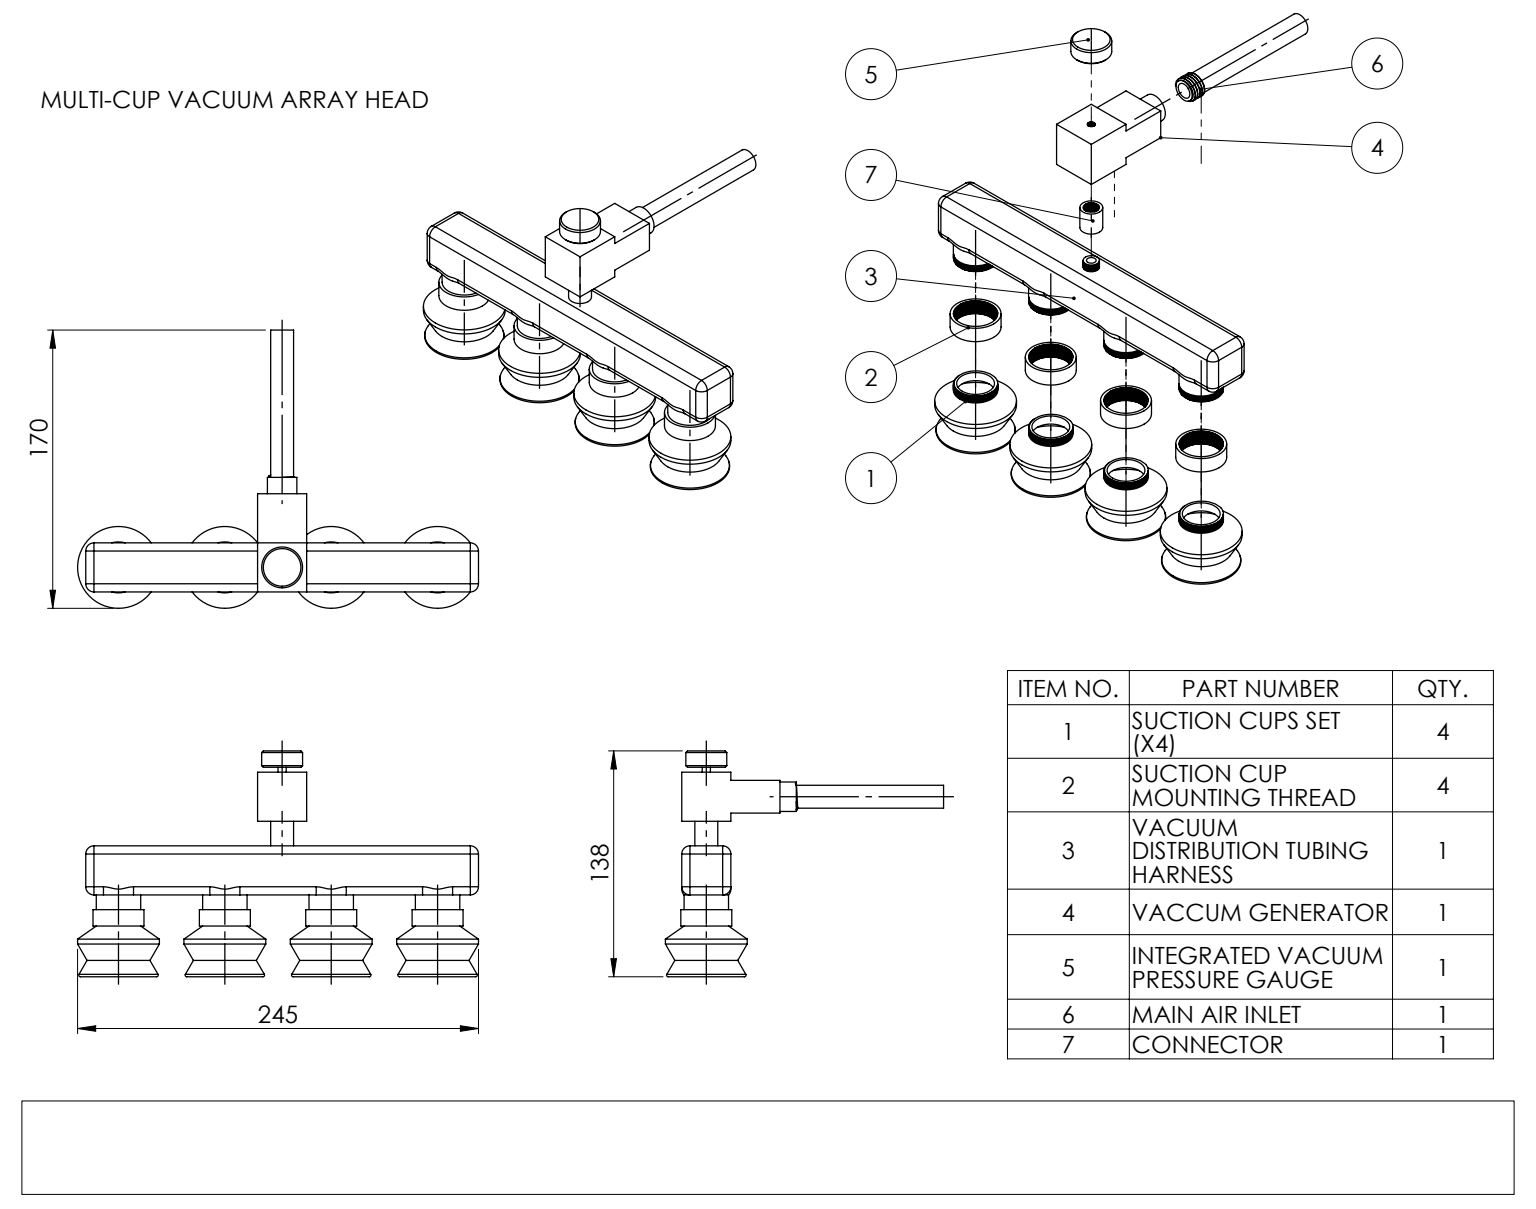
ISO-10303-21;
HEADER;
FILE_DESCRIPTION (('STEP AP214'),
    '1' );
FILE_NAME ('BR-008',
    '2026-10-01T14:18:43',
    ( '' ),
    ( '' ),
    'SwSTEP 2.0',
    'SolidWorks 2026',
    '' );
FILE_SCHEMA (( 'AUTOMOTIVE_DESIGN' ));
ENDSEC;

DATA;
#1 = ORIENTED_EDGE ( 'NONE', *, *, #27439, .T. ) ;
#2 = CARTESIAN_POINT ( 'NONE',  ( 94.99999999999995737, 83.93750000000001421, -2.071067811865491048 ) ) ;
#3 = CARTESIAN_POINT ( 'NONE',  ( 103.1528011352953484, 93.43749999863440792, -3.152801135295366208 ) ) ;
#4 = ORIENTED_EDGE ( 'NONE', *, *, #23222, .F. ) ;
#5 = CARTESIAN_POINT ( 'NONE',  ( 95.67376207875069838, 115.9545556584642867, -49.30000000000000426 ) ) ;
#6 = CARTESIAN_POINT ( 'NONE',  ( 59.55508561352770158, 34.55078125108393294, 13.14518615778179722 ) ) ;
#7 = ORIENTED_EDGE ( 'NONE', *, *, #7284, .F. ) ;
#8 = CARTESIAN_POINT ( 'NONE',  ( 13.57481594606304753, 32.71523437500000142, -5.622872871577873966 ) ) ;
#9 = CARTESIAN_POINT ( 'NONE',  ( 101.8468681455906903, 4.458734125000016313, 4.375000001365592084 ) ) ;
#10 = EDGE_CURVE ( 'NONE', #23304, #14872, #10315, .T. ) ;
#11 = VERTEX_POINT ( 'NONE', #12909 ) ;
#12 = CARTESIAN_POINT ( 'NONE',  ( 13.14518615778179544, 34.00507812608393721, -1.609821015232357215E-15 ) ) ;
#13 = CARTESIAN_POINT ( 'NONE',  ( -5.444914386472299306, 39.31328125108394289, 13.14518615778179722 ) ) ;
#14 = CARTESIAN_POINT ( 'NONE',  ( 185.4011555911795597, 37.22968750216787726, 9.598844408820459861 ) ) ;
#15 = CARTESIAN_POINT ( 'NONE',  ( 5.444914386472302859, 36.83281250108392868, 13.14518615778179189 ) ) ;
#16 = CARTESIAN_POINT ( 'NONE',  ( 94.99999999999995737, 1.387778780781445676E-14, 4.999999999999999112 ) ) ;
#17 = CARTESIAN_POINT ( 'NONE',  ( 198.0446094569239790, 53.89089363584123049, 14.99999999999994671 ) ) ;
#18 = CARTESIAN_POINT ( 'NONE',  ( 143.1451861577818363, 36.43593750108394147, -5.444914386472297529 ) ) ;
#19 = ORIENTED_EDGE ( 'NONE', *, *, #9159, .T. ) ;
#21 = VECTOR ( 'NONE', #21803, 1000.000000000000000 ) ;
#20 = CARTESIAN_POINT ( 'NONE',  ( 13.14518615778179544, 37.97382812608393721, -1.609821015232357215E-15 ) ) ;
#22 = CARTESIAN_POINT ( 'NONE',  ( 143.1451861577818079, 35.39414062608393152, -1.609821015232357215E-15 ) ) ;
#23 = CARTESIAN_POINT ( 'NONE',  ( 65.00000000000000000, 34.84843749999999574, 13.57481594606304576 ) ) ;
#24 = CARTESIAN_POINT ( 'NONE',  ( 130.0000000000000000, -7.395377635281828788, -1.503427012513233026E-14 ) ) ;
#25 = CARTESIAN_POINT ( 'NONE',  ( 95.54126587499996504, 1.387778780781445676E-14, 10.68750000136559208 ) ) ;
#26 = CARTESIAN_POINT ( 'NONE',  ( 99.99999999999998579, 130.0000000000000000, 0.5000000000000034417 ) ) ;
#27 = CARTESIAN_POINT ( 'NONE',  ( 99.99999999999995737, -4.458734124999988779, 1.687500001365591418 ) ) ;
#28 = CARTESIAN_POINT ( 'NONE',  ( 104.9952793366501851, 116.8754121666685393, -49.82500000273120122 ) ) ;
#29 = CARTESIAN_POINT ( 'NONE',  ( -8.312177448680279460E-16, 39.31328125216787583, -13.57481594606304576 ) ) ;
#30 = CARTESIAN_POINT ( 'NONE',  ( 99.99999999999995737, 80.00000000000000000, -1.387778780781445676E-14 ) ) ;
#31 = CARTESIAN_POINT ( 'NONE',  ( 93.46109445667489979, 105.2492070361643215, -47.42499999726882720 ) ) ;
#32 = CARTESIAN_POINT ( 'NONE',  ( -9.295050272127046043, 35.89023437608393152, -9.295050272127046043 ) ) ;
#33 = CARTESIAN_POINT ( 'NONE',  ( 95.00472066334982912, 103.1245878333314323, -47.57499999726882578 ) ) ;
#34 = VERTEX_POINT ( 'NONE', #6384 ) ;
#35 = CARTESIAN_POINT ( 'NONE',  ( 102.0669872999999797, 124.3500000010924822, -9.794112055954760458E-15 ) ) ;
#36 =( BOUNDED_CURVE ( )  B_SPLINE_CURVE ( 2, ( #22936, #3397, #12350, #21068, #12069, #998, #12204, #16222, #18653 ),
 .UNSPECIFIED., .F., .F. ) 
 B_SPLINE_CURVE_WITH_KNOTS ( ( 3, 2, 2, 2, 3 ),
 ( 0.5208333333333332593, 0.5312499999999997780, 0.5416666666666664076, 0.5520833333333330373, 0.5624999999999996669 ),
 .UNSPECIFIED. ) 
 CURVE ( )  GEOMETRIC_REPRESENTATION_ITEM ( )  RATIONAL_B_SPLINE_CURVE ( ( 1.000000000000000888, 0.9238795325112859613, 1.000000000000000000, 0.9238795325112867385, 1.000000000000000000, 0.9238795325112867385, 1.000000000000000000, 0.9238795325112891810, 0.9999999999999975575 ) ) 
 REPRESENTATION_ITEM ( '' )  );
#37 = CARTESIAN_POINT ( 'NONE',  ( 102.0669872999999797, 123.3500000010924680, -9.794112055954760458E-15 ) ) ;
#38 = LINE ( 'NONE', #22552, #12466 ) ;
#39 = CARTESIAN_POINT ( 'NONE',  ( 195.0000000000000000, 37.97382812608393721, -13.14518615778179544 ) ) ;
#40 = ORIENTED_EDGE ( 'NONE', *, *, #17022, .F. ) ;
#41 = CYLINDRICAL_SURFACE ( 'NONE', #26554, 13.57481594606304576 ) ;
#42 = CARTESIAN_POINT ( 'NONE',  ( -13.36000105192242060, 40.87597656304196647, 0.000000000000000000 ) ) ;
#43 = CARTESIAN_POINT ( 'NONE',  ( 104.4587341249999781, -1.846868145590721655, 14.12500000136559208 ) ) ;
#44 = EDGE_CURVE ( 'NONE', #13519, #7822, #26113, .T. ) ;
#45 = ORIENTED_EDGE ( 'NONE', *, *, #19075, .T. ) ;
#46 = CARTESIAN_POINT ( 'NONE',  ( 93.00000000000001421, 112.2744378736303332, -50.10000000000000142 ) ) ;
#47 = AXIS2_PLACEMENT_3D ( 'NONE', #20882, #18604, #27308 ) ;
#48 = CARTESIAN_POINT ( 'NONE',  ( -13.14518615778179900, 40.50390625108394005, -5.444914386472297529 ) ) ;
#49 = CARTESIAN_POINT ( 'NONE',  ( 97.93301269999999192, 123.9000000010924794, -0.8561741729129505041 ) ) ;
#50 = CARTESIAN_POINT ( 'NONE',  ( 143.1451861577818079, 39.31328125108392868, 5.444914386472293977 ) ) ;
#51 = CYLINDRICAL_SURFACE ( 'NONE', #259, 5.000000000000004441 ) ;
#52 = APPLICATION_CONTEXT ( 'automotive_design' ) ;
#53 = CARTESIAN_POINT ( 'NONE',  ( 103.5355339059327235, 93.74999999726881583, 3.535533905932724874 ) ) ;
#54 = CARTESIAN_POINT ( 'NONE',  ( 78.14518615778179367, 39.51171875108392584, 5.444914386472293977 ) ) ;
#55 = FACE_OUTER_BOUND ( 'NONE', #22673, .T. ) ;
#56 = CIRCLE ( 'NONE', #18273, 5.000000000000000000 ) ;
#57 = CARTESIAN_POINT ( 'NONE',  ( 181.8548138422181921, 33.65781250108393152, 5.444914386472304635 ) ) ;
#58 = VERTEX_POINT ( 'NONE', #14643 ) ;
#59 = ORIENTED_EDGE ( 'NONE', *, *, #2461, .T. ) ;
#60 = CARTESIAN_POINT ( 'NONE',  ( -13.14518615778179900, 39.11484375108394573, -5.444914386472297529 ) ) ;
#61 = CARTESIAN_POINT ( 'NONE',  ( 103.1528011352953342, -3.152801135295355106, 10.06250000136559386 ) ) ;
#62 = CARTESIAN_POINT ( 'NONE',  ( 51.85481384221820633, 38.96601562608393721, 0.000000000000000000 ) ) ;
#63 = CARTESIAN_POINT ( 'NONE',  ( 99.99999999999995737, 80.18750000136559208, -4.458734125000016313 ) ) ;
#64 = CARTESIAN_POINT ( 'NONE',  ( 189.5550856135277229, 39.61093750108393152, -13.14518615778179722 ) ) ;
#65 = CARTESIAN_POINT ( 'NONE',  ( -8.049105076161786076E-16, 38.96601562608393721, -13.14518615778179544 ) ) ;
#66 = CARTESIAN_POINT ( 'NONE',  ( 187.8845096081555823, 49.99999999945637796, 11.58166858714721492 ) ) ;
#67 =( BOUNDED_CURVE ( )  B_SPLINE_CURVE ( 2, ( #19739, #26449, #6767, #8908, #2228, #15452, #13444, #6906, #10892, #17316, #24023, #2505, #15595, #2083, #2648, #15160, #20032, #19600, #512, #9193, #17887, #26593, #10752, #19463, #28160, #8627, #4357, #13014, #83, #8766, #26155, #15308, #18836, #13875, #8143, #13592, #5879, #15877, #16700, #11735, #22314, #20460, #11453, #942, #10262, #12398, #21119, #26883, #22601, #3070, #26736, #2788, #23265, #20986, #13733, #1606, #24872, #14549, #18972, #27680, #27543, #16017, #5355, #24587, #4929, #7329, #18022, #20174, #9613, #9328, #8000, #3738, #7180, #1467, #25399, #5069, #16837, #655, #16165, #22457, #2923, #10123, #18316, #14410, #27025, #11593, #20313, #7470, #800, #9469, #23126, #18171, #3601, #24731, #5211, #12261, #10683, #8842, #23398, #23956, #8558 ),
 .UNSPECIFIED., .F., .F. ) 
 B_SPLINE_CURVE_WITH_KNOTS ( ( 3, 2, 2, 2, 2, 2, 2, 2, 2, 2, 2, 2, 2, 2, 2, 2, 2, 2, 2, 2, 2, 2, 2, 2, 2, 2, 2, 2, 2, 2, 2, 2, 2, 2, 2, 2, 2, 2, 2, 2, 2, 2, 2, 2, 2, 2, 2, 2, 2, 2, 3 ),
 ( 0.000000000000000000, 0.02000000000000000042, 0.04000000000000000083, 0.05999999999999999778, 0.08000000000000000167, 0.1000000000000000056, 0.1199999999999999956, 0.1400000000000000133, 0.1600000000000000033, 0.1799999999999999933, 0.2000000000000000111, 0.2200000000000000011, 0.2399999999999999911, 0.2600000000000000089, 0.2800000000000000266, 0.2999999999999999889, 0.3200000000000000067, 0.3400000000000000244, 0.3599999999999999867, 0.3800000000000000044, 0.4000000000000000222, 0.4199999999999999845, 0.4400000000000000022, 0.4600000000000000200, 0.4799999999999999822, 0.5000000000000000000, 0.5200000000000000178, 0.5400000000000000355, 0.5600000000000000533, 0.5799999999999999600, 0.5999999999999999778, 0.6199999999999999956, 0.6400000000000000133, 0.6600000000000000311, 0.6800000000000000488, 0.6999999999999999556, 0.7199999999999999734, 0.7399999999999999911, 0.7600000000000000089, 0.7800000000000000266, 0.8000000000000000444, 0.8199999999999999512, 0.8399999999999999689, 0.8599999999999999867, 0.8800000000000000044, 0.9000000000000000222, 0.9200000000000000400, 0.9399999999999999467, 0.9599999999999999645, 0.9799999999999999822, 1.000000000000000000 ),
 .UNSPECIFIED. ) 
 CURVE ( )  GEOMETRIC_REPRESENTATION_ITEM ( )  RATIONAL_B_SPLINE_CURVE ( ( 1.000000000000000000, 0.9510565162951535312, 1.000000000000000000, 0.9510565162951535312, 1.000000000000000000, 0.9510565162951535312, 1.000000000000000000, 0.9510565162951535312, 1.000000000000000000, 0.9510565162951535312, 1.000000000000000000, 0.9510565162951535312, 1.000000000000000000, 0.9510565162951535312, 1.000000000000000000, 0.9510565162951535312, 1.000000000000000000, 0.9510565162951535312, 1.000000000000000000, 0.9510565162951535312, 1.000000000000000000, 0.9510565162951535312, 1.000000000000000000, 0.9510565162951535312, 1.000000000000000000, 0.9510565162951535312, 1.000000000000000000, 0.9510565162951535312, 1.000000000000000000, 0.9510565162951535312, 1.000000000000000000, 0.9510565162951535312, 1.000000000000000000, 0.9510565162951535312, 1.000000000000000000, 0.9510565162951535312, 1.000000000000000000, 0.9510565162951535312, 1.000000000000000000, 0.9510565162951535312, 1.000000000000000000, 0.9510565162951535312, 1.000000000000000000, 0.9510565162951535312, 1.000000000000000000, 0.9510565162951535312, 1.000000000000000000, 0.9510565162951535312, 1.000000000000000000, 0.9510565162951535312, 1.000000000000000000, 0.9510565162951535312, 1.000000000000000000, 0.9510565162951535312, 1.000000000000000000, 0.9510565162951535312, 1.000000000000000000, 0.9510565162951535312, 1.000000000000000000, 0.9510565162951535312, 1.000000000000000000, 0.9510565162951535312, 1.000000000000000000, 0.9510565162951535312, 1.000000000000000000, 0.9510565162951535312, 1.000000000000000000, 0.9510565162951535312, 1.000000000000000000, 0.9510565162951535312, 1.000000000000000000, 0.9510565162951535312, 1.000000000000000000, 0.9510565162951535312, 1.000000000000000000, 0.9510565162951535312, 1.000000000000000000, 0.9510565162951535312, 1.000000000000000000, 0.9510565162951535312, 1.000000000000000000, 0.9510565162951535312, 1.000000000000000000, 0.9510565162951535312, 1.000000000000000000, 0.9510565162951535312, 1.000000000000000000, 0.9510565162951535312, 1.000000000000000000, 0.9510565162951535312, 1.000000000000000000, 0.9510565162951535312, 1.000000000000000000, 0.9510565162951535312, 1.000000000000000000, 0.9510565162951535312, 1.000000000000000000, 0.9510565162951535312, 1.000000000000000000, 0.9510565162951535312, 1.000000000000000000 ) ) 
 REPRESENTATION_ITEM ( '' )  );
#68 = CARTESIAN_POINT ( 'NONE',  ( 2.493653234604083739E-15, 38.02343749999999289, 13.57481594606304576 ) ) ;
#69 = CARTESIAN_POINT ( 'NONE',  ( 97.50236033167490746, 102.3130555110000159, -55.22499999726881725 ) ) ;
#70 = ORIENTED_EDGE ( 'NONE', *, *, #20702, .F. ) ;
#71 = EDGE_CURVE ( 'NONE', #7474, #9199, #1741, .T. ) ;
#72 = CARTESIAN_POINT ( 'NONE',  ( 13.57481594606304931, 38.17226562499999432, 5.622872871577869525 ) ) ;
#73 = CARTESIAN_POINT ( 'NONE',  ( 5.444914386472297529, 37.92421875108392726, -13.14518615778179900 ) ) ;
#74 = CARTESIAN_POINT ( 'NONE',  ( 99.99999999999995737, -4.999999999999990230, 1.375000002731184612 ) ) ;
#75 = CARTESIAN_POINT ( 'NONE',  ( 143.1451861577818079, 34.79882812608394005, -1.609821015232357215E-15 ) ) ;
#76 = CARTESIAN_POINT ( 'NONE',  ( 59.55508561352770158, 32.76484375108393010, 13.14518615778179722 ) ) ;
#77 = CARTESIAN_POINT ( 'NONE',  ( 208.1451861577817795, 38.71796875108393721, 5.444914386472293977 ) ) ;
#78 = CARTESIAN_POINT ( 'NONE',  ( 9.295050272127047819, 32.91367187608393152, 9.295050272127046043 ) ) ;
#79 = CARTESIAN_POINT ( 'NONE',  ( 134.5715916325255250, 51.44262710532316873, -14.99999999999934452 ) ) ;
#80 = EDGE_CURVE ( 'NONE', #16509, #7689, #8629, .T. ) ;
#81 = CARTESIAN_POINT ( 'NONE',  ( 99.99999999999998579, 110.0000000000000000, -145.0000000000000284 ) ) ;
#82 = CARTESIAN_POINT ( 'NONE',  ( -9.180175813647991845, 50.00000000000000000, 9.999999999999998224 ) ) ;
#83 = CARTESIAN_POINT ( 'NONE',  ( 93.46109445667491400, 114.7507929638356785, -51.32500000273120122 ) ) ;
#84 = EDGE_CURVE ( 'NONE', #861, #22018, #1572, .T. ) ;
#85 = CARTESIAN_POINT ( 'NONE',  ( 13.14518615778179544, 33.80664062608393294, -1.609821015232357215E-15 ) ) ;
#86 = CARTESIAN_POINT ( 'NONE',  ( 84.99999999999998579, 100.0000000000000000, -15.00000000000000533 ) ) ;
#87 = CARTESIAN_POINT ( 'NONE',  ( 101.7677669529663547, 123.8000000021849587, 1.767766952966350891 ) ) ;
#88 = EDGE_CURVE ( 'NONE', #26327, #25494, #13051, .T. ) ;
#89 = CARTESIAN_POINT ( 'NONE',  ( -5.622872871577804688, 36.48554687716787726, 13.57481594606311504 ) ) ;
#90 = SURFACE_STYLE_USAGE ( .BOTH. , #4222 ) ;
#91 = CARTESIAN_POINT ( 'NONE',  ( 98.15313185440925281, 4.458734125000016313, 7.250000001365591196 ) ) ;
#92 = ORIENTED_EDGE ( 'NONE', *, *, #1447, .F. ) ;
#93 = CARTESIAN_POINT ( 'NONE',  ( 102.0669872999999797, 122.5500000010924850, -9.794112055954760458E-15 ) ) ;
#94 = CARTESIAN_POINT ( 'NONE',  ( 101.8468681455906903, -4.458734124999987891, 10.75000000136559208 ) ) ;
#95 = LINE ( 'NONE', #11320, #20973 ) ;
#96 = ADVANCED_FACE ( 'NONE', ( #24479 ), #13627, .T. ) ;
#97 = CARTESIAN_POINT ( 'NONE',  ( 13.14518615778179544, 38.56914062608393579, -1.609821015232357215E-15 ) ) ;
#98 = CARTESIAN_POINT ( 'NONE',  ( 120.4011555911795455, 38.61875000216787157, -9.598844408820458085 ) ) ;
#99 = CARTESIAN_POINT ( 'NONE',  ( 103.1528011352953342, 80.06250000136559208, 3.152801135295355106 ) ) ;
#100 = CARTESIAN_POINT ( 'NONE',  ( 78.14518615778179367, 34.05468750108394005, -5.444914386472297529 ) ) ;
#101 = CARTESIAN_POINT ( 'NONE',  ( 108.0825317500000011, 112.6261737610028320, -50.02500000273118275 ) ) ;
#102 = CARTESIAN_POINT ( 'NONE',  ( 103.5355339059327093, 3.535533905932755072, 11.62500000000000000 ) ) ;
#103 = CARTESIAN_POINT ( 'NONE',  ( 214.9999999999999716, 80.00000000000000000, 9.999999999999946709 ) ) ;
#104 = CARTESIAN_POINT ( 'NONE',  ( 95.54126587499996504, 1.387778780781445676E-14, 0.6875000013655923059 ) ) ;
#105 = CARTESIAN_POINT ( 'NONE',  ( 143.5748159460630404, 39.06523437499998863, -5.622872871577873077 ) ) ;
#106 = ORIENTED_EDGE ( 'NONE', *, *, #13267, .T. ) ;
#107 = DIRECTION ( 'NONE',  ( -1.000000000000000000, 0.000000000000000000, 0.000000000000000000 ) ) ;
#108 = CARTESIAN_POINT ( 'NONE',  ( 9.295050272127046043, 38.07304687608393579, -9.295050272127046043 ) ) ;
#109 = CARTESIAN_POINT ( 'NONE',  ( -5.622872871577873077, 36.18789062716787441, -13.57481594606304753 ) ) ;
#110 = CARTESIAN_POINT ( 'NONE',  ( 143.1451861577818079, 37.82500000108392868, -5.444914386472297529 ) ) ;
#111 = CARTESIAN_POINT ( 'NONE',  ( 51.42518405393695957, 33.16171875216787868, 0.000000000000000000 ) ) ;
#112 = EDGE_CURVE ( 'NONE', #21487, #10978, #25380, .T. ) ;
#113 = DIRECTION ( 'NONE',  ( 0.000000000000000000, 0.000000000000000000, 1.000000000000000000 ) ) ;
#114 = CARTESIAN_POINT ( 'NONE',  ( 13.57481594606304931, 32.71523437716787441, 5.622872871577869525 ) ) ;
#115 = CARTESIAN_POINT ( 'NONE',  ( 102.0710678118654329, 5.000000000000018652, 4.687500000000000000 ) ) ;
#116 = EDGE_CURVE ( 'NONE', #24967, #25660, #21271, .T. ) ;
#117 = CARTESIAN_POINT ( 'NONE',  ( 185.7049497278729575, 34.10429687608393579, -9.295050272127046043 ) ) ;
#118 = EDGE_CURVE ( 'NONE', #27220, #19908, #1908, .T. ) ;
#119 = VECTOR ( 'NONE', #9370, 1000.000000000000000 ) ;
#120 = CARTESIAN_POINT ( 'NONE',  ( 104.9999999999999716, 92.93749999999998579, 2.071067811865467956 ) ) ;
#121 = CARTESIAN_POINT ( 'NONE',  ( 181.4251840539369596, 37.97382812716787726, 5.622872871577880183 ) ) ;
#122 = LINE ( 'NONE', #8807, #24532 ) ;
#123 = CARTESIAN_POINT ( 'NONE',  ( 92.99999999999998579, 110.0000000000000000, -48.49999999453763877 ) ) ;
#124 = CARTESIAN_POINT ( 'NONE',  ( 13.57481594606304576, 37.42812499999999432, -1.662435489736055892E-15 ) ) ;
#125 = CARTESIAN_POINT ( 'NONE',  ( 99.99999999999998579, 117.3602355696678643, -54.50000000000000000 ) ) ;
#126 = CARTESIAN_POINT ( 'NONE',  ( 5.444914386472297529, 36.53515625108393294, -13.14518615778179900 ) ) ;
#127 = CARTESIAN_POINT ( 'NONE',  ( 5.444914386472302859, 36.03906250108394005, 13.14518615778179189 ) ) ;
#128 = CARTESIAN_POINT ( 'NONE',  ( 195.0000000000000000, 35.24531249999999716, -13.57481594606304576 ) ) ;
#129 = CARTESIAN_POINT ( 'NONE',  ( 106.5389055433251002, 105.2492070361643215, -44.57500000273119412 ) ) ;
#130 = CARTESIAN_POINT ( 'NONE',  ( 104.3262379212492590, 115.9545556584642867, -45.20000000546237828 ) ) ;
#131 = CARTESIAN_POINT ( 'NONE',  ( 59.55508561352770158, 35.14609375108393152, 13.14518615778179722 ) ) ;
#132 = CARTESIAN_POINT ( 'NONE',  ( 104.4587341249999781, 1.846868145590750521, 4.000000001365592084 ) ) ;
#133 = CARTESIAN_POINT ( 'NONE',  ( 102.1631189606246295, 116.6573956140660897, -45.10000000546238397 ) ) ;
#134 = CARTESIAN_POINT ( 'NONE',  ( 98.15313185440925281, 94.99999999863439371, 4.458734124999979898 ) ) ;
#135 = CARTESIAN_POINT ( 'NONE',  ( 97.93294022916485631, 122.9999999999999858, -0.1348184704668160261 ) ) ;
#136 = CARTESIAN_POINT ( 'NONE',  ( 13.57481594606304753, 36.68398437499999432, -5.622872871577873077 ) ) ;
#137 = CARTESIAN_POINT ( 'NONE',  ( 130.0000000000000000, 36.58476562608393579, -13.14518615778179544 ) ) ;
#138 = VERTEX_POINT ( 'NONE', #3105 ) ;
#139 = ORIENTED_EDGE ( 'NONE', *, *, #6013, .F. ) ;
#140 = CARTESIAN_POINT ( 'NONE',  ( 99.99999999999995737, 84.75000000000000000, -5.000000000000018652 ) ) ;
#141 = CARTESIAN_POINT ( 'NONE',  ( 94.99999999999995737, 82.06250000273119838, -2.071067811865491048 ) ) ;
#142 = CARTESIAN_POINT ( 'NONE',  ( 96.84719886470463734, 92.93749999863440792, 3.152801135295351997 ) ) ;
#143 = CARTESIAN_POINT ( 'NONE',  ( 9.598844408820456309, 34.35234374999999574, -9.598844408820458085 ) ) ;
#144 = VERTEX_POINT ( 'NONE', #11771 ) ;
#145 = AXIS2_PLACEMENT_3D ( 'NONE', #183, #21567, #25834 ) ;
#146 = CARTESIAN_POINT ( 'NONE',  ( 99.99999999999997158, 102.6397644303321215, -52.50000000000000711 ) ) ;
#147 = CARTESIAN_POINT ( 'NONE',  ( 70.44491438647230552, 33.85625000108393579, 13.14518615778179189 ) ) ;
#148 = ORIENTED_EDGE ( 'NONE', *, *, #16828, .T. ) ;
#149 = CARTESIAN_POINT ( 'NONE',  ( -8.312177448680279460E-16, 32.96328125216787441, -13.57481594606304576 ) ) ;
#150 = CARTESIAN_POINT ( 'NONE',  ( 101.8468681455906903, -4.458734124999987891, 3.000000001365592528 ) ) ;
#151 = EDGE_CURVE ( 'NONE', #14316, #1074, #18349, .T. ) ;
#152 = VERTEX_POINT ( 'NONE', #22777 ) ;
#153 = CARTESIAN_POINT ( 'NONE',  ( 94.99999999999995737, 82.18750000273119838, 2.071067811865466624 ) ) ;
#154 = CARTESIAN_POINT ( 'NONE',  ( 13.14518615778179544, 38.76757812608393294, -1.609821015232357215E-15 ) ) ;
#155 = UNCERTAINTY_MEASURE_WITH_UNIT (LENGTH_MEASURE( 1.000000000000000082E-05 ), #20072, 'distance_accuracy_value', 'NONE');
#156 = CARTESIAN_POINT ( 'NONE',  ( 208.5748159460630120, 35.09648437716787583, 5.622872871577869525 ) ) ;
#157 =( BOUNDED_CURVE ( )  B_SPLINE_CURVE ( 2, ( #25854, #26427, #8886, #8604, #23721, #4618, #22006, #19716, #2060, #6886, #24002, #4059, #2483, #19859, #12721, #10593, #17292, #17435, #26134, #346, #10730, #19438, #6600, #9033, #21447, #25994, #1925, #6465, #15139, #2204, #10868, #19578, #62, #5047, #2628, #15857, #775, #22576, #24851, #11571, #920, #7307, #13712, #7161, #13851, #491, #24419, #5188, #9172, #22433, #27146, #631, #15994, #4908, #9447, #11713, #24566, #3045, #9307, #11289, #17864, #20289, #22720, #26569, #9590, #18004, #2902, #24709, #20438, #7598, #18294, #7021, #27000, #7447, #16143, #22292, #24280, #5330, #4761, #13994, #3187, #13569, #11857, #20579, #2768, #26861, #18147, #1062, #15716, #9732, #18437, #13421, #11432 ),
 .UNSPECIFIED., .F., .F. ) 
 B_SPLINE_CURVE_WITH_KNOTS ( ( 3, 2, 2, 2, 2, 2, 2, 2, 2, 2, 2, 2, 2, 2, 2, 2, 2, 2, 2, 2, 2, 2, 2, 2, 2, 2, 2, 2, 2, 2, 2, 2, 2, 2, 2, 2, 2, 2, 2, 2, 2, 2, 2, 2, 2, 2, 3 ),
 ( 0.000000000000000000, 0.01041666666666666609, 0.02083333333333333218, 0.03125000000000000000, 0.04166666666666666435, 0.05208333333333333565, 0.06250000000000000000, 0.07291666666666667129, 0.08333333333333332871, 0.09375000000000000000, 0.1041666666666666713, 0.1145833333333333287, 0.1250000000000000000, 0.1354166666666666574, 0.1458333333333333426, 0.1562500000000000278, 0.1666666666666666574, 0.1770833333333333426, 0.1875000000000000000, 0.1979166666666666574, 0.2083333333333333426, 0.2187499999999999722, 0.2291666666666666574, 0.2395833333333333426, 0.2500000000000000000, 0.2604166666666666852, 0.2708333333333333148, 0.2812500000000000000, 0.2916666666666666852, 0.3020833333333333148, 0.3125000000000000555, 0.3229166666666666852, 0.3333333333333333148, 0.3437500000000000000, 0.3541666666666666852, 0.3645833333333333148, 0.3750000000000000000, 0.3854166666666666852, 0.3958333333333333148, 0.4062500000000000000, 0.4166666666666666852, 0.4270833333333333148, 0.4374999999999999445, 0.4479166666666666852, 0.4583333333333333148, 0.4687500000000000000, 0.4779971559588573893 ),
 .UNSPECIFIED. ) 
 CURVE ( )  GEOMETRIC_REPRESENTATION_ITEM ( )  RATIONAL_B_SPLINE_CURVE ( ( 1.000000000000000000, 0.9238795325112867385, 1.000000000000000000, 0.9238795325112867385, 1.000000000000000000, 0.9238795325112867385, 1.000000000000000000, 0.9238795325112867385, 1.000000000000000000, 0.9238795325112867385, 1.000000000000000000, 0.9238795325112867385, 1.000000000000000000, 0.9238795325112867385, 1.000000000000000000, 0.9238795325112867385, 1.000000000000000000, 0.9238795325112867385, 1.000000000000000000, 0.9238795325112867385, 1.000000000000000000, 0.9238795325112867385, 1.000000000000000000, 0.9238795325112867385, 1.000000000000000000, 0.9238795325112867385, 1.000000000000000000, 0.9238795325112867385, 1.000000000000000000, 0.9238795325112867385, 1.000000000000000000, 0.9238795325112867385, 1.000000000000000000, 0.9238795325112867385, 1.000000000000000000, 0.9238795325112867385, 1.000000000000000000, 0.9238795325112867385, 1.000000000000000000, 0.9238795325112867385, 1.000000000000000000, 0.9238795325112867385, 1.000000000000000000, 0.9238795325112867385, 1.000000000000000000, 0.9238795325112867385, 1.000000000000000000, 0.9238795325112867385, 1.000000000000000000, 0.9238795325112867385, 1.000000000000000000, 0.9238795325112867385, 1.000000000000000000, 0.9238795325112867385, 1.000000000000000000, 0.9238795325112867385, 1.000000000000000000, 0.9238795325112867385, 1.000000000000000000, 0.9238795325112867385, 1.000000000000000000, 0.9238795325112867385, 1.000000000000000000, 0.9238795325112867385, 1.000000000000000000, 0.9238795325112867385, 1.000000000000000000, 0.9238795325112867385, 1.000000000000000000, 0.9238795325112867385, 1.000000000000000000, 0.9238795325112867385, 1.000000000000000000, 0.9238795325112867385, 1.000000000000000000, 0.9238795325112867385, 1.000000000000000000, 0.9238795325112867385, 1.000000000000000000, 0.9238795325112867385, 1.000000000000000000, 0.9238795325112867385, 1.000000000000000000, 0.9238795325112867385, 1.000000000000000000, 0.9238795325112867385, 1.000000000000000000, 0.9238795325112867385, 1.000000000000000000, 0.9238795325112867385, 1.000000000000000000, 0.9324258078851906939, 0.9848264816800322841 ) ) 
 REPRESENTATION_ITEM ( '' )  );
#158 = CARTESIAN_POINT ( 'NONE',  ( -9.295050272127046043, 36.48554687608393721, -9.295050272127046043 ) ) ;
#159 = CARTESIAN_POINT ( 'NONE',  ( 103.5355338419364699, 95.00000000000001421, -3.535533969929001596 ) ) ;
#160 = EDGE_CURVE ( 'NONE', #17655, #15436, #3245, .T. ) ;
#161 = CARTESIAN_POINT ( 'NONE',  ( 204.5988444088204687, 39.80937500216786873, 9.598844408820456309 ) ) ;
#162 = VERTEX_POINT ( 'NONE', #19320 ) ;
#163 = CARTESIAN_POINT ( 'NONE',  ( -13.14518615778179189, 36.83281250108393579, 5.444914386472304635 ) ) ;
#164 = CARTESIAN_POINT ( 'NONE',  ( 130.0000000000000000, 36.38632812608393152, -13.14518615778179544 ) ) ;
#165 = CARTESIAN_POINT ( 'NONE',  ( 65.00000000000000000, 35.64218749999999147, 13.57481594606304576 ) ) ;
#166 = CARTESIAN_POINT ( 'NONE',  ( 9.598844408820456309, 38.42031250216787441, -9.598844408820458085 ) ) ;
#167 = CARTESIAN_POINT ( 'NONE',  ( 96.84719886470459471, -3.152801135295355994, 12.81250000136559208 ) ) ;
#169 = CARTESIAN_POINT ( 'NONE',  ( 195.0000000000000000, 37.22968749999999716, 13.57481594606304576 ) ) ;
#168 = AXIS2_PLACEMENT_3D ( 'NONE', #6488, #12746, #4083 ) ;
#170 = CARTESIAN_POINT ( 'NONE',  ( 103.1528011352953342, -3.152801135295355106, 0.8125000013655924169 ) ) ;
#171 = CARTESIAN_POINT ( 'NONE',  ( 93.46109445667491400, 114.7507929638356785, -51.32500000273120122 ) ) ;
#172 = CARTESIAN_POINT ( 'NONE',  ( 103.1528011352953342, -3.152801135295355106, 1.062500001365592528 ) ) ;
#173 = DIRECTION ( 'NONE',  ( 1.000000000000000000, 0.000000000000000000, 0.000000000000000000 ) ) ;
#174 = CARTESIAN_POINT ( 'NONE',  ( 99.99999999999997158, 118.4984768113314146, -52.12499999726881583 ) ) ;
#175 = CARTESIAN_POINT ( 'NONE',  ( -13.14518615778179900, 36.73359375108393010, -5.444914386472297529 ) ) ;
#176 = CARTESIAN_POINT ( 'NONE',  ( 106.5389055433250860, 114.7507929638356785, -50.67499999726882010 ) ) ;
#177 = ORIENTED_EDGE ( 'NONE', *, *, #19574, .T. ) ;
#178 = CARTESIAN_POINT ( 'NONE',  ( 101.4615807364564546, 124.2500000010924737, 1.461580736456455476 ) ) ;
#179 = CARTESIAN_POINT ( 'NONE',  ( 84.99999999999998579, 120.0000000000000000, -45.00000000000000711 ) ) ;
#180 = LINE ( 'NONE', #8862, #20235 ) ;
#181 = CARTESIAN_POINT ( 'NONE',  ( 185.7049497278729575, 38.27148437608393294, 9.295050272127047819 ) ) ;
#182 = EDGE_LOOP ( 'NONE', ( #354, #23980, #3469, #3062 ) ) ;
#183 = CARTESIAN_POINT ( 'NONE',  ( 0.000000000000000000, -7.395377635281828788, 0.000000000000000000 ) ) ;
#184 = CARTESIAN_POINT ( 'NONE',  ( 189.6826484225240677, 54.47013368152370560, -15.00000000000000000 ) ) ;
#185 = CARTESIAN_POINT ( 'NONE',  ( 143.5748159460630688, 39.85898437499999858, -5.622872871577873966 ) ) ;
#186 = ORIENTED_EDGE ( 'NONE', *, *, #18586, .T. ) ;
#187 = CARTESIAN_POINT ( 'NONE',  ( 97.83688103937538472, 116.6573956140660897, -48.40000000000000568 ) ) ;
#188 = CARTESIAN_POINT ( 'NONE',  ( 130.0000000000000000, 37.62656249999999858, -13.57481594606304576 ) ) ;
#189 = FACE_OUTER_BOUND ( 'NONE', #22000, .T. ) ;
#190 = CARTESIAN_POINT ( 'NONE',  ( 130.0000000000000000, 31.37578125216787583, -13.57481594606304576 ) ) ;
#191 = CARTESIAN_POINT ( 'NONE',  ( 13.14518615778179722, 40.30546875108393579, 5.444914386472293977 ) ) ;
#192 = CARTESIAN_POINT ( 'NONE',  ( 95.00000000000000000, 93.31249999726880162, -2.071067811865479058 ) ) ;
#193 = CARTESIAN_POINT ( 'NONE',  ( 51.85481384221820633, 37.57695312608393579, 0.000000000000000000 ) ) ;
#194 = CARTESIAN_POINT ( 'NONE',  ( 92.99999999999998579, 110.0000000000000000, -145.0000000000000284 ) ) ;
#195 = CARTESIAN_POINT ( 'NONE',  ( 189.5550856135277229, 36.13828125108393863, 13.14518615778179722 ) ) ;
#196 = ORIENTED_EDGE ( 'NONE', *, *, #21889, .T. ) ;
#197 =( BOUNDED_CURVE ( )  B_SPLINE_CURVE ( 2, ( #21878, #15145, #8893, #6748, #2489, #2066, #15434, #19866, #10736 ),
 .UNSPECIFIED., .F., .F. ) 
 B_SPLINE_CURVE_WITH_KNOTS ( ( 3, 2, 2, 2, 3 ),
 ( 0.1041666666666664909, 0.1145833333333332732, 0.1250000000000000833, 0.1354166666666668517, 0.1458333333333336757 ),
 .UNSPECIFIED. ) 
 CURVE ( )  GEOMETRIC_REPRESENTATION_ITEM ( )  RATIONAL_B_SPLINE_CURVE ( ( 1.000000000000001332, 0.9238795325112854062, 1.000000000000000000, 0.9238795325112867385, 1.000000000000000000, 0.9238795325112867385, 1.000000000000000000, 0.9238795325112842960, 1.000000000000002442 ) ) 
 REPRESENTATION_ITEM ( '' )  );
#198 = ORIENTED_EDGE ( 'NONE', *, *, #2542, .F. ) ;
#199 = CARTESIAN_POINT ( 'NONE',  ( -13.14518615778179544, 37.57695312608393579, 0.000000000000000000 ) ) ;
#200 = PRODUCT_CONTEXT ( 'NONE', #23898, 'mechanical' ) ;
#201 = CARTESIAN_POINT ( 'NONE',  ( 104.4587341249999781, -1.846868145590721655, 11.12500000136559208 ) ) ;
#202 = CARTESIAN_POINT ( 'NONE',  ( 101.8468681455907046, 80.12500000136560629, -4.458734125000016313 ) ) ;
#203 = CARTESIAN_POINT ( 'NONE',  ( 208.1451861577818079, 38.61875000108392442, -5.444914386472297529 ) ) ;
#204 = CARTESIAN_POINT ( 'NONE',  ( -9.295050272127046043, 36.68398437608393436, -9.295050272127046043 ) ) ;
#205 = ADVANCED_FACE ( 'NONE', ( #10326 ), #4081, .F. ) ;
#206 = CARTESIAN_POINT ( 'NONE',  ( 186.5976842187810973, 54.99999999484811752, 14.99999999999995026 ) ) ;
#207 = CARTESIAN_POINT ( 'NONE',  ( 103.5355339059327093, -3.535533905932726206, 12.37499999999999822 ) ) ;
#208 = DIRECTION ( 'NONE',  ( 0.000000000000000000, 0.000000000000000000, 1.000000000000000000 ) ) ;
#209 = CARTESIAN_POINT ( 'NONE',  ( 99.99999999999997158, 118.4984768113314004, -52.12499999726880873 ) ) ;
#210 = VERTEX_POINT ( 'NONE', #12459 ) ;
#211 = CARTESIAN_POINT ( 'NONE',  ( -8.312177448680279460E-16, 36.83281249999999574, -13.57481594606304576 ) ) ;
#212 = CARTESIAN_POINT ( 'NONE',  ( -13.14518615778179900, 38.12265625108393152, -5.444914386472297529 ) ) ;
#213 = ORIENTED_EDGE ( 'NONE', *, *, #13961, .F. ) ;
#214 = CARTESIAN_POINT ( 'NONE',  ( 116.8548138422182063, 35.93984375108393436, -5.444914386472297529 ) ) ;
#215 = CARTESIAN_POINT ( 'NONE',  ( 78.14518615778179367, 33.75703125108393010, 5.444914386472293977 ) ) ;
#216 = CARTESIAN_POINT ( 'NONE',  ( 189.5550856135277229, 35.84062500108394289, -13.14518615778179900 ) ) ;
#217 = ORIENTED_EDGE ( 'NONE', *, *, #21157, .F. ) ;
#218 = CARTESIAN_POINT ( 'NONE',  ( 66.13716782454086740, 35.99999999999998579, 13.09590655363602707 ) ) ;
#219 = FILL_AREA_STYLE ('',( #13008 ) ) ;
#220 = FACE_OUTER_BOUND ( 'NONE', #12562, .T. ) ;
#221 = DIRECTION ( 'NONE',  ( 1.000000000000000000, 0.000000000000000000, 0.000000000000000000 ) ) ;
#222 = CARTESIAN_POINT ( 'NONE',  ( 65.00000000000000000, 40.40468749999999432, 13.57481594606304576 ) ) ;
#223 = CARTESIAN_POINT ( 'NONE',  ( 92.99999999999998579, 110.0000000000000000, -45.00000000000001421 ) ) ;
#224 = CYLINDRICAL_SURFACE ( 'NONE', #5646, 2.500000000000008882 ) ;
#225 = CARTESIAN_POINT ( 'NONE',  ( 97.50000000000000000, 124.3184775928351655, 0.3826834323650784575 ) ) ;
#226 = CARTESIAN_POINT ( 'NONE',  ( 61.88530225446237409, 53.90847045361019241, 14.99999999999997868 ) ) ;
#227 = VECTOR ( 'NONE', #13588, 1000.000000000000000 ) ;
#228 =( NAMED_UNIT ( * ) PLANE_ANGLE_UNIT ( ) SI_UNIT ( $, .RADIAN. ) );
#229 = CARTESIAN_POINT ( 'NONE',  ( 95.54126587499995082, 1.846868145590750077, 10.37500000136559208 ) ) ;
#230 = CARTESIAN_POINT ( 'NONE',  ( 101.0355339059327378, 122.4500000021849502, -2.499999999999997780 ) ) ;
#231 = CARTESIAN_POINT ( 'NONE',  ( 95.54126587499995082, -1.846868145590724986, 13.50000000136559208 ) ) ;
#232 = CARTESIAN_POINT ( 'NONE',  ( 131.8143553545780264, 51.46618445021973542, 14.99999999999996625 ) ) ;
#233 = CARTESIAN_POINT ( 'NONE',  ( 5.444914386472297529, 38.71796875108393721, -13.14518615778179900 ) ) ;
#234 = PLANE ( 'NONE',  #26801 ) ;
#235 = CARTESIAN_POINT ( 'NONE',  ( 95.54126587499995082, 80.62500000136559208, -1.846868145590750077 ) ) ;
#236 = CARTESIAN_POINT ( 'NONE',  ( 65.00000000000000000, 35.39414062608393863, 13.14518615778179544 ) ) ;
#237 = CARTESIAN_POINT ( 'NONE',  ( 91.91746824999998466, 107.3738262389971538, -51.02500000273119696 ) ) ;
#238 = CARTESIAN_POINT ( 'NONE',  ( -5.444914386472297529, 36.43593750108394147, -13.14518615778179722 ) ) ;
#239 = EDGE_CURVE ( 'NONE', #2183, #6189, #25460, .T. ) ;
#240 = FACE_OUTER_BOUND ( 'NONE', #19523, .T. ) ;
#241 = CARTESIAN_POINT ( 'NONE',  ( 116.4251840539369596, 40.65273437608393436, 0.000000000000000000 ) ) ;
#242 = CARTESIAN_POINT ( 'NONE',  ( 1.662435489736055892E-15, 40.99999999999999289, 13.57481594606304576 ) ) ;
#243 = CARTESIAN_POINT ( 'NONE',  ( 130.0000000000000000, 38.81718749999999574, 13.57481594606304576 ) ) ;
#244 = ORIENTED_EDGE ( 'NONE', *, *, #571, .T. ) ;
#245 = CARTESIAN_POINT ( 'NONE',  ( 112.9999999999999858, 120.0000000000000000, -43.00000000000000000 ) ) ;
#246 = EDGE_CURVE ( 'NONE', #18432, #1781, #20836, .T. ) ;
#247 = CARTESIAN_POINT ( 'NONE',  ( 9.295050272127046043, 35.69179687608394147, -9.295050272127046043 ) ) ;
#248 = CARTESIAN_POINT ( 'NONE',  ( 2.493653234604083739E-15, 37.32890625216786873, 13.57481594606304576 ) ) ;
#249 = CARTESIAN_POINT ( 'NONE',  ( 143.1451861577818079, 36.93203125108394147, 5.444914386472293977 ) ) ;
#250 = CARTESIAN_POINT ( 'NONE',  ( 74.59884440882045453, 34.45156250216787441, -9.598844408820458085 ) ) ;
#251 = ORIENTED_EDGE ( 'NONE', *, *, #21153, .F. ) ;
#252 = VECTOR ( 'NONE', #26544, 1000.000000000000114 ) ;
#253 = CARTESIAN_POINT ( 'NONE',  ( 6.106658654948486920, 35.99999999999996447, 11.74215035806527396 ) ) ;
#254 = CARTESIAN_POINT ( 'NONE',  ( 2.493653234604083739E-15, 32.56640625216787299, 13.57481594606304576 ) ) ;
#255 = LINE ( 'NONE', #20201, #25320 ) ;
#256 = ADVANCED_FACE ( 'NONE', ( #12743 ), #3942, .F. ) ;
#257 = CARTESIAN_POINT ( 'NONE',  ( 104.9952793366501567, 116.8754121666685393, -48.57499999726882578 ) ) ;
#258 = CARTESIAN_POINT ( 'NONE',  ( 189.5550856135277229, 35.14609375108393152, 13.14518615778179722 ) ) ;
#259 = AXIS2_PLACEMENT_3D ( 'NONE', #9021, #6875, #19848 ) ;
#260 = AXIS2_PLACEMENT_3D ( 'NONE', #16112, #26536, #3014 ) ;
#261 = CARTESIAN_POINT ( 'NONE',  ( 1.662435489736055892E-15, 40.99999999999999289, 13.57481594606304576 ) ) ;
#263 = ORIENTED_EDGE ( 'NONE', *, *, #18368, .T. ) ;
#262 = CARTESIAN_POINT ( 'NONE',  ( 99.99999999999995737, 81.25000000000000000, 4.999999999999990230 ) ) ;
#264 = DIRECTION ( 'NONE',  ( 0.000000000000000000, -1.000000000000000000, 0.000000000000000000 ) ) ;
#265 = CARTESIAN_POINT ( 'NONE',  ( 95.67376207875072680, 104.0454443415356991, -48.19999999453764161 ) ) ;
#266 = CARTESIAN_POINT ( 'NONE',  ( -13.57481594606304576, 38.61874999999999147, 0.000000000000000000 ) ) ;
#267 = CARTESIAN_POINT ( 'NONE',  ( 139.5988444088204403, 38.32109374999999574, -9.598844408820458085 ) ) ;
#268 = CARTESIAN_POINT ( 'NONE',  ( 13.14518615778179900, 38.02343750108395426, -5.444914386472297529 ) ) ;
#269 = CARTESIAN_POINT ( 'NONE',  ( -13.14518615778179189, 36.63437500108393152, 5.444914386472304635 ) ) ;
#270 = CARTESIAN_POINT ( 'NONE',  ( 208.5748159460630120, 35.09648437499998863, -5.622872871577873077 ) ) ;
#271 = CARTESIAN_POINT ( 'NONE',  ( 204.1801758136480203, 55.00000000000014211, 9.999999999999948486 ) ) ;
#272 = CARTESIAN_POINT ( 'NONE',  ( 139.5988444088204403, 36.73359374999999716, -9.598844408820458085 ) ) ;
#273 = CARTESIAN_POINT ( 'NONE',  ( 74.29505027212704249, 35.49335937608393010, -9.295050272127046043 ) ) ;
#274 = CARTESIAN_POINT ( 'NONE',  ( 99.99999999999995737, -4.458734124999988779, 1.687500001365591418 ) ) ;
#275 = CARTESIAN_POINT ( 'NONE',  ( 102.4999999999999858, 123.0000000000000000, -8.724596124144689908E-15 ) ) ;
#276 = ORIENTED_EDGE ( 'NONE', *, *, #2418, .F. ) ;
#277 = ADVANCED_FACE ( 'NONE', ( #16895 ), #6077, .T. ) ;
#278 = DIRECTION ( 'NONE',  ( 0.000000000000000000, -1.000000000000000000, 0.000000000000000000 ) ) ;
#279 = CARTESIAN_POINT ( 'NONE',  ( 2.493653234604083739E-15, 35.64218749999999147, 13.57481594606304576 ) ) ;
#280 = CARTESIAN_POINT ( 'NONE',  ( 139.2950502721270425, 37.27929687608394005, -9.295050272127046043 ) ) ;
#281 = ORIENTED_EDGE ( 'NONE', *, *, #3794, .F. ) ;
#282 = ORIENTED_EDGE ( 'NONE', *, *, #1152, .F. ) ;
#283 = CARTESIAN_POINT ( 'NONE',  ( 104.9999999999999574, 83.56250000000002842, -2.071067811865491937 ) ) ;
#284 = CARTESIAN_POINT ( 'NONE',  ( 96.46446609406721961, 80.25000000273119838, 3.535533905932727539 ) ) ;
#285 = TOROIDAL_SURFACE ( 'NONE', #12557, 23.26794919243112858, 1.000000000000000000 ) ;
#286 = CARTESIAN_POINT ( 'NONE',  ( 98.15313185440925281, 92.99999999863439371, 4.458734124999979898 ) ) ;
#287 = CARTESIAN_POINT ( 'NONE',  ( 51.85082601884828080, 35.99999999999999289, -1.058935892997133088 ) ) ;
#288 = EDGE_CURVE ( 'NONE', #11725, #11898, #16264, .T. ) ;
#289 = CARTESIAN_POINT ( 'NONE',  ( 92.99999999999998579, 110.0000000000000000, -53.00000000000001421 ) ) ;
#290 = CARTESIAN_POINT ( 'NONE',  ( 59.37712712842213136, 40.85117187499999147, -13.57481594606304753 ) ) ;
#291 = VERTEX_POINT ( 'NONE', #25731 ) ;
#292 = CARTESIAN_POINT ( 'NONE',  ( 139.5988444088204403, 39.21406250216787015, -9.598844408820458085 ) ) ;
#293 = CARTESIAN_POINT ( 'NONE',  ( 101.8468681455906903, 4.458734125000016313, 3.375000001365592972 ) ) ;
#294 = EDGE_CURVE ( 'NONE', #22062, #7806, #16625, .T. ) ;
#295 = EDGE_LOOP ( 'NONE', ( #18742, #1157, #17267, #23427 ) ) ;
#296 = CARTESIAN_POINT ( 'NONE',  ( 120.8198241863519939, 50.00000000000000000, -9.999999999999998224 ) ) ;
#297 = CARTESIAN_POINT ( 'NONE',  ( -9.295050272127046043, 39.06523437608392868, -9.295050272127046043 ) ) ;
#298 = CARTESIAN_POINT ( 'NONE',  ( 181.4251840539369596, 33.90585937716787868, -5.622872871577873077 ) ) ;
#299 = AXIS2_PLACEMENT_3D ( 'NONE', #13990, #23131, #5887 ) ;
#300 = CARTESIAN_POINT ( 'NONE',  ( 13.14518615778179544, 37.77539062608393294, -1.609821015232357215E-15 ) ) ;
#301 = CARTESIAN_POINT ( 'NONE',  ( 92.99999999999998579, 110.0000000000000000, -145.0000000000000284 ) ) ;
#302 = CARTESIAN_POINT ( 'NONE',  ( 143.1451861577818363, 37.13046875108393863, 5.444914386472293977 ) ) ;
#303 = ORIENTED_EDGE ( 'NONE', *, *, #24870, .F. ) ;
#304 = CARTESIAN_POINT ( 'NONE',  ( 9.295050272127046043, 34.89804687608393863, -9.295050272127046043 ) ) ;
#305 = CARTESIAN_POINT ( 'NONE',  ( 124.5550856135277087, 35.14609375108393152, 13.14518615778179722 ) ) ;
#306 = CARTESIAN_POINT ( 'NONE',  ( 59.37712712842213136, 35.29492187500000000, -13.57481594606304753 ) ) ;
#307 = AXIS2_PLACEMENT_3D ( 'NONE', #10055, #1393, #9916 ) ;
#308 = CARTESIAN_POINT ( 'NONE',  ( 97.93301270000000613, 124.7500000010924737, -9.540979117872439019E-15 ) ) ;
#309 = CARTESIAN_POINT ( 'NONE',  ( 101.8468681455906903, -4.458734124999987891, 13.00000000136559386 ) ) ;
#310 = DIRECTION ( 'NONE',  ( -0.000000000000000000, 1.000000000000000000, -0.000000000000000000 ) ) ;
#311 = CARTESIAN_POINT ( 'NONE',  ( 95.54126587499995082, -1.846868145590724986, 0.5000000013655920839 ) ) ;
#312 = CARTESIAN_POINT ( 'NONE',  ( 102.4976396683250925, 102.3130555110000159, -44.52500000273119696 ) ) ;
#313 = CARTESIAN_POINT ( 'NONE',  ( 104.9999999999999716, 1.449011120738813565E-14, 5.625000002731185056 ) ) ;
#314 = FACE_OUTER_BOUND ( 'NONE', #8408, .T. ) ;
#315 = CARTESIAN_POINT ( 'NONE',  ( 106.5389055433250860, 105.2492070361643215, -50.82499999726882578 ) ) ;
#316 = CARTESIAN_POINT ( 'NONE',  ( 5.444914386472302859, 37.82500000108392868, 13.14518615778179189 ) ) ;
#317 = CARTESIAN_POINT ( 'NONE',  ( 108.0825317499999869, 107.3738262389971538, -54.97499999726881015 ) ) ;
#318 = ORIENTED_EDGE ( 'NONE', *, *, #24476, .T. ) ;
#319 = CARTESIAN_POINT ( 'NONE',  ( 98.53841926354351699, 124.6500000010924651, -1.461580736456474794 ) ) ;
#320 =( BOUNDED_CURVE ( )  B_SPLINE_CURVE ( 2, ( #29, #14971, #10973, #15395, #28107, #8572, #17262, #24107, #13244 ),
 .UNSPECIFIED., .F., .T. ) 
 B_SPLINE_CURVE_WITH_KNOTS ( ( 3, 2, 2, 2, 3 ),
 ( 0.1041666666666664909, 0.1145833333333332732, 0.1250000000000000833, 0.1354166666666668517, 0.1458333333333336757 ),
 .UNSPECIFIED. ) 
 CURVE ( )  GEOMETRIC_REPRESENTATION_ITEM ( )  RATIONAL_B_SPLINE_CURVE ( ( 1.000000000000001332, 0.9238795325112854062, 1.000000000000000000, 0.9238795325112867385, 1.000000000000000000, 0.9238795325112867385, 1.000000000000000000, 0.9238795325112842960, 1.000000000000002442 ) ) 
 REPRESENTATION_ITEM ( '' )  );
#321 = AXIS2_PLACEMENT_3D ( 'NONE', #9134, #9413, #17827 ) ;
#322 = CARTESIAN_POINT ( 'NONE',  ( 102.0669872999999797, 122.5500000010924850, -9.794112055954760458E-15 ) ) ;
#323 = FACE_OUTER_BOUND ( 'NONE', #26669, .T. ) ;
#324 = EDGE_CURVE ( 'NONE', #25689, #13199, #21050, .T. ) ;
#325 = CARTESIAN_POINT ( 'NONE',  ( 181.8548138422181921, 39.01562500108393294, 5.444914386472304635 ) ) ;
#326 = ORIENTED_EDGE ( 'NONE', *, *, #10011, .F. ) ;
#327 = CARTESIAN_POINT ( 'NONE',  ( 135.6228728715780107, 36.08867187716787583, -13.57481594606290898 ) ) ;
#328 = CARTESIAN_POINT ( 'NONE',  ( 104.4587341249999781, -1.846868145590721655, 13.12500000136559208 ) ) ;
#329 = ORIENTED_EDGE ( 'NONE', *, *, #20493, .F. ) ;
#330 = CARTESIAN_POINT ( 'NONE',  ( 95.00472066334982912, 116.8754121666685393, -51.67500000273118133 ) ) ;
#331 = CARTESIAN_POINT ( 'NONE',  ( 13.14518615778179900, 38.51953125108393294, 5.444914386472293977 ) ) ;
#332 = CARTESIAN_POINT ( 'NONE',  ( 101.4615807364564546, 122.8500000010924680, -1.461580736456474794 ) ) ;
#333 = CARTESIAN_POINT ( 'NONE',  ( 143.5748159460630404, 31.92148437716787512, 5.622872871577869525 ) ) ;
#334 = DIRECTION ( 'NONE',  ( -0.000000000000000000, 1.000000000000000000, -0.000000000000000000 ) ) ;
#335 = CARTESIAN_POINT ( 'NONE',  ( 96.46446609406726225, 92.24999999726880162, -3.535533905932738197 ) ) ;
#336 = AXIS2_PLACEMENT_3D ( 'NONE', #4217, #10471, #27744 ) ;
#337 = CARTESIAN_POINT ( 'NONE',  ( 74.29505027212704249, 37.87460937608393863, 9.295050272127046043 ) ) ;
#338 = CARTESIAN_POINT ( 'NONE',  ( 64.55395874322236693, 49.99999999978093257, -13.57776691409252656 ) ) ;
#339 = CARTESIAN_POINT ( 'NONE',  ( 189.3771271284221314, 40.35507812499998437, 13.57481594606304753 ) ) ;
#340 = CARTESIAN_POINT ( 'NONE',  ( 77.25119088044421289, 35.99999999999997158, 5.405483146088426061 ) ) ;
#341 = ORIENTED_EDGE ( 'NONE', *, *, #1476, .T. ) ;
#342 = EDGE_LOOP ( 'NONE', ( #1311, #13880, #16852, #27004 ) ) ;
#343 = CARTESIAN_POINT ( 'NONE',  ( 2.414731522848535132E-15, 40.15664062608393436, 13.14518615778179544 ) ) ;
#344 = CARTESIAN_POINT ( 'NONE',  ( 195.0000000000000000, 0.000000000000000000, 0.000000000000000000 ) ) ;
#345 = CARTESIAN_POINT ( 'NONE',  ( 98.15313185440923860, -4.458734124999987891, 12.87500000136559208 ) ) ;
#346 = CARTESIAN_POINT ( 'NONE',  ( 59.55508561352770158, 39.61093750108393152, -13.14518615778179722 ) ) ;
#347 = CARTESIAN_POINT ( 'NONE',  ( 103.1528011352953342, 82.81250000136560629, 3.152801135295355106 ) ) ;
#348 = CARTESIAN_POINT ( 'NONE',  ( 189.5550856135277229, 38.32109375108394289, 13.14518615778179722 ) ) ;
#349 = CARTESIAN_POINT ( 'NONE',  ( 9.295050272127046043, 37.27929687608394005, -9.295050272127046043 ) ) ;
#350 = CARTESIAN_POINT ( 'NONE',  ( 186.7886859848165102, 50.68678854790359622, 14.99999999999995737 ) ) ;
#351 = DIRECTION ( 'NONE',  ( 0.000000000000000000, 0.000000000000000000, -1.000000000000000000 ) ) ;
#352 = CARTESIAN_POINT ( 'NONE',  ( 208.1451861577818079, 40.40468750108393436, -5.444914386472297529 ) ) ;
#353 = CARTESIAN_POINT ( 'NONE',  ( 93.46109445667489979, 105.2492070361643215, -55.42499999726882720 ) ) ;
#354 = ORIENTED_EDGE ( 'NONE', *, *, #7968, .T. ) ;
#355 = CARTESIAN_POINT ( 'NONE',  ( 5.622872871577878406, 37.27929687499999289, 13.57481594606304576 ) ) ;
#356 = CARTESIAN_POINT ( 'NONE',  ( -5.444914386472299306, 38.32109375108394289, 13.14518615778179722 ) ) ;
#357 = ORIENTED_EDGE ( 'NONE', *, *, #27287, .T. ) ;
#358 = CARTESIAN_POINT ( 'NONE',  ( 116.8548138422182063, 34.35234375108393579, -5.444914386472297529 ) ) ;
#359 = AXIS2_PLACEMENT_3D ( 'NONE', #24146, #26286, #22010 ) ;
#360 = CARTESIAN_POINT ( 'NONE',  ( 74.29505027212704249, 34.69960937608393436, -9.295050272127046043 ) ) ;
#361 = CARTESIAN_POINT ( 'NONE',  ( 181.8548138422182205, 38.37070312608393152, 0.000000000000000000 ) ) ;
#362 = ORIENTED_EDGE ( 'NONE', *, *, #430, .T. ) ;
#363 = CARTESIAN_POINT ( 'NONE',  ( 99.99999999999995737, 80.00000000000000000, -1.387778780781445676E-14 ) ) ;
#364 = CARTESIAN_POINT ( 'NONE',  ( 5.444914386472302859, 32.07031250108393294, 13.14518615778179189 ) ) ;
#365 = CARTESIAN_POINT ( 'NONE',  ( 2.493653234604083739E-15, 35.64218749999999147, 13.57481594606304576 ) ) ;
#366 = CARTESIAN_POINT ( 'NONE',  ( 78.57481594606305464, 40.65273437499999432, -5.622872871577873966 ) ) ;
#367 = PLANE ( 'NONE',  #22670 ) ;
#368 = EDGE_CURVE ( 'NONE', #4636, #22369, #10615, .T. ) ;
#369 =( BOUNDED_CURVE ( )  B_SPLINE_CURVE ( 2, ( #25306, #14184, #6305, #9907, #1384, #3231, #14981, #3653, #12315 ),
 .UNSPECIFIED., .F., .F. ) 
 B_SPLINE_CURVE_WITH_KNOTS ( ( 3, 2, 2, 2, 3 ),
 ( 0.05000000000000004441, 0.07500000000000006661, 0.1000000000000000888, 0.1250000000000001110, 0.1500000000000001332 ),
 .UNSPECIFIED. ) 
 CURVE ( )  GEOMETRIC_REPRESENTATION_ITEM ( )  RATIONAL_B_SPLINE_CURVE ( ( 0.9999999999999998890, 0.9238795325112868495, 1.000000000000000000, 0.9238795325112867385, 1.000000000000000000, 0.9238795325112867385, 1.000000000000000000, 0.9238795325112862944, 1.000000000000000444 ) ) 
 REPRESENTATION_ITEM ( '' )  );
#370 = VERTEX_POINT ( 'NONE', #20912 ) ;
#371 = CARTESIAN_POINT ( 'NONE',  ( 0.000000000000000000, 40.99999999999999289, 0.000000000000000000 ) ) ;
#372 = CARTESIAN_POINT ( 'NONE',  ( 102.4999999999999858, 122.2813376356282191, 0.3865102666887284544 ) ) ;
#373 = CARTESIAN_POINT ( 'NONE',  ( 57.88450960814756030, 49.99999999945625717, 11.58166858714126235 ) ) ;
#374 = ORIENTED_EDGE ( 'NONE', *, *, #22029, .T. ) ;
#375 = CARTESIAN_POINT ( 'NONE',  ( 95.54126587499996504, 1.387778780781445676E-14, 7.437500001365592084 ) ) ;
#376 = ORIENTED_EDGE ( 'NONE', *, *, #19099, .T. ) ;
#377 = CARTESIAN_POINT ( 'NONE',  ( 99.99999999999998579, 122.9000000021849530, 2.499999999999978684 ) ) ;
#378 = CARTESIAN_POINT ( 'NONE',  ( 95.54126587499995082, 1.846868145590750077, 7.375000001365592084 ) ) ;
#379 = AXIS2_PLACEMENT_3D ( 'NONE', #4372, #22042, #19613 ) ;
#380 = CARTESIAN_POINT ( 'NONE',  ( -9.295050272127046043, 40.45429687608393721, -9.295050272127046043 ) ) ;
#381 = CARTESIAN_POINT ( 'NONE',  ( 84.99999999999998579, 99.99999999999998579, -45.00000000000000711 ) ) ;
#382 = CARTESIAN_POINT ( 'NONE',  ( 95.54126587499995082, 82.75000000136560629, 1.846868145590724986 ) ) ;
#383 = CARTESIAN_POINT ( 'NONE',  ( 65.00000000000000000, 36.18789062608393436, 13.14518615778179544 ) ) ;
#384 = CARTESIAN_POINT ( 'NONE',  ( 99.99999999999998579, 118.4984768113314004, -53.62500000273119127 ) ) ;
#385 = CARTESIAN_POINT ( 'NONE',  ( -13.14518615778179544, 36.58476562608393579, 0.000000000000000000 ) ) ;
#386 = PRODUCT_DEFINITION_FORMATION_WITH_SPECIFIED_SOURCE ( 'ANY', '', #2399, .NOT_KNOWN. ) ;
#387 = DIRECTION ( 'NONE',  ( 0.000000000000000000, 0.000000000000000000, -1.000000000000000000 ) ) ;
#388 = LINE ( 'NONE', #2390, #9039 ) ;
#389 = CARTESIAN_POINT ( 'NONE',  ( 95.67376207875072680, 115.9545556584642867, -54.79999999453764303 ) ) ;
#390 = CARTESIAN_POINT ( 'NONE',  ( 116.4251840539369454, 37.77539062499999289, -5.622872871577873077 ) ) ;
#391 = ORIENTED_EDGE ( 'NONE', *, *, #1518, .F. ) ;
#392 = ORIENTED_EDGE ( 'NONE', *, *, #14583, .T. ) ;
#393 = CARTESIAN_POINT ( 'NONE',  ( 106.9999999999999858, 112.2744378736303474, -51.90000000000001279 ) ) ;
#394 = CARTESIAN_POINT ( 'NONE',  ( 5.444914386472297529, 38.12265625108393152, -13.14518615778179900 ) ) ;
#395 = CARTESIAN_POINT ( 'NONE',  ( -9.598844408820454532, 37.22968750216787726, 9.598844408820459861 ) ) ;
#396 = CARTESIAN_POINT ( 'NONE',  ( 99.99999999999995737, -4.999999999999990230, 10.37500000273118594 ) ) ;
#397 = CARTESIAN_POINT ( 'NONE',  ( 124.5550856135277087, 37.52734375108393294, 13.14518615778179722 ) ) ;
#398 = CARTESIAN_POINT ( 'NONE',  ( 51.42518405393695957, 33.11210937716786873, -5.622872871577873077 ) ) ;
#399 = ORIENTED_EDGE ( 'NONE', *, *, #6701, .T. ) ;
#400 = CARTESIAN_POINT ( 'NONE',  ( 3.304118597822780057, 36.00000000000001421, 12.77244747738236441 ) ) ;
#401 = CARTESIAN_POINT ( 'NONE',  ( -13.57481594606304576, 33.95546875216787441, 0.000000000000000000 ) ) ;
#402 = CIRCLE ( 'NONE', #16324, 11.57481594606304398 ) ;
#403 = CARTESIAN_POINT ( 'NONE',  ( 102.4976396683250783, 117.6869444889999841, -46.47499999726882436 ) ) ;
#404 = AXIS2_PLACEMENT_3D ( 'NONE', #9924, #14615, #3535 ) ;
#405 = CARTESIAN_POINT ( 'NONE',  ( 181.8548138422182205, 34.99726562608393721, 0.000000000000000000 ) ) ;
#406 = FACE_OUTER_BOUND ( 'NONE', #21933, .T. ) ;
#407 = CARTESIAN_POINT ( 'NONE',  ( -8.312177448680279460E-16, 34.55078125216787299, -13.57481594606304576 ) ) ;
#408 = CARTESIAN_POINT ( 'NONE',  ( 189.3771271284220745, 40.05742187499998863, -13.57481594606297293 ) ) ;
#409 = CARTESIAN_POINT ( 'NONE',  ( -5.622872871578057818, 35.59257812499998863, 13.57481594606286457 ) ) ;
#410 = CARTESIAN_POINT ( 'NONE',  ( 120.8198241863519939, 55.00000000000000000, 14.99999999999996803 ) ) ;
#411 = CARTESIAN_POINT ( 'NONE',  ( -5.622872871577873077, 37.97382812499999716, 13.57481594606304753 ) ) ;
#412 = CARTESIAN_POINT ( 'NONE',  ( 135.6228728715778118, 38.07304687499999574, 13.57481594606313813 ) ) ;
#413 = CARTESIAN_POINT ( 'NONE',  ( -8.049105076161786076E-16, 36.58476562608393579, -13.14518615778179544 ) ) ;
#414 = CARTESIAN_POINT ( 'NONE',  ( -13.14518615778179189, 35.84062500108394289, 5.444914386472304635 ) ) ;
#415 = CARTESIAN_POINT ( 'NONE',  ( 181.4251840539369596, 33.11210937499999574, 5.622872871577880183 ) ) ;
#416 = CARTESIAN_POINT ( 'NONE',  ( 9.598844408820456309, 39.11484374999999858, -9.598844408820458085 ) ) ;
#417 = CARTESIAN_POINT ( 'NONE',  ( 70.44491438647230552, 36.83281250108392868, 13.14518615778179189 ) ) ;
#418 = CARTESIAN_POINT ( 'NONE',  ( 101.8468681455907046, -4.458734124999987891, 3.750000001365591640 ) ) ;
#419 = CARTESIAN_POINT ( 'NONE',  ( 100.8031273896213378, 123.0000000000000000, 2.371931796629188405 ) ) ;
#420 = CARTESIAN_POINT ( 'NONE',  ( 99.99999999999998579, 92.12499999726880162, -4.999999999999997335 ) ) ;
#421 = CARTESIAN_POINT ( 'NONE',  ( -9.598844408820454532, 34.74921874999999716, 9.598844408820459861 ) ) ;
#422 = CARTESIAN_POINT ( 'NONE',  ( 143.1451861577818079, 38.76757812608393294, -1.609821015232357215E-15 ) ) ;
#423 = ORIENTED_EDGE ( 'NONE', *, *, #17964, .T. ) ;
#424 = CARTESIAN_POINT ( 'NONE',  ( 102.0710678118654329, 82.68750000000001421, -5.000000000000018652 ) ) ;
#425 = CARTESIAN_POINT ( 'NONE',  ( 219.9999999999999716, 50.00000000000000000, -10.00000000000000000 ) ) ;
#426 = CARTESIAN_POINT ( 'NONE',  ( 103.5355339059327093, 83.50000000273119838, 3.535533905932726206 ) ) ;
#427 = CARTESIAN_POINT ( 'NONE',  ( 96.84719886470463734, 94.68749999863440792, -3.152801135295366208 ) ) ;
#428 = PRESENTATION_LAYER_ASSIGNMENT (  '', '', ( #26847 ) ) ;
#429 = CARTESIAN_POINT ( 'NONE',  ( 95.54126587499999346, 94.99999999863439371, -1.846868145590737864 ) ) ;
#430 = EDGE_CURVE ( 'NONE', #1457, #22555, #4820, .T. ) ;
#431 = CARTESIAN_POINT ( 'NONE',  ( 95.67376207875069838, 115.9545556584642867, -47.30000000000000426 ) ) ;
#432 = CARTESIAN_POINT ( 'NONE',  ( 59.37712712842213136, 39.56132812499999574, 13.57481594606304753 ) ) ;
#433 = ORIENTED_EDGE ( 'NONE', *, *, #23597, .T. ) ;
#434 = DIRECTION ( 'NONE',  ( 0.000000000000000000, 1.000000000000000000, -1.156482317317871478E-16 ) ) ;
#435 = CARTESIAN_POINT ( 'NONE',  ( 96.46446609406721961, 3.535533905932755072, 11.87500000000000000 ) ) ;
#436 = EDGE_LOOP ( 'NONE', ( #17651, #5409, #22660, #15371, #2602 ) ) ;
#437 = CARTESIAN_POINT ( 'NONE',  ( 5.444914386472297529, 35.74140625108393721, -13.14518615778179900 ) ) ;
#438 = CARTESIAN_POINT ( 'NONE',  ( 189.3771271284221314, 33.31054687716787299, 13.57481594606304753 ) ) ;
#439 = VERTEX_POINT ( 'NONE', #6346 ) ;
#440 = EDGE_CURVE ( 'NONE', #5976, #21288, #23550, .T. ) ;
#441 = CARTESIAN_POINT ( 'NONE',  ( 13.14518615778179544, 33.01289062608393010, -1.609821015232357215E-15 ) ) ;
#442 = CARTESIAN_POINT ( 'NONE',  ( 99.99999999999995737, 1.387778780781445676E-14, 34.79898987322334136 ) ) ;
#443 = CARTESIAN_POINT ( 'NONE',  ( 124.5550856135277087, 36.93203125108394147, 13.14518615778179722 ) ) ;
#444 = VERTEX_POINT ( 'NONE', #16759 ) ;
#445 = CARTESIAN_POINT ( 'NONE',  ( 13.14518615778179900, 33.95546875108393436, 5.444914386472293977 ) ) ;
#446 = EDGE_CURVE ( 'NONE', #27429, #27080, #21214, .T. ) ;
#447 = CARTESIAN_POINT ( 'NONE',  ( 120.7049497278729575, 32.51679687608393721, -9.295050272127046043 ) ) ;
#448 = CARTESIAN_POINT ( 'NONE',  ( 78.57481594606304043, 34.30273437500000000, -5.622872871577873077 ) ) ;
#449 = CARTESIAN_POINT ( 'NONE',  ( 97.93301269999999192, 124.7000000010924623, -0.8561741729129505041 ) ) ;
#450 = AXIS2_PLACEMENT_3D ( 'NONE', #25758, #24046, #13329 ) ;
#451 = EDGE_CURVE ( 'NONE', #10079, #19989, #7039, .T. ) ;
#452 = CARTESIAN_POINT ( 'NONE',  ( 103.1528011352953342, 3.152801135295383084, 11.31250000136559386 ) ) ;
#453 = FACE_OUTER_BOUND ( 'NONE', #21146, .T. ) ;
#454 = CARTESIAN_POINT ( 'NONE',  ( 96.84719886470459471, -3.152801135295355994, 0.5625000013655921949 ) ) ;
#455 = CARTESIAN_POINT ( 'NONE',  ( 99.99999999999998579, 118.4984768113314004, -45.62500000273118417 ) ) ;
#456 = CARTESIAN_POINT ( 'NONE',  ( 101.8468681455907046, -4.458734124999987891, 1.000000001365592528 ) ) ;
#457 = CARTESIAN_POINT ( 'NONE',  ( 102.0710678118654187, 83.81250000273119838, -5.000000000000015987 ) ) ;
#458 = CARTESIAN_POINT ( 'NONE',  ( 97.50236033167490746, 117.6869444889999841, -50.02499999726882152 ) ) ;
#459 = CARTESIAN_POINT ( 'NONE',  ( -5.444914386472299306, 36.13828125108393863, 13.14518615778179722 ) ) ;
#460 = ADVANCED_FACE ( 'NONE', ( #11167, #24165 ), #367, .F. ) ;
#461 = CARTESIAN_POINT ( 'NONE',  ( 92.99999999999998579, 110.0000000000000000, -48.49999999453763877 ) ) ;
#462 = ORIENTED_EDGE ( 'NONE', *, *, #14982, .F. ) ;
#463 = CARTESIAN_POINT ( 'NONE',  ( 101.4615807364564546, 124.4500000010924765, -1.461580736456474794 ) ) ;
#464 = CARTESIAN_POINT ( 'NONE',  ( 102.0669873000000081, 123.3000000010924850, 0.8561741729129311862 ) ) ;
#465 = DIRECTION ( 'NONE',  ( 0.000000000000000000, 0.000000000000000000, 1.000000000000000000 ) ) ;
#466 = CARTESIAN_POINT ( 'NONE',  ( 189.5550856135277229, 37.22968750108393721, -13.14518615778179900 ) ) ;
#467 = VERTEX_POINT ( 'NONE', #26304 ) ;
#468 = CARTESIAN_POINT ( 'NONE',  ( 13.57481594606304753, 39.95820312716787726, -5.622872871577873966 ) ) ;
#469 = CARTESIAN_POINT ( 'NONE',  ( 104.4587341249999781, -1.846868145590721655, 12.12500000136559208 ) ) ;
#470 = EDGE_CURVE ( 'NONE', #4431, #13527, #13159, .T. ) ;
#471 = VECTOR ( 'NONE', #27075, 1000.000000000000000 ) ;
#472 = ORIENTED_EDGE ( 'NONE', *, *, #2653, .T. ) ;
#473 = CARTESIAN_POINT ( 'NONE',  ( 107.0000000000000142, 110.0000000000000000, -47.00000000000000711 ) ) ;
#474 = CARTESIAN_POINT ( 'NONE',  ( -13.14518615778179189, 39.01562500108393294, 5.444914386472304635 ) ) ;
#475 = CARTESIAN_POINT ( 'NONE',  ( 101.0355339059327378, 123.1499999999999915, -2.499999999999997780 ) ) ;
#476 = EDGE_CURVE ( 'NONE', #26599, #20388, #21898, .T. ) ;
#477 = CARTESIAN_POINT ( 'NONE',  ( 143.5748159460630688, 32.76484375216787015, -1.662435489736055892E-15 ) ) ;
#478 = CARTESIAN_POINT ( 'NONE',  ( 9.295050272127047819, 39.46210937608393721, 9.295050272127046043 ) ) ;
#479 = EDGE_CURVE ( 'NONE', #25975, #2330, #24301, .T. ) ;
#480 = CARTESIAN_POINT ( 'NONE',  ( 104.9999999999999716, 94.81249999726880162, 2.071067811865467956 ) ) ;
#481 = CARTESIAN_POINT ( 'NONE',  ( 55.70494972787295751, 38.27148437608393294, -9.295050272127046043 ) ) ;
#482 = CARTESIAN_POINT ( 'NONE',  ( 62.97537227446170505, 50.00000000051003468, -13.43320860980927201 ) ) ;
#483 = CARTESIAN_POINT ( 'NONE',  ( 108.0825317500000153, 110.0000000000000000, -52.37500000273119838 ) ) ;
#484 = EDGE_CURVE ( 'NONE', #26503, #20101, #13985, .T. ) ;
#485 = CARTESIAN_POINT ( 'NONE',  ( 189.5550856135277229, 31.87187500108393223, -13.14518615778179900 ) ) ;
#486 = CARTESIAN_POINT ( 'NONE',  ( 102.4999999999999858, 123.1000000021849416, -9.847140817659276890E-15 ) ) ;
#487 = VERTEX_POINT ( 'NONE', #17746 ) ;
#488 = CARTESIAN_POINT ( 'NONE',  ( -9.295050272127046043, 35.09648437608393579, -9.295050272127046043 ) ) ;
#489 = CARTESIAN_POINT ( 'NONE',  ( 98.15313185440923860, -4.458734124999987891, 11.87500000136559208 ) ) ;
#490 =( BOUNDED_CURVE ( )  B_SPLINE_CURVE ( 2, ( #3629, #3902, #12290, #3485, #23428, #25141, #19000, #10438, #9887 ),
 .UNSPECIFIED., .F., .F. ) 
 B_SPLINE_CURVE_WITH_KNOTS ( ( 3, 2, 2, 2, 3 ),
 ( 0.4500000000000003997, 0.4750000000000003664, 0.5000000000000004441, 0.5250000000000004663, 0.5500000000000004885 ),
 .UNSPECIFIED. ) 
 CURVE ( )  GEOMETRIC_REPRESENTATION_ITEM ( )  RATIONAL_B_SPLINE_CURVE ( ( 0.9999999999999987788, 0.9238795325112879597, 1.000000000000000000, 0.9238795325112867385, 1.000000000000000000, 0.9238795325112867385, 1.000000000000000000, 0.9238795325112854062, 1.000000000000001332 ) ) 
 REPRESENTATION_ITEM ( '' )  );
#491 = CARTESIAN_POINT ( 'NONE',  ( 59.55508561352770158, 38.32109375108394289, 13.14518615778179722 ) ) ;
#492 = DIRECTION ( 'NONE',  ( -0.000000000000000000, 1.000000000000000000, -0.000000000000000000 ) ) ;
#493 = EDGE_LOOP ( 'NONE', ( #21611, #13258, #8930, #18827, #22732, #24894, #25682, #24306 ) ) ;
#494 = AXIS2_PLACEMENT_3D ( 'NONE', #24, #21266, #25957 ) ;
#495 = CARTESIAN_POINT ( 'NONE',  ( 13.14518615778179544, 36.38632812608393863, -1.609821015232357215E-15 ) ) ;
#496 = CARTESIAN_POINT ( 'NONE',  ( 97.50000000000000000, 124.9500000000000028, -1.035533905932742416 ) ) ;
#497 = CARTESIAN_POINT ( 'NONE',  ( 200.4449143864723055, 36.53515625108394715, -13.14518615778179722 ) ) ;
#498 = CARTESIAN_POINT ( 'NONE',  ( 91.91746824999998466, 110.0000000000000000, -53.62499999726882294 ) ) ;
#499 = VERTEX_POINT ( 'NONE', #223 ) ;
#500 = CARTESIAN_POINT ( 'NONE',  ( 2.493653234604083739E-15, 33.26093749999999716, 13.57481594606304576 ) ) ;
#501 = CARTESIAN_POINT ( 'NONE',  ( -8.049105076161786076E-16, 33.21132812608393436, -13.14518615778179544 ) ) ;
#502 = ORIENTED_EDGE ( 'NONE', *, *, #15207, .F. ) ;
#503 = CARTESIAN_POINT ( 'NONE',  ( 116.8548138422182063, 32.07031250108393294, 5.444914386472304635 ) ) ;
#504 = CARTESIAN_POINT ( 'NONE',  ( 51.85481384221820633, 35.04687500108393294, 5.444914386472304635 ) ) ;
#505 = CARTESIAN_POINT ( 'NONE',  ( 208.1451861577818079, 36.38632812608393863, -1.609821015232357215E-15 ) ) ;
#506 = VERTEX_POINT ( 'NONE', #11310 ) ;
#507 = CARTESIAN_POINT ( 'NONE',  ( 94.99999999999995737, 1.387778780781445676E-14, 34.79898987322334136 ) ) ;
#508 = CARTESIAN_POINT ( 'NONE',  ( -9.295050272127044266, 33.50898437608393010, 9.295050272127047819 ) ) ;
#509 = CARTESIAN_POINT ( 'NONE',  ( 99.99999999999995737, -4.999999999999990230, 1.375000002731184612 ) ) ;
#510 = AXIS2_PLACEMENT_3D ( 'NONE', #5908, #18592, #16158 ) ;
#511 = CARTESIAN_POINT ( 'NONE',  ( 124.3771271284221314, 39.36289062716787157, -13.57481594606304753 ) ) ;
#512 = CARTESIAN_POINT ( 'NONE',  ( 106.5389055433251002, 105.2492070361643215, -52.32500000273119412 ) ) ;
#513 = PLANE ( 'NONE',  #11990 ) ;
#514 = DIRECTION ( 'NONE',  ( -1.000000000000000000, 0.000000000000000000, 0.000000000000000000 ) ) ;
#515 = CARTESIAN_POINT ( 'NONE',  ( 208.1451861577817795, 39.61093750108393863, -5.444914386472297529 ) ) ;
#516 = VECTOR ( 'NONE', #15597, 1000.000000000000000 ) ;
#517 = CARTESIAN_POINT ( 'NONE',  ( 95.54126587499995082, -1.846868145590724986, 3.500000001365591196 ) ) ;
#518 = ORIENTED_EDGE ( 'NONE', *, *, #16489, .T. ) ;
#519 = CARTESIAN_POINT ( 'NONE',  ( 102.0669872999999797, 123.3500000010924680, -9.794112055954760458E-15 ) ) ;
#520 = CARTESIAN_POINT ( 'NONE',  ( 95.54126587499995082, 1.846868145590750077, 9.375000001365592084 ) ) ;
#521 = CARTESIAN_POINT ( 'NONE',  ( 139.1801758136480203, 50.00000000000000000, 9.999999999999953815 ) ) ;
#522 = CARTESIAN_POINT ( 'NONE',  ( 13.14518615778179544, 35.39414062608393152, -1.609821015232357215E-15 ) ) ;
#523 = CARTESIAN_POINT ( 'NONE',  ( 74.59884440882045453, 39.01562500216787299, 9.598844408820456309 ) ) ;
#524 = CARTESIAN_POINT ( 'NONE',  ( 93.00000000000000000, 110.0000000000000000, -52.50000000546237544 ) ) ;
#525 = CARTESIAN_POINT ( 'NONE',  ( 59.55508561352770158, 35.34453125108393579, 13.14518615778179722 ) ) ;
#526 = CARTESIAN_POINT ( 'NONE',  ( 108.0825317500000153, 110.0000000000000000, -46.12500000273119838 ) ) ;
#527 = CARTESIAN_POINT ( 'NONE',  ( 5.444914386472297529, 38.71796875108393721, -13.14518615778179722 ) ) ;
#528 = CARTESIAN_POINT ( 'NONE',  ( 104.9999999999999716, 1.449011120738813565E-14, 34.79898987322334136 ) ) ;
#529 = CARTESIAN_POINT ( 'NONE',  ( 6.085944215996224038, 54.65299103241510892, 14.99999999999999289 ) ) ;
#530 = CARTESIAN_POINT ( 'NONE',  ( 107.0000000000000000, 110.0000000000000000, -55.49999999453763877 ) ) ;
#531 = CARTESIAN_POINT ( 'NONE',  ( 139.5988444088204403, 37.52734375000000000, -9.598844408820458085 ) ) ;
#532 = ORIENTED_EDGE ( 'NONE', *, *, #5026, .F. ) ;
#533 = EDGE_LOOP ( 'NONE', ( #3888, #18754, #1481 ) ) ;
#534 = DIRECTION ( 'NONE',  ( 0.000000000000000000, -1.000000000000000000, 0.000000000000000000 ) ) ;
#535 = CARTESIAN_POINT ( 'NONE',  ( -5.444914386472297529, 35.84062500108394289, -13.14518615778179900 ) ) ;
#536 = CARTESIAN_POINT ( 'NONE',  ( -13.57481594606304576, 37.92421875216787441, 0.000000000000000000 ) ) ;
#537 = CARTESIAN_POINT ( 'NONE',  ( 97.92893218813451028, -4.999999999999989342, 8.312500002731185944 ) ) ;
#538 = CARTESIAN_POINT ( 'NONE',  ( 124.5550856135277087, 33.55859375108393294, 13.14518615778179722 ) ) ;
#539 = CARTESIAN_POINT ( 'NONE',  ( 51.42518405393695957, 34.69960937716787441, -5.622872871577873077 ) ) ;
#540 = VERTEX_POINT ( 'NONE', #15739 ) ;
#541 =( BOUNDED_CURVE ( )  B_SPLINE_CURVE ( 2, ( #6091, #14214, #10070, #8082, #18782 ),
 .UNSPECIFIED., .F., .F. ) 
 B_SPLINE_CURVE_WITH_KNOTS ( ( 3, 2, 3 ),
 ( 0.9500000000000009548, 0.9750000000000005329, 1.000000000000000000 ),
 .UNSPECIFIED. ) 
 CURVE ( )  GEOMETRIC_REPRESENTATION_ITEM ( )  RATIONAL_B_SPLINE_CURVE ( ( 0.9999999999999970024, 0.9238795325112897361, 1.000000000000000000, 0.9238795325112867385, 1.000000000000000000 ) ) 
 REPRESENTATION_ITEM ( '' )  );
#542 = CARTESIAN_POINT ( 'NONE',  ( 219.9999999999999716, 55.00000000000000000, 14.99999999999994316 ) ) ;
#543 = CARTESIAN_POINT ( 'NONE',  ( 13.57481594606304576, 32.76484375216787015, -1.662435489736055892E-15 ) ) ;
#544 = CARTESIAN_POINT ( 'NONE',  ( 102.4999999999999858, 123.9000000021849530, -9.847140817659276890E-15 ) ) ;
#545 = DIRECTION ( 'NONE',  ( 0.000000000000000000, 0.000000000000000000, 1.000000000000000000 ) ) ;
#546 = DIRECTION ( 'NONE',  ( 1.000000000000000000, 0.000000000000000000, -5.782411586589357392E-17 ) ) ;
#547 = CARTESIAN_POINT ( 'NONE',  ( 181.8548138422182205, 33.40976562608393863, 0.000000000000000000 ) ) ;
#548 = CARTESIAN_POINT ( 'NONE',  ( -9.598844408820454532, 31.67343750216787512, 9.598844408820459861 ) ) ;
#549 = CARTESIAN_POINT ( 'NONE',  ( 102.4999999999999716, 124.5569999999781601, 1.035533905932722876 ) ) ;
#550 = CARTESIAN_POINT ( 'NONE',  ( 97.93301270000000613, 124.5500000010924850, -9.540979117872439019E-15 ) ) ;
#551 = CARTESIAN_POINT ( 'NONE',  ( 95.00000000000000000, 94.43749999726878741, 2.071067811865463959 ) ) ;
#552 = CARTESIAN_POINT ( 'NONE',  ( 116.4251840539369596, 36.33671875216787583, 0.000000000000000000 ) ) ;
#553 = FACE_OUTER_BOUND ( 'NONE', #16139, .T. ) ;
#554 = CARTESIAN_POINT ( 'NONE',  ( 5.622872871577878406, 37.27929687499999289, 13.57481594606304576 ) ) ;
#555 = CARTESIAN_POINT ( 'NONE',  ( -2.086998648631069653, 36.00000000000000000, -13.31420566034952202 ) ) ;
#556 = CARTESIAN_POINT ( 'NONE',  ( -8.049105076161786076E-16, 33.40976562608393863, -13.14518615778179544 ) ) ;
#557 = CARTESIAN_POINT ( 'NONE',  ( -13.14518615778179900, 37.32890625108393579, -5.444914386472297529 ) ) ;
#558 = CARTESIAN_POINT ( 'NONE',  ( 181.4251840539369596, 33.90585937500000568, 5.622872871577880183 ) ) ;
#559 = CARTESIAN_POINT ( 'NONE',  ( 9.598844408820459861, 35.04687500216787299, 9.598844408820456309 ) ) ;
#560 = DIRECTION ( 'NONE',  ( 5.782411586589357392E-17, -0.000000000000000000, 1.000000000000000000 ) ) ;
#561 = CARTESIAN_POINT ( 'NONE',  ( 84.99999999999998579, 102.0000000000000000, -43.00000000000000000 ) ) ;
#562 = CARTESIAN_POINT ( 'NONE',  ( 55.70494972787295751, 35.89023437608393152, 9.295050272127047819 ) ) ;
#563 = CARTESIAN_POINT ( 'NONE',  ( 99.99999999999995737, 85.00000000000000000, -1.387778780781445676E-14 ) ) ;
#564 = DIRECTION ( 'NONE',  ( -0.000000000000000000, 1.000000000000000000, -0.000000000000000000 ) ) ;
#565 = ORIENTED_EDGE ( 'NONE', *, *, #12281, .F. ) ;
#566 = CARTESIAN_POINT ( 'NONE',  ( 98.35496906260777905, 122.9999999999999858, -1.258827244710729154 ) ) ;
#567 = CARTESIAN_POINT ( 'NONE',  ( -9.598844408820458085, 35.34453124999998863, -9.598844408820458085 ) ) ;
#568 = CARTESIAN_POINT ( 'NONE',  ( 143.1451861577818079, 38.81718750108393579, -5.444914386472297529 ) ) ;
#569 = ORIENTED_EDGE ( 'NONE', *, *, #14895, .T. ) ;
#570 = CARTESIAN_POINT ( 'NONE',  ( 102.0710678118654329, 81.68750000000000000, -5.000000000000018652 ) ) ;
#571 = EDGE_CURVE ( 'NONE', #4666, #18529, #26293, .T. ) ;
#572 = CARTESIAN_POINT ( 'NONE',  ( 101.4674565229751693, 123.0000000000000568, 1.992898914349557682 ) ) ;
#573 = CARTESIAN_POINT ( 'NONE',  ( 103.5355339059327093, 83.75000000273119838, -3.535533905932755072 ) ) ;
#574 = CARTESIAN_POINT ( 'NONE',  ( 99.99999999999998579, 93.25000000000000000, -4.999999999999997335 ) ) ;
#575 = CARTESIAN_POINT ( 'NONE',  ( 104.4587341249999923, 94.62499999863439371, -1.846868145590737198 ) ) ;
#576 = CARTESIAN_POINT ( 'NONE',  ( 95.67376207875069838, 104.0454443415356991, -50.70000000000000284 ) ) ;
#577 = CARTESIAN_POINT ( 'NONE',  ( 70.62287287157786864, 40.75195312500000711, -13.57481594606304753 ) ) ;
#578 = ORIENTED_EDGE ( 'NONE', *, *, #27721, .F. ) ;
#579 =( BOUNDED_SURFACE ( )  B_SPLINE_SURFACE ( 1, 2, ( 
 ( #14484, #7804, #25599, #1404, #3808, #3950, #3385, #8074, #3536, #18775, #16634, #25327, #10196, #25188, #14203, #7938, #27346, #18906, #19188, #18641, #12055, #16494, #27890, #10335, #5676, #23201, #25740, #23333, #27482, #12610, #10063, #23472, #8351, #5813, #14341, #23058, #6085, #12468, #12192, #16770, #12339, #3676, #20921, #27617, #1678, #5949, #25470, #21193, #14616, #9926, #19044, #20781, #1263, #27752, #8213, #16902, #1815, #10480, #17037, #6772, #21759, #11035, #19745, #26021, #26310, #229, #15029, #4507, #1950, #6629, #17754, #23747, #15458, #10757, #24172, #4649, #10620, #17327, #9059, #6223, #10898, #23610, #8915, #14890, #19469, #28029, #17604, #28168, #6492, #21903, #12882, #4087, #8636, #19325, #13164, #21612, #2377, #2088, #12751, #15168, #23887, #4365, #13308, #22035, #2511, #11172, #19606, #19891, #13022, #21474, #8495, #2236, #375, #17180, #4223, #91, #8772, #17461, #26163, #25886, #6355, #15314, #24029, #22176, #948, #26888, #2927, #15602, #3078, #6911, #2792, #20038, #11743, #11459, #18028, #13882, #4935, #24305, #20178, #11316, #24736, #13598, #5217, #22321, #1092, #662, #9335, #26742, #18324, #5359, #24880, #14025, #11597, #9619, #7184, #4791, #9759, #13738, #27031, #22750, #7046, #24598, #15882, #20319, #15744, #26457, #13449, #9475, #7477, #2655, #16172, #7334, #3216, #5077, #18177, #517, #9198, #17892, #11882, #22608, #22462, #20607, #807, #26600, #16023, #24449, #20469, #4163, #12025, #7904, #5778, #15100, #14967, #9896, #23686, #20749, #12688, #12958, #18607, #27442, #2165, #27965, #23026, #17258, #14305, #28103, #4300, #10031, #1233, #27312, #10692, #17111, #7769, #21413, #16599, #18743, #16456, #4022, #6290, #10556, #25151, #8421, #5641, #14170, #12160 ),
 ( #25815, #19398, #14447, #12823, #21549, #25291, #8567, #2023, #3496, #25958, #22888, #19266, #18469, #20886, #6431, #1370, #23822, #21692, #3353, #23545, #27176, #7628, #1892, #16320, #25021, #5502, #9133, #309, #2449, #6702, #167, #15823, #2593, #13095, #24529, #17969, #26243, #13385, #20116, #9273, #8849, #13240, #23964, #11397, #21836, #22257, #17687, #6845, #4872, #11254, #2732, #19973, #2312, #10969, #452, #21972, #4725, #26678, #11110, #4443, #594, #15390, #17826, #7126, #25, #22113, #17539, #24102, #19824, #8994, #26392, #19681, #10828, #4580, #15535, #24243, #5014, #15243, #19544, #26531, #6987, #15682, #24383, #13536, #13679, #22396, #8707, #17399, #26098, #6563, #14386, #7704, #12098, #5720, #9412, #16107, #16253, #7559, #18683, #20402, #5582, #25096, #7413, #22685, #2865, #1030, #24952, #15961, #3431, #20689, #18111, #1172, #24676, #887, #26825, #14247, #9701, #27386, #7271, #5438, #16398, #14106, #20548, #22969, #22829, #3296, #20825, #11966, #5154, #18402, #11535, #13959, #20251, #1302, #9971, #18544, #3155, #9837, #24811, #5295, #9558, #27248, #7845, #16540, #27108, #11825, #738, #25230, #13816, #22539, #3007, #11679, #18260, #26968, #27796, #7977, #23653, #12655, #10103, #21380, #16676, #12378, #18815, #6259, #21237, #10659, #1445, #8253, #27931, #6124, #12508, #14932, #14790, #23513, #4128, #3992, #27522, #1719, #25926, #5990, #3577, #8390, #1992, #10523, #23375, #1859, #8119, #27657, #1585, #19230, #16940, #17076, #10381, #25510, #23103, #25781, #19088, #12794, #25375, #21512, #25641, #5855, #19366, #28069, #14655, #18948, #21097, #8535, #17221, #14525, #6400, #12234, #10239, #20962, #23240, #3717, #16813, #3848, #16312, #15650, #26063, #26498, #21942, #11078, #9101 ) ),
 .UNSPECIFIED., .F., .F., .F. ) 
 B_SPLINE_SURFACE_WITH_KNOTS ( ( 2, 2 ),
 ( 3, 2, 2, 2, 2, 2, 2, 2, 2, 2, 2, 2, 2, 2, 2, 2, 2, 2, 2, 2, 2, 2, 2, 2, 2, 2, 2, 2, 2, 2, 2, 2, 2, 2, 2, 2, 2, 2, 2, 2, 2, 2, 2, 2, 2, 2, 2, 2, 2, 2, 2, 2, 2, 2, 2, 2, 2, 2, 2, 2, 2, 2, 2, 2, 2, 2, 2, 2, 2, 2, 2, 2, 2, 2, 2, 2, 2, 2, 2, 2, 2, 2, 2, 2, 2, 2, 2, 2, 2, 2, 2, 2, 2, 2, 2, 2, 2, 2, 2, 2, 2, 2, 2, 2, 2, 2, 2, 2, 2, 2, 2, 2, 3 ),
 ( 0.000000000000000000, 1.000000000000000000 ),
 ( 0.000000000000000000, 0.008928571428571428076, 0.01785714285714285615, 0.02678571428571428423, 0.03571428571428571230, 0.04464285714285714385, 0.05357142857142856845, 0.06250000000000000000, 0.07142857142857142461, 0.08035714285714286309, 0.08928571428571428770, 0.09821428571428571230, 0.1071428571428571369, 0.1160714285714285754, 0.1250000000000000000, 0.1339285714285714246, 0.1428571428571428492, 0.1517857142857142738, 0.1607142857142857262, 0.1696428571428571508, 0.1785714285714285754, 0.1875000000000000000, 0.1964285714285714246, 0.2053571428571428492, 0.2142857142857142738, 0.2232142857142857262, 0.2321428571428571508, 0.2410714285714285754, 0.2500000000000000000, 0.2589285714285714524, 0.2678571428571428492, 0.2767857142857143016, 0.2857142857142856984, 0.2946428571428571508, 0.3035714285714285476, 0.3125000000000000000, 0.3214285714285714524, 0.3303571428571428492, 0.3392857142857143016, 0.3482142857142856984, 0.3571428571428571508, 0.3660714285714285476, 0.3750000000000000000, 0.3839285714285714524, 0.3928571428571428492, 0.4017857142857143016, 0.4107142857142856984, 0.4196428571428571508, 0.4285714285714285476, 0.4375000000000000000, 0.4464285714285714524, 0.4553571428571428492, 0.4642857142857143016, 0.4732142857142856984, 0.4821428571428571508, 0.4910714285714285476, 0.5000000000000000000, 0.5089285714285713969, 0.5178571428571429047, 0.5267857142857143016, 0.5357142857142856984, 0.5446428571428570953, 0.5535714285714286031, 0.5625000000000000000, 0.5714285714285713969, 0.5803571428571429047, 0.5892857142857143016, 0.5982142857142856984, 0.6071428571428570953, 0.6160714285714286031, 0.6250000000000000000, 0.6339285714285713969, 0.6428571428571429047, 0.6517857142857143016, 0.6607142857142856984, 0.6696428571428570953, 0.6785714285714286031, 0.6875000000000000000, 0.6964285714285713969, 0.7053571428571429047, 0.7142857142857143016, 0.7232142857142856984, 0.7321428571428570953, 0.7410714285714286031, 0.7500000000000000000, 0.7589285714285713969, 0.7678571428571429047, 0.7767857142857143016, 0.7857142857142856984, 0.7946428571428570953, 0.8035714285714286031, 0.8125000000000000000, 0.8214285714285713969, 0.8303571428571429047, 0.8392857142857143016, 0.8482142857142856984, 0.8571428571428570953, 0.8660714285714286031, 0.8750000000000000000, 0.8839285714285713969, 0.8928571428571429047, 0.9017857142857143016, 0.9107142857142856984, 0.9196428571428570953, 0.9285714285714286031, 0.9375000000000000000, 0.9464285714285713969, 0.9553571428571429047, 0.9642857142857143016, 0.9732142857142856984, 0.9821428571428570953, 0.9910714285714286031, 1.000000000000000000 ),
 .UNSPECIFIED. ) 
 GEOMETRIC_REPRESENTATION_ITEM ( )  RATIONAL_B_SPLINE_SURFACE ( (
 ( 1.000000000000000000, 0.9238795325112867385, 1.000000000000000000, 0.9238795325112867385, 1.000000000000000000, 0.9238795325112867385, 1.000000000000000000, 0.9238795325112867385, 1.000000000000000000, 0.9238795325112867385, 1.000000000000000000, 0.9238795325112867385, 1.000000000000000000, 0.9238795325112867385, 1.000000000000000000, 0.9238795325112867385, 1.000000000000000000, 0.9238795325112867385, 1.000000000000000000, 0.9238795325112867385, 1.000000000000000000, 0.9238795325112867385, 1.000000000000000000, 0.9238795325112867385, 1.000000000000000000, 0.9238795325112867385, 1.000000000000000000, 0.9238795325112867385, 1.000000000000000000, 0.9238795325112867385, 1.000000000000000000, 0.9238795325112867385, 1.000000000000000000, 0.9238795325112867385, 1.000000000000000000, 0.9238795325112867385, 1.000000000000000000, 0.9238795325112867385, 1.000000000000000000, 0.9238795325112867385, 1.000000000000000000, 0.9238795325112867385, 1.000000000000000000, 0.9238795325112867385, 1.000000000000000000, 0.9238795325112867385, 1.000000000000000000, 0.9238795325112867385, 1.000000000000000000, 0.9238795325112867385, 1.000000000000000000, 0.9238795325112867385, 1.000000000000000000, 0.9238795325112867385, 1.000000000000000000, 0.9238795325112867385, 1.000000000000000000, 0.9238795325112867385, 1.000000000000000000, 0.9238795325112867385, 1.000000000000000000, 0.9238795325112867385, 1.000000000000000000, 0.9238795325112867385, 1.000000000000000000, 0.9238795325112867385, 1.000000000000000000, 0.9238795325112867385, 1.000000000000000000, 0.9238795325112867385, 1.000000000000000000, 0.9238795325112867385, 1.000000000000000000, 0.9238795325112867385, 1.000000000000000000, 0.9238795325112867385, 1.000000000000000000, 0.9238795325112867385, 1.000000000000000000, 0.9238795325112867385, 1.000000000000000000, 0.9238795325112867385, 1.000000000000000000, 0.9238795325112867385, 1.000000000000000000, 0.9238795325112867385, 1.000000000000000000, 0.9238795325112867385, 1.000000000000000000, 0.9238795325112867385, 1.000000000000000000, 0.9238795325112867385, 1.000000000000000000, 0.9238795325112867385, 1.000000000000000000, 0.9238795325112867385, 1.000000000000000000, 0.9238795325112867385, 1.000000000000000000, 0.9238795325112867385, 1.000000000000000000, 0.9238795325112867385, 1.000000000000000000, 0.9238795325112867385, 1.000000000000000000, 0.9238795325112867385, 1.000000000000000000, 0.9238795325112867385, 1.000000000000000000, 0.9238795325112867385, 1.000000000000000000, 0.9238795325112867385, 1.000000000000000000, 0.9238795325112867385, 1.000000000000000000, 0.9238795325112867385, 1.000000000000000000, 0.9238795325112867385, 1.000000000000000000, 0.9238795325112867385, 1.000000000000000000, 0.9238795325112867385, 1.000000000000000000, 0.9238795325112867385, 1.000000000000000000, 0.9238795325112867385, 1.000000000000000000, 0.9238795325112867385, 1.000000000000000000, 0.9238795325112867385, 1.000000000000000000, 0.9238795325112867385, 1.000000000000000000, 0.9238795325112867385, 1.000000000000000000, 0.9238795325112867385, 1.000000000000000000, 0.9238795325112867385, 1.000000000000000000, 0.9238795325112867385, 1.000000000000000000, 0.9238795325112867385, 1.000000000000000000, 0.9238795325112867385, 1.000000000000000000, 0.9238795325112867385, 1.000000000000000000, 0.9238795325112867385, 1.000000000000000000, 0.9238795325112867385, 1.000000000000000000, 0.9238795325112867385, 1.000000000000000000, 0.9238795325112867385, 1.000000000000000000, 0.9238795325112867385, 1.000000000000000000, 0.9238795325112867385, 1.000000000000000000, 0.9238795325112867385, 1.000000000000000000, 0.9238795325112867385, 1.000000000000000000, 0.9238795325112867385, 1.000000000000000000, 0.9238795325112867385, 1.000000000000000000, 0.9238795325112867385, 1.000000000000000000, 0.9238795325112867385, 1.000000000000000000, 0.9238795325112867385, 1.000000000000000000, 0.9238795325112867385, 1.000000000000000000, 0.9238795325112867385, 1.000000000000000000, 0.9238795325112867385, 1.000000000000000000, 0.9238795325112867385, 1.000000000000000000, 0.9238795325112867385, 1.000000000000000000, 0.9238795325112867385, 1.000000000000000000, 0.9238795325112867385, 1.000000000000000000, 0.9238795325112867385, 1.000000000000000000, 0.9238795325112867385, 1.000000000000000000, 0.9238795325112867385, 1.000000000000000000, 0.9238795325112867385, 1.000000000000000000, 0.9238795325112867385, 1.000000000000000000, 0.9238795325112867385, 1.000000000000000000, 0.9238795325112867385, 1.000000000000000000, 0.9238795325112867385, 1.000000000000000000, 0.9238795325112867385, 1.000000000000000000, 0.9238795325112867385, 1.000000000000000000, 0.9238795325112867385, 1.000000000000000000, 0.9238795325112867385, 1.000000000000000000, 0.9238795325112867385, 1.000000000000000000, 0.9238795325112867385, 1.000000000000000000, 0.9238795325112867385, 1.000000000000000000, 0.9238795325112867385, 1.000000000000000000, 0.9238795325112867385, 1.000000000000000000, 0.9238795325112867385, 1.000000000000000000, 0.9238795325112867385, 1.000000000000000000),
 ( 1.000000000000000000, 0.9238795325112867385, 1.000000000000000000, 0.9238795325112867385, 1.000000000000000000, 0.9238795325112867385, 1.000000000000000000, 0.9238795325112867385, 1.000000000000000000, 0.9238795325112867385, 1.000000000000000000, 0.9238795325112867385, 1.000000000000000000, 0.9238795325112867385, 1.000000000000000000, 0.9238795325112867385, 1.000000000000000000, 0.9238795325112867385, 1.000000000000000000, 0.9238795325112867385, 1.000000000000000000, 0.9238795325112867385, 1.000000000000000000, 0.9238795325112867385, 1.000000000000000000, 0.9238795325112867385, 1.000000000000000000, 0.9238795325112867385, 1.000000000000000000, 0.9238795325112867385, 1.000000000000000000, 0.9238795325112867385, 1.000000000000000000, 0.9238795325112867385, 1.000000000000000000, 0.9238795325112867385, 1.000000000000000000, 0.9238795325112867385, 1.000000000000000000, 0.9238795325112867385, 1.000000000000000000, 0.9238795325112867385, 1.000000000000000000, 0.9238795325112867385, 1.000000000000000000, 0.9238795325112867385, 1.000000000000000000, 0.9238795325112867385, 1.000000000000000000, 0.9238795325112867385, 1.000000000000000000, 0.9238795325112867385, 1.000000000000000000, 0.9238795325112867385, 1.000000000000000000, 0.9238795325112867385, 1.000000000000000000, 0.9238795325112867385, 1.000000000000000000, 0.9238795325112867385, 1.000000000000000000, 0.9238795325112867385, 1.000000000000000000, 0.9238795325112867385, 1.000000000000000000, 0.9238795325112867385, 1.000000000000000000, 0.9238795325112867385, 1.000000000000000000, 0.9238795325112867385, 1.000000000000000000, 0.9238795325112867385, 1.000000000000000000, 0.9238795325112867385, 1.000000000000000000, 0.9238795325112867385, 1.000000000000000000, 0.9238795325112867385, 1.000000000000000000, 0.9238795325112867385, 1.000000000000000000, 0.9238795325112867385, 1.000000000000000000, 0.9238795325112867385, 1.000000000000000000, 0.9238795325112867385, 1.000000000000000000, 0.9238795325112867385, 1.000000000000000000, 0.9238795325112867385, 1.000000000000000000, 0.9238795325112867385, 1.000000000000000000, 0.9238795325112867385, 1.000000000000000000, 0.9238795325112867385, 1.000000000000000000, 0.9238795325112867385, 1.000000000000000000, 0.9238795325112867385, 1.000000000000000000, 0.9238795325112867385, 1.000000000000000000, 0.9238795325112867385, 1.000000000000000000, 0.9238795325112867385, 1.000000000000000000, 0.9238795325112867385, 1.000000000000000000, 0.9238795325112867385, 1.000000000000000000, 0.9238795325112867385, 1.000000000000000000, 0.9238795325112867385, 1.000000000000000000, 0.9238795325112867385, 1.000000000000000000, 0.9238795325112867385, 1.000000000000000000, 0.9238795325112867385, 1.000000000000000000, 0.9238795325112867385, 1.000000000000000000, 0.9238795325112867385, 1.000000000000000000, 0.9238795325112867385, 1.000000000000000000, 0.9238795325112867385, 1.000000000000000000, 0.9238795325112867385, 1.000000000000000000, 0.9238795325112867385, 1.000000000000000000, 0.9238795325112867385, 1.000000000000000000, 0.9238795325112867385, 1.000000000000000000, 0.9238795325112867385, 1.000000000000000000, 0.9238795325112867385, 1.000000000000000000, 0.9238795325112867385, 1.000000000000000000, 0.9238795325112867385, 1.000000000000000000, 0.9238795325112867385, 1.000000000000000000, 0.9238795325112867385, 1.000000000000000000, 0.9238795325112867385, 1.000000000000000000, 0.9238795325112867385, 1.000000000000000000, 0.9238795325112867385, 1.000000000000000000, 0.9238795325112867385, 1.000000000000000000, 0.9238795325112867385, 1.000000000000000000, 0.9238795325112867385, 1.000000000000000000, 0.9238795325112867385, 1.000000000000000000, 0.9238795325112867385, 1.000000000000000000, 0.9238795325112867385, 1.000000000000000000, 0.9238795325112867385, 1.000000000000000000, 0.9238795325112867385, 1.000000000000000000, 0.9238795325112867385, 1.000000000000000000, 0.9238795325112867385, 1.000000000000000000, 0.9238795325112867385, 1.000000000000000000, 0.9238795325112867385, 1.000000000000000000, 0.9238795325112867385, 1.000000000000000000, 0.9238795325112867385, 1.000000000000000000, 0.9238795325112867385, 1.000000000000000000, 0.9238795325112867385, 1.000000000000000000, 0.9238795325112867385, 1.000000000000000000, 0.9238795325112867385, 1.000000000000000000, 0.9238795325112867385, 1.000000000000000000, 0.9238795325112867385, 1.000000000000000000, 0.9238795325112867385, 1.000000000000000000, 0.9238795325112867385, 1.000000000000000000, 0.9238795325112867385, 1.000000000000000000, 0.9238795325112867385, 1.000000000000000000, 0.9238795325112867385, 1.000000000000000000, 0.9238795325112867385, 1.000000000000000000, 0.9238795325112867385, 1.000000000000000000, 0.9238795325112867385, 1.000000000000000000, 0.9238795325112867385, 1.000000000000000000, 0.9238795325112867385, 1.000000000000000000, 0.9238795325112867385, 1.000000000000000000, 0.9238795325112867385, 1.000000000000000000, 0.9238795325112867385, 1.000000000000000000, 0.9238795325112867385, 1.000000000000000000, 0.9238795325112867385, 1.000000000000000000) ) ) 
 REPRESENTATION_ITEM ( '' )  SURFACE ( )  );
#580 = DIRECTION ( 'NONE',  ( 0.000000000000000000, 0.000000000000000000, -1.000000000000000000 ) ) ;
#581 = AXIS2_PLACEMENT_3D ( 'NONE', #23300, #18317, #25016 ) ;
#582 = CARTESIAN_POINT ( 'NONE',  ( 102.0710678118654329, -4.999999999999989342, 12.31249999999999822 ) ) ;
#583 = ORIENTED_EDGE ( 'NONE', *, *, #5538, .F. ) ;
#584 = CARTESIAN_POINT ( 'NONE',  ( -5.444914386472299306, 35.34453125108393579, 13.14518615778179722 ) ) ;
#585 = CARTESIAN_POINT ( 'NONE',  ( 185.4011555911795313, 33.06250000216787299, -9.598844408820458085 ) ) ;
#586 = CARTESIAN_POINT ( 'NONE',  ( -5.444914386472299306, 31.97109375108393792, 13.14518615778179722 ) ) ;
#587 = CARTESIAN_POINT ( 'NONE',  ( 200.6228728715780107, 36.08867187716787583, -13.57481594606290898 ) ) ;
#588 = LINE ( 'NONE', #8843, #28012 ) ;
#589 = CARTESIAN_POINT ( 'NONE',  ( 13.14518615778179900, 35.64218750108393152, -5.444914386472297529 ) ) ;
#590 = CARTESIAN_POINT ( 'NONE',  ( 116.8548138422182205, 31.82226562608393650, 0.000000000000000000 ) ) ;
#591 = CARTESIAN_POINT ( 'NONE',  ( 65.00000000000000000, 33.26093749999999716, 13.57481594606304576 ) ) ;
#592 = DIRECTION ( 'NONE',  ( -5.782411586589357392E-17, 0.000000000000000000, -1.000000000000000000 ) ) ;
#593 = CARTESIAN_POINT ( 'NONE',  ( 122.9316343120017194, 36.00000000000003553, 11.09140360074130705 ) ) ;
#594 = CARTESIAN_POINT ( 'NONE',  ( 99.99999999999995737, -4.458734124999988779, 10.93750000136559208 ) ) ;
#595 = CARTESIAN_POINT ( 'NONE',  ( 207.0772764098356049, 36.00000000000000000, -6.197985357349214297 ) ) ;
#596 = CARTESIAN_POINT ( 'NONE',  ( 98.15313185440923860, 4.458734125000016313, 14.25000000136559208 ) ) ;
#597 = CARTESIAN_POINT ( 'NONE',  ( 91.91746824999998466, 107.3738262389971538, -45.02500000273118985 ) ) ;
#598 = CARTESIAN_POINT ( 'NONE',  ( 98.15313185440925281, 91.24999999863439371, 4.458734124999979898 ) ) ;
#599 = FACE_OUTER_BOUND ( 'NONE', #17431, .T. ) ;
#600 = CARTESIAN_POINT ( 'NONE',  ( 95.00472066334981491, 103.1245878333314465, -51.32499999726881157 ) ) ;
#601 = CARTESIAN_POINT ( 'NONE',  ( 5.444914386472297529, 37.32890625108393579, -13.14518615778179900 ) ) ;
#602 = VECTOR ( 'NONE', #8159, 1000.000000000000000 ) ;
#603 = ORIENTED_EDGE ( 'NONE', *, *, #9339, .T. ) ;
#604 = CYLINDRICAL_SURFACE ( 'NONE', #14088, 10.50000000000001599 ) ;
#606 = EDGE_CURVE ( 'NONE', #15224, #13309, #67, .T. ) ;
#605 = CARTESIAN_POINT ( 'NONE',  ( 104.4587341249999781, 90.56249999863440792, -6.938893903907228378E-15 ) ) ;
#607 = CARTESIAN_POINT ( 'NONE',  ( 99.99999999999998579, 123.7000000021849502, 2.499999999999978684 ) ) ;
#608 = EDGE_CURVE ( 'NONE', #15564, #13869, #4643, .T. ) ;
#609 = CARTESIAN_POINT ( 'NONE',  ( 208.1451861577818079, 35.39414062608393152, -1.609821015232357215E-15 ) ) ;
#610 = ORIENTED_EDGE ( 'NONE', *, *, #1683, .F. ) ;
#611 = CARTESIAN_POINT ( 'NONE',  ( 203.4023157812191300, 54.99999999485618929, -14.99999999999999645 ) ) ;
#612 = CARTESIAN_POINT ( 'NONE',  ( 101.8468681455906903, -4.458734124999987891, 9.000000001365593860 ) ) ;
#613 = VERTEX_POINT ( 'NONE', #17102 ) ;
#614 = CARTESIAN_POINT ( 'NONE',  ( 102.1631189606246295, 116.6573956140660897, -46.60000000000000142 ) ) ;
#615 = CARTESIAN_POINT ( 'NONE',  ( 13.14518615778179900, 36.23750000108393010, -5.444914386472297529 ) ) ;
#616 = CARTESIAN_POINT ( 'NONE',  ( 98.23223304703363112, 124.1000000000000085, -1.767766952966370209 ) ) ;
#617 = AXIS2_PLACEMENT_3D ( 'NONE', #8449, #19290, #20876 ) ;
#618 = EDGE_CURVE ( 'NONE', #28009, #5791, #13088, .T. ) ;
#619 = CARTESIAN_POINT ( 'NONE',  ( 120.7049497278729575, 38.86679687608393863, -9.295050272127046043 ) ) ;
#620 = LINE ( 'NONE', #26269, #12057 ) ;
#621 = CARTESIAN_POINT ( 'NONE',  ( 5.444914386472297529, 35.54296875108393294, -13.14518615778179900 ) ) ;
#622 =( BOUNDED_CURVE ( )  B_SPLINE_CURVE ( 2, ( #23987, #4050, #21858, #21436, #25840, #8308, #4465, #8730, #16998 ),
 .UNSPECIFIED., .F., .T. ) 
 B_SPLINE_CURVE_WITH_KNOTS ( ( 3, 2, 2, 2, 3 ),
 ( 0.3500000000000003109, 0.3750000000000003331, 0.4000000000000003553, 0.4250000000000003775, 0.4500000000000003997 ),
 .UNSPECIFIED. ) 
 CURVE ( )  GEOMETRIC_REPRESENTATION_ITEM ( )  RATIONAL_B_SPLINE_CURVE ( ( 0.9999999999999990008, 0.9238795325112877377, 1.000000000000000000, 0.9238795325112867385, 1.000000000000000000, 0.9238795325112867385, 1.000000000000000000, 0.9238795325112855172, 1.000000000000001110 ) ) 
 REPRESENTATION_ITEM ( '' )  );
#623 = CARTESIAN_POINT ( 'NONE',  ( 97.92893218813452449, 95.56249999726883004, 4.999999999999983125 ) ) ;
#624 = CARTESIAN_POINT ( 'NONE',  ( 78.14518615778179367, 38.02343750108395426, -5.444914386472297529 ) ) ;
#625 = CARTESIAN_POINT ( 'NONE',  ( 55.81982418635199394, 49.99999999999999289, -14.99999999999999822 ) ) ;
#626 = CARTESIAN_POINT ( 'NONE',  ( 104.9952793366501709, 103.1245878333314465, -50.67500000273119554 ) ) ;
#627 = CARTESIAN_POINT ( 'NONE',  ( 181.8548138422182205, 32.81445312608393294, 0.000000000000000000 ) ) ;
#628 = DIRECTION ( 'NONE',  ( 0.000000000000000000, -1.000000000000000000, 0.000000000000000000 ) ) ;
#629 = CARTESIAN_POINT ( 'NONE',  ( 13.14518615778179900, 36.33671875108394289, 5.444914386472293977 ) ) ;
#630 = CARTESIAN_POINT ( 'NONE',  ( 99.99999999999995737, -4.458734124999988779, 7.937500001365592084 ) ) ;
#631 = CARTESIAN_POINT ( 'NONE',  ( 59.55508561352770158, 38.02343750108394005, -13.14518615778179722 ) ) ;
#632 = ADVANCED_FACE ( 'NONE', ( #6014 ), #27956, .F. ) ;
#633 = CARTESIAN_POINT ( 'NONE',  ( 65.00000000000000000, 38.81718749999999574, 13.57481594606304576 ) ) ;
#634 = CARTESIAN_POINT ( 'NONE',  ( 208.1451861577818079, 36.18789062608393436, -1.609821015232357215E-15 ) ) ;
#635 = EDGE_LOOP ( 'NONE', ( #198, #4757, #6902, #2298 ) ) ;
#636 = CARTESIAN_POINT ( 'NONE',  ( -13.14518615778179189, 39.21406250108392300, 5.444914386472304635 ) ) ;
#637 = VERTEX_POINT ( 'NONE', #2015 ) ;
#638 = CARTESIAN_POINT ( 'NONE',  ( 99.99999999999998579, 91.31249999863440792, 4.458734124999981674 ) ) ;
#639 = CARTESIAN_POINT ( 'NONE',  ( 181.8548138422182205, 38.32109375108394289, -5.444914386472297529 ) ) ;
#640 = CARTESIAN_POINT ( 'NONE',  ( 102.4976396683250783, 117.6869444889999841, -50.47499999726882436 ) ) ;
#641 = ORIENTED_EDGE ( 'NONE', *, *, #1027, .F. ) ;
#642 = VECTOR ( 'NONE', #23365, 1000.000000000000000 ) ;
#643 = CARTESIAN_POINT ( 'NONE',  ( 5.622872871577878406, 33.31054687499999289, 13.57481594606304576 ) ) ;
#644 = CARTESIAN_POINT ( 'NONE',  ( 5.444914386472297529, 33.16171875108393152, -13.14518615778179900 ) ) ;
#645 = ORIENTED_EDGE ( 'NONE', *, *, #3764, .T. ) ;
#646 = CARTESIAN_POINT ( 'NONE',  ( 130.0000000000000000, 33.80664062608393294, 13.14518615778179544 ) ) ;
#647 = CARTESIAN_POINT ( 'NONE',  ( 70.44491438647230552, 32.07031250108393294, 13.14518615778179189 ) ) ;
#648 = EDGE_CURVE ( 'NONE', #24292, #15569, #2303, .T. ) ;
#649 = CARTESIAN_POINT ( 'NONE',  ( 195.0000000000000000, 33.80664062608393294, 13.14518615778179544 ) ) ;
#650 = ORIENTED_EDGE ( 'NONE', *, *, #4627, .F. ) ;
#651 = CARTESIAN_POINT ( 'NONE',  ( 96.46446609406721961, 3.535533905932755072, 11.00000000273118594 ) ) ;
#652 = CARTESIAN_POINT ( 'NONE',  ( -0.3969994146497772824, 51.45716825712459297, -15.00000000000033573 ) ) ;
#653 = CARTESIAN_POINT ( 'NONE',  ( 99.99999999999995737, -4.999999999999990230, 5.375000002731185056 ) ) ;
#654 = CARTESIAN_POINT ( 'NONE',  ( 65.00000000000000000, 36.00000000000000000, -7.517135062566165128E-15 ) ) ;
#655 = CARTESIAN_POINT ( 'NONE',  ( 104.9952793366501709, 103.1245878333314465, -46.42500000273119554 ) ) ;
#656 =( BOUNDED_CURVE ( )  B_SPLINE_CURVE ( 2, ( #15903, #27198, #9360, #11907, #14190, #4961, #20631, #9782, #7650 ),
 .UNSPECIFIED., .F., .T. ) 
 B_SPLINE_CURVE_WITH_KNOTS ( ( 3, 2, 2, 2, 3 ),
 ( 0.2708333333333330928, 0.2812499999999998890, 0.2916666666666666852, 0.3020833333333334259, 0.3125000000000002220 ),
 .UNSPECIFIED. ) 
 CURVE ( )  GEOMETRIC_REPRESENTATION_ITEM ( )  RATIONAL_B_SPLINE_CURVE ( ( 1.000000000000001554, 0.9238795325112850731, 1.000000000000000000, 0.9238795325112867385, 1.000000000000000000, 0.9238795325112867385, 1.000000000000000000, 0.9238795325112850731, 1.000000000000001554 ) ) 
 REPRESENTATION_ITEM ( '' )  );
#657 = FACE_OUTER_BOUND ( 'NONE', #19869, .T. ) ;
#658 = CARTESIAN_POINT ( 'NONE',  ( -9.598844408820454532, 34.05468750216788010, 9.598844408820459861 ) ) ;
#659 = CARTESIAN_POINT ( 'NONE',  ( 208.1451861577818079, 40.35507812608393863, -1.609821015232357215E-15 ) ) ;
#660 = ORIENTED_EDGE ( 'NONE', *, *, #2653, .F. ) ;
#661 =( NAMED_UNIT ( * ) SI_UNIT ( $, .STERADIAN. ) SOLID_ANGLE_UNIT ( ) );
#662 = CARTESIAN_POINT ( 'NONE',  ( 95.54126587499995082, 1.846868145590750077, 5.375000001365592972 ) ) ;
#663 = EDGE_LOOP ( 'NONE', ( #12558, #2041, #9546, #25011 ) ) ;
#664 = CARTESIAN_POINT ( 'NONE',  ( -5.622872871577920151, 35.39414062716787868, -13.57481594606300135 ) ) ;
#665 = CARTESIAN_POINT ( 'NONE',  ( 95.54126587499995082, 1.846868145590750077, 6.375000001365592084 ) ) ;
#666 = CARTESIAN_POINT ( 'NONE',  ( 138.3959387413077593, 54.99999999495823744, 14.99999999999996092 ) ) ;
#667 = CARTESIAN_POINT ( 'NONE',  ( -5.444914386472297529, 37.22968750108393721, -13.14518615778179900 ) ) ;
#668 = CYLINDRICAL_SURFACE ( 'NONE', #16059, 5.000000000000004441 ) ;
#669 = CARTESIAN_POINT ( 'NONE',  ( 78.14518615778179367, 33.21132812608393436, -1.609821015232357215E-15 ) ) ;
#670 = CARTESIAN_POINT ( 'NONE',  ( 96.84719886470463734, 92.68749999863440792, -3.152801135295366208 ) ) ;
#671 = CARTESIAN_POINT ( 'NONE',  ( 108.0825317500000153, 110.0000000000000000, -48.12500000273119838 ) ) ;
#672 = CARTESIAN_POINT ( 'NONE',  ( -8.049105076161786076E-16, 37.97382812608393721, -13.14518615778179544 ) ) ;
#673 = CIRCLE ( 'NONE', #4302, 5.000000000000000888 ) ;
#674 = CARTESIAN_POINT ( 'NONE',  ( 97.83688103937535629, 116.6573956140660897, -52.89999999453764445 ) ) ;
#675 = CARTESIAN_POINT ( 'NONE',  ( -3.863925265120440322, 54.10645156200380512, 14.99999999999999645 ) ) ;
#676 = CARTESIAN_POINT ( 'NONE',  ( 135.6228728715778971, 40.45429687500001137, 13.57481594606306174 ) ) ;
#677 = CARTESIAN_POINT ( 'NONE',  ( 143.5748159460630688, 37.42812499999999432, -1.662435489736055892E-15 ) ) ;
#678 = ORIENTED_EDGE ( 'NONE', *, *, #24104, .F. ) ;
#679 = CARTESIAN_POINT ( 'NONE',  ( 104.3262379212492448, 115.9545556584642867, -51.70000000000001705 ) ) ;
#680 = CARTESIAN_POINT ( 'NONE',  ( 13.14518615778179900, 33.95546875108393436, 5.444914386472293977 ) ) ;
#681 = CARTESIAN_POINT ( 'NONE',  ( -13.57481594606304576, 33.95546875216787441, 0.000000000000000000 ) ) ;
#682 = CARTESIAN_POINT ( 'NONE',  ( 104.9999999999999716, 1.449011120738813565E-14, 9.625000002731184168 ) ) ;
#683 = CARTESIAN_POINT ( 'NONE',  ( 116.8548138422182063, 31.87187500108393223, 5.444914386472304635 ) ) ;
#684 = CARTESIAN_POINT ( 'NONE',  ( 59.55508561352770158, 38.81718750108393579, -13.14518615778179900 ) ) ;
#685 = CYLINDRICAL_SURFACE ( 'NONE', #17971, 7.000000000000006217 ) ;
#686 = CARTESIAN_POINT ( 'NONE',  ( -9.598844408820458085, 32.26875000216787726, -9.598844408820458085 ) ) ;
#687 = CARTESIAN_POINT ( 'NONE',  ( 99.99999999999995737, 5.000000000000018652, 2.749999999999999112 ) ) ;
#688 = CARTESIAN_POINT ( 'NONE',  ( 99.99999999999997158, 101.5015231886685712, -53.37499999726883004 ) ) ;
#689 = AXIS2_PLACEMENT_3D ( 'NONE', #15191, #26185, #8519 ) ;
#690 = CARTESIAN_POINT ( 'NONE',  ( -8.312177448680279460E-16, 37.72578125216787726, -13.57481594606304576 ) ) ;
#691 = CARTESIAN_POINT ( 'NONE',  ( 195.0000000000000000, 35.19570312608392726, 13.14518615778179544 ) ) ;
#692 = DIRECTION ( 'NONE',  ( 0.000000000000000000, -1.000000000000000000, 0.000000000000000000 ) ) ;
#693 = CARTESIAN_POINT ( 'NONE',  ( 98.96446609406727646, 124.3569999999781430, 2.499999999999977796 ) ) ;
#694 = CARTESIAN_POINT ( 'NONE',  ( 99.99999999999998579, 123.9500000010924765, 2.066987299999980099 ) ) ;
#695 = CARTESIAN_POINT ( 'NONE',  ( 0.000000000000000000, 40.99999999999999289, -13.57481594606304576 ) ) ;
#696 = CARTESIAN_POINT ( 'NONE',  ( -9.598844408820458085, 35.34453124999998863, -9.598844408820458085 ) ) ;
#697 = DIRECTION ( 'NONE',  ( 0.000000000000000000, 0.000000000000000000, -1.000000000000000000 ) ) ;
#698 = CARTESIAN_POINT ( 'NONE',  ( 5.622872871577878406, 34.10429687499999574, 13.57481594606304576 ) ) ;
#699 = CARTESIAN_POINT ( 'NONE',  ( 94.33688103937534208, 114.1144967660473242, -45.20000000000000995 ) ) ;
#700 = CARTESIAN_POINT ( 'NONE',  ( -13.14518615778179900, 33.55859375108393294, -5.444914386472297529 ) ) ;
#701 = CARTESIAN_POINT ( 'NONE',  ( 13.14518615778179900, 34.65000000108393152, -5.444914386472297529 ) ) ;
#702 = CARTESIAN_POINT ( 'NONE',  ( -9.295050272127044266, 35.09648437608392868, 9.295050272127047819 ) ) ;
#703 = CARTESIAN_POINT ( 'NONE',  ( -5.622872871577873077, 34.89804687716787868, 13.57481594606304753 ) ) ;
#704 = DIRECTION ( 'NONE',  ( 0.000000000000000000, 0.000000000000000000, 1.000000000000000000 ) ) ;
#705 = CARTESIAN_POINT ( 'NONE',  ( 70.44491438647230552, 32.86406250108392868, 13.14518615778179189 ) ) ;
#706 = CARTESIAN_POINT ( 'NONE',  ( 106.5389055433251002, 105.2492070361643215, -52.57500000273119412 ) ) ;
#707 = CARTESIAN_POINT ( 'NONE',  ( 99.99999999999998579, 123.7000000021849502, 2.499999999999978684 ) ) ;
#708 = CARTESIAN_POINT ( 'NONE',  ( 195.0000000000000000, 36.93203125216787441, -13.57481594606304576 ) ) ;
#709 = CARTESIAN_POINT ( 'NONE',  ( 13.57481594606304753, 32.71523437500000142, -5.622872871577873077 ) ) ;
#710 = CARTESIAN_POINT ( 'NONE',  ( 116.8548138422182063, 36.73359375108393010, -5.444914386472297529 ) ) ;
#711 = ORIENTED_EDGE ( 'NONE', *, *, #4617, .T. ) ;
#712 = CARTESIAN_POINT ( 'NONE',  ( 97.92893218813451028, 80.18750000000000000, 4.999999999999989342 ) ) ;
#713 = CIRCLE ( 'NONE', #17080, 5.000000000000004441 ) ;
#714 = CARTESIAN_POINT ( 'NONE',  ( 97.83688103937535629, 116.6573956140660897, -47.40000000000001279 ) ) ;
#715 = CARTESIAN_POINT ( 'NONE',  ( 104.4587341249999781, 84.00000000136560629, -1.846868145590750299 ) ) ;
#716 = CARTESIAN_POINT ( 'NONE',  ( 96.46446609406726225, 91.62500000000000000, 3.535533905932723986 ) ) ;
#717 = CARTESIAN_POINT ( 'NONE',  ( -8.312177448680279460E-16, 34.45156249999999432, -13.57481594606304576 ) ) ;
#718 = CARTESIAN_POINT ( 'NONE',  ( 91.91746824999997045, 112.6261737610028320, -45.72499999726882436 ) ) ;
#719 = CARTESIAN_POINT ( 'NONE',  ( 55.70494972787295751, 32.11992187608393579, 9.295050272127047819 ) ) ;
#720 = AXIS2_PLACEMENT_3D ( 'NONE', #7150, #15417, #19999 ) ;
#721 = VECTOR ( 'NONE', #26504, 1000.000000000000000 ) ;
#722 = ORIENTED_EDGE ( 'NONE', *, *, #13713, .T. ) ;
#723 = CARTESIAN_POINT ( 'NONE',  ( 96.46446609406726225, 95.24999999726881583, -3.535533905932738197 ) ) ;
#724 = B_SPLINE_CURVE_WITH_KNOTS ( 'NONE', 3,
 ( #27392, #24818, #7851, #20969 ),
 .UNSPECIFIED., .F., .F.,
 ( 4, 4 ),
 ( 0.000000000000000000, 1.000000000000000000 ),
 .UNSPECIFIED. ) ;
#725 = CARTESIAN_POINT ( 'NONE',  ( 104.9999999999999716, 1.449011120738813565E-14, 11.50000000000000000 ) ) ;
#726 = EDGE_LOOP ( 'NONE', ( #26515, #6676, #7045, #6065, #18961, #16121, #12170, #2779, #21665, #14808, #18012, #26164 ) ) ;
#727 = CARTESIAN_POINT ( 'NONE',  ( 13.14518615778179900, 36.43593750108392726, -5.444914386472297529 ) ) ;
#728 = CARTESIAN_POINT ( 'NONE',  ( 189.3771271284221314, 35.69179687716786731, 13.57481594606304753 ) ) ;
#729 = CARTESIAN_POINT ( 'NONE',  ( -5.444914386472297529, 32.46718750108393436, -13.14518615778179722 ) ) ;
#730 = LINE ( 'NONE', #20110, #16690 ) ;
#731 = CARTESIAN_POINT ( 'NONE',  ( 116.8548138422182205, 40.55351562608393579, 0.000000000000000000 ) ) ;
#732 = CARTESIAN_POINT ( 'NONE',  ( 5.444914386472297529, 36.53515625108393294, -13.14518615778179900 ) ) ;
#733 = EDGE_CURVE ( 'NONE', #12114, #10399, #2983, .T. ) ;
#734 = CARTESIAN_POINT ( 'NONE',  ( 107.0000000000000142, 110.0000000000000000, -49.50000000546238255 ) ) ;
#735 = CARTESIAN_POINT ( 'NONE',  ( 101.8468681455907330, 91.49999999863440792, -4.458734124999994997 ) ) ;
#736 = DIRECTION ( 'NONE',  ( 0.000000000000000000, 0.000000000000000000, 1.000000000000000000 ) ) ;
#737 = CARTESIAN_POINT ( 'NONE',  ( 117.6241215996508060, 35.99999999999999289, 4.513979326318619201 ) ) ;
#738 = CARTESIAN_POINT ( 'NONE',  ( 96.84719886470459471, 3.152801135295383084, 5.562500001365592972 ) ) ;
#739 = CARTESIAN_POINT ( 'NONE',  ( 208.0198548647683197, 36.00000000000000711, 3.369129432478914055 ) ) ;
#740 = CARTESIAN_POINT ( 'NONE',  ( 96.84719886470459471, 3.152801135295383084, 11.31250000136559208 ) ) ;
#741 = CARTESIAN_POINT ( 'NONE',  ( 93.00000000000000000, 110.0000000000000000, -52.50000000546237544 ) ) ;
#742 = CARTESIAN_POINT ( 'NONE',  ( 0.000000000000000000, 50.00000000000000000, 0.000000000000000000 ) ) ;
#743 = AXIS2_PLACEMENT_3D ( 'NONE', #5650, #23447, #6063 ) ;
#744 = DIRECTION ( 'NONE',  ( -5.782411586589357392E-17, -0.000000000000000000, -1.000000000000000000 ) ) ;
#745 = CYLINDRICAL_SURFACE ( 'NONE', #13433, 11.57481594606304398 ) ;
#746 = CARTESIAN_POINT ( 'NONE',  ( -9.295050272127044266, 34.50117187608393721, 9.295050272127047819 ) ) ;
#747 = VERTEX_POINT ( 'NONE', #25950 ) ;
#748 = PRESENTATION_STYLE_ASSIGNMENT (( #20411 ) ) ;
#749 =( BOUNDED_CURVE ( )  B_SPLINE_CURVE ( 2, ( #24281, #4762, #20290, #13422, #20439 ),
 .UNSPECIFIED., .F., .F. ) 
 B_SPLINE_CURVE_WITH_KNOTS ( ( 3, 2, 3 ),
 ( 0.000000000000000000, 0.02500000000000002220, 0.05000000000000004441 ),
 .UNSPECIFIED. ) 
 CURVE ( )  GEOMETRIC_REPRESENTATION_ITEM ( )  RATIONAL_B_SPLINE_CURVE ( ( 1.000000000000000000, 0.9238795325112867385, 1.000000000000000000, 0.9238795325112866275, 1.000000000000000222 ) ) 
 REPRESENTATION_ITEM ( '' )  );
#750 = DIRECTION ( 'NONE',  ( -1.000000000000000000, 0.000000000000000000, 0.000000000000000000 ) ) ;
#751 = CARTESIAN_POINT ( 'NONE',  ( 97.50000000000000000, 123.4500000021849502, -1.035533905932742416 ) ) ;
#752 = CARTESIAN_POINT ( 'NONE',  ( 208.1451861577817795, 35.34453125108392868, 5.444914386472293977 ) ) ;
#753 = ORIENTED_EDGE ( 'NONE', *, *, #18439, .F. ) ;
#754 = CARTESIAN_POINT ( 'NONE',  ( 193.4989808756949685, 53.60014735326986113, -15.00000000000000000 ) ) ;
#755 = CARTESIAN_POINT ( 'NONE',  ( 101.8468681455906903, -4.458734124999987891, 10.00000000136559386 ) ) ;
#756 = VERTEX_POINT ( 'NONE', #28095 ) ;
#757 = CARTESIAN_POINT ( 'NONE',  ( 93.46109445667491400, 105.2492070361643215, -51.17500000273119554 ) ) ;
#758 = CARTESIAN_POINT ( 'NONE',  ( -13.14518615778179189, 35.04687500108393294, 5.444914386472304635 ) ) ;
#759 = AXIS2_PLACEMENT_3D ( 'NONE', #7749, #5760, #14289 ) ;
#760 = CARTESIAN_POINT ( 'NONE',  ( 101.0355339059327378, 123.6500000000000199, 2.499999999999977796 ) ) ;
#761 = CARTESIAN_POINT ( 'NONE',  ( 99.99999999999998579, 94.75000000000000000, 4.999999999999984013 ) ) ;
#762 = CARTESIAN_POINT ( 'NONE',  ( 120.7049497278729575, 37.27929687608393294, -9.295050272127046043 ) ) ;
#763 = CARTESIAN_POINT ( 'NONE',  ( -5.444914386472299306, 37.72578125108394431, 13.14518615778179722 ) ) ;
#764 = CARTESIAN_POINT ( 'NONE',  ( -9.295050272127044266, 34.30273437608393294, 9.295050272127047819 ) ) ;
#765 = CARTESIAN_POINT ( 'NONE',  ( 95.54126587499999346, 93.99999999863439371, -1.846868145590737864 ) ) ;
#766 = CARTESIAN_POINT ( 'NONE',  ( 57.37803646580599093, 54.91641323977226818, -14.99999999999999822 ) ) ;
#767 = CARTESIAN_POINT ( 'NONE',  ( 91.91746824999998466, 112.6261737610028320, -53.47500000273119980 ) ) ;
#768 = CARTESIAN_POINT ( 'NONE',  ( 208.5748159460630120, 39.85898437499999858, -5.622872871577873077 ) ) ;
#769 = EDGE_CURVE ( 'NONE', #10253, #21981, #23538, .T. ) ;
#770 = CARTESIAN_POINT ( 'NONE',  ( 69.85997726958113674, 35.99999999999999289, 12.29462155906316134 ) ) ;
#771 = ORIENTED_EDGE ( 'NONE', *, *, #15560, .F. ) ;
#772 = CARTESIAN_POINT ( 'NONE',  ( -5.444914386472297529, 36.63437500108393152, -13.14518615778179900 ) ) ;
#773 = CARTESIAN_POINT ( 'NONE',  ( 101.8468681455907046, 4.458734125000016313, 6.375000001365592084 ) ) ;
#774 = AXIS2_PLACEMENT_3D ( 'NONE', #17038, #5950, #27753 ) ;
#775 = CARTESIAN_POINT ( 'NONE',  ( 65.00000000000000000, 38.76757812608393294, -13.14518615778179544 ) ) ;
#776 = CARTESIAN_POINT ( 'NONE',  ( 99.99999999999998579, 124.7999999999999972, -2.499999999999997780 ) ) ;
#777 = CARTESIAN_POINT ( 'NONE',  ( 94.99999999999994316, -2.071067811865454633, 14.06249999999999645 ) ) ;
#778 = VERTEX_POINT ( 'NONE', #4290 ) ;
#779 = CARTESIAN_POINT ( 'NONE',  ( -8.049105076161786076E-16, 34.99726562608393721, -13.14518615778179544 ) ) ;
#780 = EDGE_LOOP ( 'NONE', ( #22014, #25520, #18027, #26838 ) ) ;
#781 = AXIS2_PLACEMENT_3D ( 'NONE', #19737, #5175, #18568 ) ;
#782 = CARTESIAN_POINT ( 'NONE',  ( 100.8561741729129295, 123.2000000010924765, 2.066987299999979211 ) ) ;
#783 = CARTESIAN_POINT ( 'NONE',  ( 95.54126587500000767, 92.06249999863440792, -7.484931351350258973E-15 ) ) ;
#784 = CARTESIAN_POINT ( 'NONE',  ( 204.2950502721270425, 37.08085937608393579, 9.295050272127046043 ) ) ;
#785 = CARTESIAN_POINT ( 'NONE',  ( 97.50236033167490746, 102.3130555110000159, -51.47499999726882436 ) ) ;
#786 = EDGE_LOOP ( 'NONE', ( #13335, #26038, #5279, #4137, #3777, #6140, #22751, #12521, #6165, #4758, #19712, #15028, #12709, #11189, #23225, #569, #24661 ) ) ;
#787 = CARTESIAN_POINT ( 'NONE',  ( -8.312177448680279460E-16, 32.86406249999999574, -13.57481594606304576 ) ) ;
#788 = CARTESIAN_POINT ( 'NONE',  ( 9.295050272127047819, 35.29492187608393294, 9.295050272127046043 ) ) ;
#789 = VERTEX_POINT ( 'NONE', #17249 ) ;
#790 = CARTESIAN_POINT ( 'NONE',  ( 135.4449143864723055, 32.26875000108393721, 13.14518615778179189 ) ) ;
#791 = CARTESIAN_POINT ( 'NONE',  ( 55.70494972787295751, 40.65273437608393436, -9.295050272127046043 ) ) ;
#792 = CARTESIAN_POINT ( 'NONE',  ( 189.5550856135277229, 34.25312500108393010, -13.14518615778179900 ) ) ;
#793 = ADVANCED_FACE ( 'NONE', ( #6282, #1743 ), #6424, .F. ) ;
#794 =( BOUNDED_CURVE ( )  B_SPLINE_CURVE ( 2, ( #5981, #8244, #25772, #1851, #19221, #27923, #21502, #17214, #25918 ),
 .UNSPECIFIED., .F., .T. ) 
 B_SPLINE_CURVE_WITH_KNOTS ( ( 3, 2, 2, 2, 3 ),
 ( 0.5249747582430949189, 0.5312500000000001110, 0.5416666666666668517, 0.5520833333333337034, 0.5625000000000004441 ),
 .UNSPECIFIED. ) 
 CURVE ( )  GEOMETRIC_REPRESENTATION_ITEM ( )  RATIONAL_B_SPLINE_CURVE ( ( 0.9635368518655842429, 0.9541432637305302666, 1.000000000000000000, 0.9238795325112867385, 1.000000000000000000, 0.9238795325112867385, 1.000000000000000000, 0.9238795325112835188, 1.000000000000003331 ) ) 
 REPRESENTATION_ITEM ( '' )  );
#795 = ORIENTED_EDGE ( 'NONE', *, *, #15778, .F. ) ;
#796 = CARTESIAN_POINT ( 'NONE',  ( 99.99999999999998579, 91.62499999726880162, 4.999999999999984013 ) ) ;
#797 = CARTESIAN_POINT ( 'NONE',  ( 7.171391216998964424, 31.99955315621561525, -11.52591757658528948 ) ) ;
#798 = AXIS2_PLACEMENT_3D ( 'NONE', #21029, #12723, #5784 ) ;
#799 = CARTESIAN_POINT ( 'NONE',  ( 143.5748159460630404, 39.06523437716786873, 5.622872871577869525 ) ) ;
#800 = CARTESIAN_POINT ( 'NONE',  ( 93.46109445667491400, 114.7507929638356785, -45.32500000273119412 ) ) ;
#801 = CARTESIAN_POINT ( 'NONE',  ( -18.00000000000000711, 80.00000000000000000, -12.99999999999999645 ) ) ;
#802 = EDGE_CURVE ( 'NONE', #24847, #3863, #10819, .T. ) ;
#803 = FACE_OUTER_BOUND ( 'NONE', #4700, .T. ) ;
#804 = FACE_OUTER_BOUND ( 'NONE', #18856, .T. ) ;
#805 = ORIENTED_EDGE ( 'NONE', *, *, #10321, .T. ) ;
#806 = SURFACE_STYLE_USAGE ( .BOTH. , #11458 ) ;
#807 = CARTESIAN_POINT ( 'NONE',  ( 103.1528011352953342, 3.152801135295383084, 3.062500001365592528 ) ) ;
#808 = EDGE_LOOP ( 'NONE', ( #10115, #14859, #2478, #8132 ) ) ;
#809 = CARTESIAN_POINT ( 'NONE',  ( -13.15267690958718205, 36.00000000000000711, 0.5874252385153145850 ) ) ;
#810 = CARTESIAN_POINT ( 'NONE',  ( 104.4587341249999781, 1.846868145590750299, 10.00000000136559208 ) ) ;
#811 = CARTESIAN_POINT ( 'NONE',  ( 138.2014461876379983, 50.69246985422729779, 14.99999999999717382 ) ) ;
#812 = ADVANCED_FACE ( 'NONE', ( #14959 ), #15093, .T. ) ;
#813 = CARTESIAN_POINT ( 'NONE',  ( 2.414731522848535132E-15, 35.98945312608393010, 13.14518615778179544 ) ) ;
#814 = CARTESIAN_POINT ( 'NONE',  ( 185.4011555911795313, 40.20625000216787726, -9.598844408820458085 ) ) ;
#815 = CARTESIAN_POINT ( 'NONE',  ( 70.44491438647230552, 32.56640625108394005, -13.14518615778179900 ) ) ;
#816 = CARTESIAN_POINT ( 'NONE',  ( 99.99999999999998579, 118.4984768113314004, -47.62500000273119127 ) ) ;
#817 = CARTESIAN_POINT ( 'NONE',  ( -5.622872871577947684, 39.36289062716787157, -13.57481594606297293 ) ) ;
#818 = AXIS2_PLACEMENT_3D ( 'NONE', #8800, #11063, #545 ) ;
#819 = CARTESIAN_POINT ( 'NONE',  ( 55.81982418635200816, 50.00000000000000000, -10.00000000000000000 ) ) ;
#820 = CARTESIAN_POINT ( 'NONE',  ( -4.925026783666235808, 49.99999999893053371, 12.67776588291678408 ) ) ;
#821 = CARTESIAN_POINT ( 'NONE',  ( 102.0710678118654613, 91.06249999726880162, -4.999999999999997335 ) ) ;
#822 = CARTESIAN_POINT ( 'NONE',  ( 143.5748159460630688, 35.84062499999999574, -1.662435489736055892E-15 ) ) ;
#823 = ORIENTED_EDGE ( 'NONE', *, *, #16054, .F. ) ;
#824 = ADVANCED_FACE ( 'NONE', ( #21683 ), #14677, .F. ) ;
#825 = ORIENTED_EDGE ( 'NONE', *, *, #22272, .F. ) ;
#826 = DIRECTION ( 'NONE',  ( -1.156482317317871478E-16, 0.000000000000000000, -1.000000000000000000 ) ) ;
#827 = CARTESIAN_POINT ( 'NONE',  ( -5.444914386472297529, 32.66562500108393863, -13.14518615778179900 ) ) ;
#828 = CARTESIAN_POINT ( 'NONE',  ( 13.57481594606304753, 35.19570312716788152, -5.622872871577873077 ) ) ;
#829 = CARTESIAN_POINT ( 'NONE',  ( 97.92893218813451028, -4.999999999999989342, 9.312500002731184168 ) ) ;
#830 = CARTESIAN_POINT ( 'NONE',  ( 116.8548138422182063, 34.25312500108393010, 5.444914386472304635 ) ) ;
#831 = PRODUCT_DEFINITION_SHAPE ( 'NONE', 'NONE',  #10642 ) ;
#832 = CARTESIAN_POINT ( 'NONE',  ( 78.14518615778179367, 38.56914062608393579, -1.609821015232357215E-15 ) ) ;
#833 = CARTESIAN_POINT ( 'NONE',  ( 2.414731522848535132E-15, 39.16445312608392726, 13.14518615778179544 ) ) ;
#834 = CARTESIAN_POINT ( 'NONE',  ( -14.99999999999999822, 55.00000000000000000, 15.00000000000000000 ) ) ;
#835 = CARTESIAN_POINT ( 'NONE',  ( 102.0710678118654329, 5.000000000000018652, 1.687499999999999778 ) ) ;
#836 = CARTESIAN_POINT ( 'NONE',  ( 108.0825317499999869, 107.3738262389971680, -54.97499999726881015 ) ) ;
#837 = CARTESIAN_POINT ( 'NONE',  ( -13.57481594606304576, 38.76757812716787299, 5.622872871577880183 ) ) ;
#838 = CARTESIAN_POINT ( 'NONE',  ( 0.000000000000000000, 36.00000000000000000, 0.000000000000000000 ) ) ;
#839 = DIRECTION ( 'NONE',  ( -0.000000000000000000, -1.000000000000000000, -0.000000000000000000 ) ) ;
#840 = CARTESIAN_POINT ( 'NONE',  ( 99.99999999999997158, 102.6397644303321215, -52.50000000000000711 ) ) ;
#841 = CARTESIAN_POINT ( 'NONE',  ( 98.53841926354351699, 123.6500000010924794, -1.461580736456474794 ) ) ;
#842 = CARTESIAN_POINT ( 'NONE',  ( 122.6059679576636796, 35.99999999999999289, -11.20317769887070547 ) ) ;
#843 = DIRECTION ( 'NONE',  ( 0.000000000000000000, 0.000000000000000000, 1.000000000000000000 ) ) ;
#844 = CARTESIAN_POINT ( 'NONE',  ( 94.99999999999995737, 1.387778780781445676E-14, 34.79898987322334136 ) ) ;
#845 = CARTESIAN_POINT ( 'NONE',  ( -9.598844408820458085, 33.75703124999999005, -9.598844408820458085 ) ) ;
#846 = CARTESIAN_POINT ( 'NONE',  ( -5.622872871577828668, 33.21132812499999432, 13.57481594606309194 ) ) ;
#847 = CARTESIAN_POINT ( 'NONE',  ( 2.414731522848535132E-15, 35.39414062608393863, 13.14518615778179544 ) ) ;
#848 = CARTESIAN_POINT ( 'NONE',  ( 13.14518615778179544, 32.21914062608393436, -1.609821015232357215E-15 ) ) ;
#849 = CARTESIAN_POINT ( 'NONE',  ( -13.14518615778179189, 34.25312500108393721, 5.444914386472304635 ) ) ;
#850 = EDGE_CURVE ( 'NONE', #21579, #8168, #25534, .T. ) ;
#851 = CARTESIAN_POINT ( 'NONE',  ( 13.57481594606304576, 35.14609375216787157, -1.662435489736055892E-15 ) ) ;
#852 = CARTESIAN_POINT ( 'NONE',  ( -8.312177448680279460E-16, 37.72578125216787726, -13.57481594606304576 ) ) ;
#853 = CARTESIAN_POINT ( 'NONE',  ( 96.84719886470459471, 83.56250000136560629, 3.152801135295355994 ) ) ;
#854 = CARTESIAN_POINT ( 'NONE',  ( 74.29505027212704249, 33.11210937608393579, -9.295050272127046043 ) ) ;
#855 = DIRECTION ( 'NONE',  ( 1.000000000000000000, 0.000000000000000000, -5.782411586589357392E-17 ) ) ;
#856 = CARTESIAN_POINT ( 'NONE',  ( 102.1049798866730214, 123.0000000000000284, -1.357224074530030800 ) ) ;
#857 = EDGE_LOOP ( 'NONE', ( #26118, #7258, #9956, #20270 ) ) ;
#858 = CARTESIAN_POINT ( 'NONE',  ( 102.0669872999999797, 124.1500000010924794, -9.794112055954760458E-15 ) ) ;
#859 = CARTESIAN_POINT ( 'NONE',  ( -8.312177448680279460E-16, 38.51953125216787299, -13.57481594606304576 ) ) ;
#860 = CARTESIAN_POINT ( 'NONE',  ( 143.1451861577818079, 35.59257812608393579, -1.609821015232357215E-15 ) ) ;
#861 = VERTEX_POINT ( 'NONE', #19534 ) ;
#862 = DIRECTION ( 'NONE',  ( -0.000000000000000000, -1.000000000000000000, -0.000000000000000000 ) ) ;
#863 = CARTESIAN_POINT ( 'NONE',  ( 92.99999999999998579, 110.0000000000000000, -54.49999999453763877 ) ) ;
#864 = CARTESIAN_POINT ( 'NONE',  ( 99.99999999999995737, 82.68750000136560629, 4.458734124999988779 ) ) ;
#865 = CARTESIAN_POINT ( 'NONE',  ( 99.99999999999998579, 92.75000000000000000, 4.999999999999984013 ) ) ;
#866 = CARTESIAN_POINT ( 'NONE',  ( 70.62287287157788285, 38.96601562716787015, 13.57481594606304576 ) ) ;
#867 = VECTOR ( 'NONE', #8438, 1000.000000000000000 ) ;
#868 = CARTESIAN_POINT ( 'NONE',  ( 97.50236033167490746, 117.6869444889999841, -50.02499999726882152 ) ) ;
#869 = CARTESIAN_POINT ( 'NONE',  ( 65.00000000000000000, 33.01289062608393721, 13.14518615778179544 ) ) ;
#870 = AXIS2_PLACEMENT_3D ( 'NONE', #1170, #3005, #6740 ) ;
#871 = CARTESIAN_POINT ( 'NONE',  ( -13.57481594606304576, 37.97382812716787726, 5.622872871577880183 ) ) ;
#872 = ORIENTED_EDGE ( 'NONE', *, *, #6518, .F. ) ;
#873 = CARTESIAN_POINT ( 'NONE',  ( 192.9130013513680808, 36.00000000000000711, -13.31420566034936392 ) ) ;
#874 = CARTESIAN_POINT ( 'NONE',  ( 103.5355339059327093, -3.535533905932726206, 13.37500000000000000 ) ) ;
#875 = EDGE_LOOP ( 'NONE', ( #22304, #6186, #9476, #20532 ) ) ;
#876 = CARTESIAN_POINT ( 'NONE',  ( -5.444914386472299306, 36.93203125108394147, 13.14518615778179722 ) ) ;
#877 = CARTESIAN_POINT ( 'NONE',  ( 200.6228728715778686, 32.11992187716787583, -13.57481594606304753 ) ) ;
#878 = CARTESIAN_POINT ( 'NONE',  ( -5.444914386472297529, 33.26093750108393721, -13.14518615778179722 ) ) ;
#879 = DIRECTION ( 'NONE',  ( 0.000000000000000000, 0.000000000000000000, 1.000000000000000000 ) ) ;
#880 = CARTESIAN_POINT ( 'NONE',  ( 135.4449143864723339, 40.30546875108393579, -13.14518615778179722 ) ) ;
#881 = CARTESIAN_POINT ( 'NONE',  ( 13.14518615778179544, 35.59257812608393579, -1.609821015232357215E-15 ) ) ;
#882 = CARTESIAN_POINT ( 'NONE',  ( 93.00000000000000000, 110.0000000000000000, -50.50000000546237544 ) ) ;
#883 = CARTESIAN_POINT ( 'NONE',  ( 51.42518405393695957, 32.31835937499999289, 5.622872871577880183 ) ) ;
#884 = DIRECTION ( 'NONE',  ( 0.000000000000000000, 1.000000000000000000, 0.000000000000000000 ) ) ;
#885 = CARTESIAN_POINT ( 'NONE',  ( 65.00000000000000000, 0.000000000000000000, 0.000000000000000000 ) ) ;
#886 = CARTESIAN_POINT ( 'NONE',  ( 99.99999999999998579, 124.3999999999999915, 2.499999999999978684 ) ) ;
#887 = CARTESIAN_POINT ( 'NONE',  ( 95.54126587499995082, 1.846868145590750077, 7.625000001365592084 ) ) ;
#888 = CARTESIAN_POINT ( 'NONE',  ( 0.000000000000000000, 52.00000000000000711, 11.57481594606304398 ) ) ;
#889 = CARTESIAN_POINT ( 'NONE',  ( 99.99999999999995737, 4.458734125000016313, 9.187500001365592084 ) ) ;
#890 = CARTESIAN_POINT ( 'NONE',  ( 104.9952793366501851, 116.8754121666685393, -45.82500000273119412 ) ) ;
#891 = VECTOR ( 'NONE', #4255, 1000.000000000000000 ) ;
#892 = CARTESIAN_POINT ( 'NONE',  ( 104.4587341249999923, 91.49999999863440792, 1.846868145590726318 ) ) ;
#893 = FACE_OUTER_BOUND ( 'NONE', #12108, .T. ) ;
#894 = DIRECTION ( 'NONE',  ( 0.000000000000000000, 1.000000000000000000, 0.000000000000000000 ) ) ;
#895 = CARTESIAN_POINT ( 'NONE',  ( 13.14518615778179900, 33.95546875108393436, 5.444914386472293977 ) ) ;
#896 = VERTEX_POINT ( 'NONE', #16 ) ;
#897 = CARTESIAN_POINT ( 'NONE',  ( 102.3917468249999700, 122.9375000002731184, -9.833883627233146598E-15 ) ) ;
#898 = FACE_OUTER_BOUND ( 'NONE', #11315, .T. ) ;
#899 = EDGE_CURVE ( 'NONE', #6096, #2435, #10963, .T. ) ;
#900 = CARTESIAN_POINT ( 'NONE',  ( 185.7049497278729575, 35.89023437608393152, 9.295050272127047819 ) ) ;
#901 = ORIENTED_EDGE ( 'NONE', *, *, #24657, .T. ) ;
#902 = CARTESIAN_POINT ( 'NONE',  ( 195.8389268692911571, 53.50081894914646341, -15.00000000000000000 ) ) ;
#903 = CARTESIAN_POINT ( 'NONE',  ( 99.99999999999995737, -4.458734124999988779, 8.937500001365592084 ) ) ;
#904 = ORIENTED_EDGE ( 'NONE', *, *, #5003, .F. ) ;
#905 = CARTESIAN_POINT ( 'NONE',  ( 106.5389055433251002, 114.7507929638356785, -52.17500000273119554 ) ) ;
#906 = CARTESIAN_POINT ( 'NONE',  ( 5.444914386472297529, 35.54296875108393294, -13.14518615778179900 ) ) ;
#907 = DIRECTION ( 'NONE',  ( 0.000000000000000000, 0.000000000000000000, 1.000000000000000000 ) ) ;
#908 = CARTESIAN_POINT ( 'NONE',  ( 0.000000000000000000, 11.00000000000000355, 0.000000000000000000 ) ) ;
#909 = CIRCLE ( 'NONE', #6776, 11.57481594606304576 ) ;
#910 = CARTESIAN_POINT ( 'NONE',  ( 120.7049497278729575, 38.07304687608393579, -9.295050272127046043 ) ) ;
#911 = CARTESIAN_POINT ( 'NONE',  ( -13.14518615778179189, 38.42031250108393436, 5.444914386472304635 ) ) ;
#912 = CARTESIAN_POINT ( 'NONE',  ( 13.14518615778179544, 34.60039062608392868, -1.609821015232357215E-15 ) ) ;
#913 = CARTESIAN_POINT ( 'NONE',  ( 104.4587341249999781, 92.56249999863440792, -6.938893903907228378E-15 ) ) ;
#914 = CARTESIAN_POINT ( 'NONE',  ( 73.77260924613699444, 50.37415326813934513, -15.00000000000000000 ) ) ;
#915 = CARTESIAN_POINT ( 'NONE',  ( 108.0825317500000011, 107.3738262389971680, -48.47500000273118559 ) ) ;
#916 = CARTESIAN_POINT ( 'NONE',  ( 130.0000000000000000, -7.395377635281828788, -13.57481594606305997 ) ) ;
#917 = CARTESIAN_POINT ( 'NONE',  ( -8.049105076161786076E-16, 37.37851562608393863, -13.14518615778179544 ) ) ;
#918 = CARTESIAN_POINT ( 'NONE',  ( 98.15313185440923860, 4.458734125000016313, 6.500000001365592084 ) ) ;
#919 =( BOUNDED_CURVE ( )  B_SPLINE_CURVE ( 2, ( #11916, #9919, #25049, #22918, #18636, #14478, #15162, #6218, #16897 ),
 .UNSPECIFIED., .F., .F. ) 
 B_SPLINE_CURVE_WITH_KNOTS ( ( 3, 2, 2, 2, 3 ),
 ( 0.2499999999999998335, 0.2916666666666665741, 0.3333333333333332593, 0.3750000000000000000, 0.4166666666666667407 ),
 .UNSPECIFIED. ) 
 CURVE ( )  GEOMETRIC_REPRESENTATION_ITEM ( )  RATIONAL_B_SPLINE_CURVE ( ( 1.000000000000000222, 0.9238795325112864054, 1.000000000000000000, 0.9238795325112867385, 1.000000000000000000, 0.9238795325112867385, 1.000000000000000000, 0.9238795325112866275, 1.000000000000000000 ) ) 
 REPRESENTATION_ITEM ( '' )  );
#920 = CARTESIAN_POINT ( 'NONE',  ( 78.14518615778179367, 38.56914062608393579, -1.609821015232357215E-15 ) ) ;
#921 = CARTESIAN_POINT ( 'NONE',  ( 59.37712712842228058, 36.18789062716787441, -13.57481594606318254 ) ) ;
#922 = LINE ( 'NONE', #9735, #12130 ) ;
#923 = VERTEX_POINT ( 'NONE', #159 ) ;
#924 = CARTESIAN_POINT ( 'NONE',  ( -8.049105076161786076E-16, 33.40976562608393863, -13.14518615778179544 ) ) ;
#925 = CARTESIAN_POINT ( 'NONE',  ( 100.8561741729129153, 122.7000000010924623, -2.066987299999999195 ) ) ;
#926 = DIRECTION ( 'NONE',  ( 0.000000000000000000, -1.000000000000000000, 0.000000000000000000 ) ) ;
#927 = CARTESIAN_POINT ( 'NONE',  ( 195.0000000000000000, 39.36289062608393152, 13.14518615778179544 ) ) ;
#928 = CARTESIAN_POINT ( 'NONE',  ( 93.46109445667489979, 114.7507929638356785, -48.07499999726882578 ) ) ;
#929 = ORIENTED_EDGE ( 'NONE', *, *, #10839, .T. ) ;
#930 = EDGE_CURVE ( 'NONE', #20608, #21855, #13534, .T. ) ;
#931 = CARTESIAN_POINT ( 'NONE',  ( -9.598844408820458085, 32.96328124999999432, -9.598844408820458085 ) ) ;
#932 = CARTESIAN_POINT ( 'NONE',  ( -8.049105076161786076E-16, 32.41757812608393863, -13.14518615778179544 ) ) ;
#933 = ORIENTED_EDGE ( 'NONE', *, *, #20510, .T. ) ;
#934 = CARTESIAN_POINT ( 'NONE',  ( 124.5550856135277087, 33.45937500108394147, -13.14518615778179900 ) ) ;
#935 = CARTESIAN_POINT ( 'NONE',  ( 59.55508561352770158, 40.60312500108393863, -13.14518615778179722 ) ) ;
#936 = CARTESIAN_POINT ( 'NONE',  ( 208.1451861577817795, 34.74921875108395142, 5.444914386472293977 ) ) ;
#937 = ORIENTED_EDGE ( 'NONE', *, *, #26334, .F. ) ;
#938 = LINE ( 'NONE', #9609, #7507 ) ;
#939 = DIRECTION ( 'NONE',  ( 1.000000000000000000, 0.000000000000000000, 0.000000000000000000 ) ) ;
#940 = CARTESIAN_POINT ( 'NONE',  ( 121.2306103278992850, 50.37710889404841197, -14.99999999999737454 ) ) ;
#941 = CARTESIAN_POINT ( 'NONE',  ( 120.4011555911795455, 36.43593750216787441, 9.598844408820459861 ) ) ;
#942 = CARTESIAN_POINT ( 'NONE',  ( 104.9952793366501709, 116.8754121666685393, -49.82500000273120122 ) ) ;
#943 = CARTESIAN_POINT ( 'NONE',  ( 96.46446609406721961, -3.535533905932727539, 7.124999999999999112 ) ) ;
#944 = CARTESIAN_POINT ( 'NONE',  ( 5.622872871578054266, 32.11992187716787583, -13.57481594606286635 ) ) ;
#945 = CARTESIAN_POINT ( 'NONE',  ( 65.87652626536205958, 51.45968077935079066, 15.00000000000066258 ) ) ;
#946 = AXIS2_PLACEMENT_3D ( 'NONE', #27552, #14136, #5889 ) ;
#947 = VERTEX_POINT ( 'NONE', #24667 ) ;
#948 = CARTESIAN_POINT ( 'NONE',  ( 99.99999999999995737, -4.458734124999988779, 6.687500001365592084 ) ) ;
#949 = VERTEX_POINT ( 'NONE', #9403 ) ;
#950 = CARTESIAN_POINT ( 'NONE',  ( -4.459473413638155748, 36.00000000000000711, -12.68347323196786114 ) ) ;
#951 = CARTESIAN_POINT ( 'NONE',  ( 101.8468681455906903, 4.458734125000016313, 9.125000001365592084 ) ) ;
#952 = CYLINDRICAL_SURFACE ( 'NONE', #25355, 13.57481594606304576 ) ;
#953 = CARTESIAN_POINT ( 'NONE',  ( 104.9999999999999716, 94.93749999726880162, -2.071067811865478170 ) ) ;
#954 = CARTESIAN_POINT ( 'NONE',  ( 51.85481384221819923, 33.55859375108393294, -5.444914386472297529 ) ) ;
#955 = FACE_OUTER_BOUND ( 'NONE', #4282, .T. ) ;
#956 = EDGE_CURVE ( 'NONE', #3776, #27236, #5144, .T. ) ;
#957 = CARTESIAN_POINT ( 'NONE',  ( 99.99999999999998579, 101.5015231886685854, -46.62500000273119838 ) ) ;
#959 = CARTESIAN_POINT ( 'NONE',  ( 13.57481594606304931, 40.55351562499999574, 5.622872871577868636 ) ) ;
#958 = AXIS2_PLACEMENT_3D ( 'NONE', #9694, #13952, #26961 ) ;
#960 = CARTESIAN_POINT ( 'NONE',  ( 92.99999999999998579, 110.0000000000000000, -53.00000000000001421 ) ) ;
#961 = CARTESIAN_POINT ( 'NONE',  ( 3.979814445815163193, 50.00000000123243638, 13.01613927312660834 ) ) ;
#962 = CARTESIAN_POINT ( 'NONE',  ( 116.4251840539369596, 35.49335937499999005, 5.622872871577880183 ) ) ;
#963 = ORIENTED_EDGE ( 'NONE', *, *, #21718, .F. ) ;
#964 = EDGE_LOOP ( 'NONE', ( #1933, #20630, #27300, #22886 ) ) ;
#965 = CARTESIAN_POINT ( 'NONE',  ( 94.99999999999995737, 1.387778780781445676E-14, 8.000000000000000000 ) ) ;
#966 =( BOUNDED_CURVE ( )  B_SPLINE_CURVE ( 2, ( #4156, #10263, #18973, #1885, #12817, #21539, #27681, #2016, #10684, #19391, #25951 ),
 .UNSPECIFIED., .F., .F. ) 
 B_SPLINE_CURVE_WITH_KNOTS ( ( 3, 2, 2, 2, 2, 3 ),
 ( 0.3000000000000002109, 0.3200000000000002287, 0.3400000000000003020, 0.3600000000000002642, 0.3800000000000003375, 0.4000000000000003553 ),
 .UNSPECIFIED. ) 
 CURVE ( )  GEOMETRIC_REPRESENTATION_ITEM ( )  RATIONAL_B_SPLINE_CURVE ( ( 0.9999999999999994449, 0.9510565162951540863, 1.000000000000000000, 0.9510565162951535312, 1.000000000000000000, 0.9510565162951535312, 1.000000000000000000, 0.9510565162951535312, 1.000000000000000000, 0.9510565162951527540, 1.000000000000000888 ) ) 
 REPRESENTATION_ITEM ( '' )  );
#967 = CARTESIAN_POINT ( 'NONE',  ( -13.14518615778179544, 33.60820312608393579, 0.000000000000000000 ) ) ;
#968 = CARTESIAN_POINT ( 'NONE',  ( 13.57481594606304753, 34.40195312716787157, -5.622872871577873077 ) ) ;
#969 = CARTESIAN_POINT ( 'NONE',  ( 99.99999999999995737, -4.999999999999990230, 8.375000002731185944 ) ) ;
#970 = CARTESIAN_POINT ( 'NONE',  ( 139.2950502721270425, 34.50117187608393010, 9.295050272127046043 ) ) ;
#971 = EDGE_CURVE ( 'NONE', #15569, #6096, #15953, .T. ) ;
#972 = CARTESIAN_POINT ( 'NONE',  ( 74.59884440882045453, 32.07031250216787299, -9.598844408820458085 ) ) ;
#973 = EDGE_CURVE ( 'NONE', #20261, #12084, #4861, .T. ) ;
#974 = ORIENTED_EDGE ( 'NONE', *, *, #24272, .F. ) ;
#975 = CARTESIAN_POINT ( 'NONE',  ( 2.493653234604083739E-15, 37.32890625216786873, 13.57481594606304576 ) ) ;
#976 = CARTESIAN_POINT ( 'NONE',  ( 2.414731522848535132E-15, 39.95820312608393010, 13.14518615778179544 ) ) ;
#977 = CARTESIAN_POINT ( 'NONE',  ( 5.444914386472302859, 32.26875000108393721, 13.14518615778179189 ) ) ;
#978 = CARTESIAN_POINT ( 'NONE',  ( 182.9434479702998146, 35.99999999999997868, 5.307619621752330374 ) ) ;
#979 = CARTESIAN_POINT ( 'NONE',  ( 91.91746824999997045, 112.6261737610028320, -53.97499999726881725 ) ) ;
#980 = CARTESIAN_POINT ( 'NONE',  ( -13.57481594606304576, 38.71796875216787726, 0.000000000000000000 ) ) ;
#981 = CARTESIAN_POINT ( 'NONE',  ( 104.9999999999999716, 82.62500000273119838, -1.449011120738813565E-14 ) ) ;
#982 = CARTESIAN_POINT ( 'NONE',  ( 104.9999999999999716, 1.449011120738813565E-14, 5.625000002731185056 ) ) ;
#983 = DIRECTION ( 'NONE',  ( -0.000000000000000000, 1.000000000000000000, -0.000000000000000000 ) ) ;
#984 = EDGE_CURVE ( 'NONE', #27010, #13376, #11532, .T. ) ;
#985 = CARTESIAN_POINT ( 'NONE',  ( 120.9219080773008557, 36.00000000000001421, -9.794392408848658249 ) ) ;
#986 = LINE ( 'NONE', #24204, #26829 ) ;
#987 = CARTESIAN_POINT ( 'NONE',  ( 130.0000000000000000, 36.43593749999999432, 13.57481594606304576 ) ) ;
#988 = CARTESIAN_POINT ( 'NONE',  ( 9.598844408820456309, 32.76484374999999716, -9.598844408820458085 ) ) ;
#989 = CARTESIAN_POINT ( 'NONE',  ( -13.57481594606304576, 33.06249999999999289, 0.000000000000000000 ) ) ;
#990 = CARTESIAN_POINT ( 'NONE',  ( 13.14518615778179544, 35.59257812608393579, -1.609821015232357215E-15 ) ) ;
#991 = CARTESIAN_POINT ( 'NONE',  ( -8.049105076161786076E-16, 34.00507812608393721, -13.14518615778179544 ) ) ;
#992 = CARTESIAN_POINT ( 'NONE',  ( 9.295050272127046043, 35.49335937608393010, -9.295050272127046043 ) ) ;
#993 = CARTESIAN_POINT ( 'NONE',  ( 13.57481594606304753, 36.78320312716786589, -5.622872871577873077 ) ) ;
#994 = CARTESIAN_POINT ( 'NONE',  ( 13.57481594606304576, 37.52734375216787299, -1.662435489736055892E-15 ) ) ;
#995 = CARTESIAN_POINT ( 'NONE',  ( -13.57481594606304576, 35.44374999999999432, 0.000000000000000000 ) ) ;
#996 = CARTESIAN_POINT ( 'NONE',  ( 68.75563991928589758, 31.58960996655074993, -13.14518615778179544 ) ) ;
#997 = CARTESIAN_POINT ( 'NONE',  ( 99.99999999999998579, 118.4984768113314004, -53.87500000273118417 ) ) ;
#998 = CARTESIAN_POINT ( 'NONE',  ( 13.57481594606304931, 35.09648437716787583, 5.622872871577868636 ) ) ;
#999 = CARTESIAN_POINT ( 'NONE',  ( 116.4251840539369596, 37.92421875216787441, 0.000000000000000000 ) ) ;
#1000 = CARTESIAN_POINT ( 'NONE',  ( -13.57481594606304576, 33.90585937500000568, 5.622872871577880183 ) ) ;
#1001 = CARTESIAN_POINT ( 'NONE',  ( 93.00000000000000000, 112.2744378736303332, -46.59999999453763309 ) ) ;
#1002 = CARTESIAN_POINT ( 'NONE',  ( 139.2950502721270425, 33.11210937608393579, 9.295050272127046043 ) ) ;
#1003 = EDGE_CURVE ( 'NONE', #11898, #11725, #6213, .T. ) ;
#1004 = EDGE_LOOP ( 'NONE', ( #28123, #4594, #14143, #20923 ) ) ;
#1005 = CARTESIAN_POINT ( 'NONE',  ( 99.99999999999998579, 117.3602355696678643, -50.49999999999999289 ) ) ;
#1006 = CARTESIAN_POINT ( 'NONE',  ( 78.57481594606305464, 38.37070312716787157, -5.622872871577873966 ) ) ;
#1007 = CARTESIAN_POINT ( 'NONE',  ( 99.99999999999995737, 79.37500000273119838, 4.999999999999990230 ) ) ;
#1008 = CARTESIAN_POINT ( 'NONE',  ( 104.9999999999999858, 93.00000000000000000, -6.938893903907228378E-15 ) ) ;
#1009 = LINE ( 'NONE', #1284, #19265 ) ;
#1010 = EDGE_CURVE ( 'NONE', #26975, #16918, #24120, .T. ) ;
#1011 = CARTESIAN_POINT ( 'NONE',  ( 97.50236033167490746, 117.6869444889999841, -48.02499999726882152 ) ) ;
#1012 = CARTESIAN_POINT ( 'NONE',  ( 181.8548138422181921, 39.90859375108394147, -5.444914386472297529 ) ) ;
#1013 = CARTESIAN_POINT ( 'NONE',  ( -5.622872871577873077, 39.66054687716786731, 13.57481594606304753 ) ) ;
#1014 = ORIENTED_EDGE ( 'NONE', *, *, #14713, .T. ) ;
#1015 = DIRECTION ( 'NONE',  ( -0.000000000000000000, -0.000000000000000000, -1.000000000000000000 ) ) ;
#1016 = EDGE_CURVE ( 'NONE', #2438, #16078, #2443, .T. ) ;
#1017 = CARTESIAN_POINT ( 'NONE',  ( 103.5355339059327093, 3.535533905932755072, 13.62500000000000000 ) ) ;
#1018 = ORIENTED_EDGE ( 'NONE', *, *, #19485, .F. ) ;
#1019 = CARTESIAN_POINT ( 'NONE',  ( 13.14518615778179900, 37.92421875108392726, 5.444914386472293977 ) ) ;
#1020 = CARTESIAN_POINT ( 'NONE',  ( 208.1451861577817795, 40.10703125108393152, 5.444914386472293977 ) ) ;
#1021 = CARTESIAN_POINT ( 'NONE',  ( 9.295050272127046043, 32.31835937608393294, -9.295050272127046043 ) ) ;
#1022 = CARTESIAN_POINT ( 'NONE',  ( 94.99999999999995737, 1.387778780781445676E-14, 13.12500000273118417 ) ) ;
#1023 = CARTESIAN_POINT ( 'NONE',  ( 97.92893218813451028, -4.999999999999989342, 3.187499999999999556 ) ) ;
#1024 = CARTESIAN_POINT ( 'NONE',  ( 97.50000000000000000, 123.4500000021849502, -1.035533905932742416 ) ) ;
#1025 = CARTESIAN_POINT ( 'NONE',  ( 116.8548138422182063, 31.77265625108393365, -5.444914386472297529 ) ) ;
#1026 = CARTESIAN_POINT ( 'NONE',  ( 98.15313185440923860, 92.62499999863439371, -4.458734124999994997 ) ) ;
#1027 = EDGE_CURVE ( 'NONE', #12839, #23013, #730, .T. ) ;
#1028 = CARTESIAN_POINT ( 'NONE',  ( 97.93301269999999192, 123.2000000010924765, 0.8561741729129329626 ) ) ;
#1029 = CARTESIAN_POINT ( 'NONE',  ( -5.622872871578010745, 32.91367187499999858, -13.57481594606290898 ) ) ;
#1030 = CARTESIAN_POINT ( 'NONE',  ( 104.4587341249999781, -1.846868145590721655, 8.125000001365592084 ) ) ;
#1031 = CARTESIAN_POINT ( 'NONE',  ( 65.00000000000000000, 40.35507812608393152, -13.14518615778179544 ) ) ;
#1032 = CARTESIAN_POINT ( 'NONE',  ( 103.1528011352953342, 3.152801135295383084, 10.06250000136559208 ) ) ;
#1033 = CARTESIAN_POINT ( 'NONE',  ( 104.3262379212492590, 104.0454443415356991, -49.80000000546237970 ) ) ;
#1034 = CARTESIAN_POINT ( 'NONE',  ( 104.9999999999999716, 1.449011120738813565E-14, 4.499999999999999112 ) ) ;
#1035 = DIRECTION ( 'NONE',  ( -0.000000000000000000, -1.000000000000000000, -0.000000000000000000 ) ) ;
#1036 = CARTESIAN_POINT ( 'NONE',  ( 108.0825317499999869, 112.6261737610028320, -54.52499999726881441 ) ) ;
#1037 = CARTESIAN_POINT ( 'NONE',  ( 5.444914386472297529, 33.36015625108393579, -13.14518615778179900 ) ) ;
#1038 = ORIENTED_EDGE ( 'NONE', *, *, #17393, .T. ) ;
#1039 = FACE_OUTER_BOUND ( 'NONE', #4312, .T. ) ;
#1040 = CARTESIAN_POINT ( 'NONE',  ( -8.312177448680279460E-16, 36.03906250000000000, -13.57481594606304576 ) ) ;
#1041 = EDGE_CURVE ( 'NONE', #19008, #5192, #8486, .T. ) ;
#1042 = CARTESIAN_POINT ( 'NONE',  ( 208.1451861577817795, 36.13828125108393863, 5.444914386472293977 ) ) ;
#1043 = ORIENTED_EDGE ( 'NONE', *, *, #5070, .F. ) ;
#1044 = CARTESIAN_POINT ( 'NONE',  ( 191.1969456267529779, 54.09082899096177499, -15.00000000000000000 ) ) ;
#1045 = CARTESIAN_POINT ( 'NONE',  ( 98.15313185440925281, 4.458734125000016313, 12.50000000136559208 ) ) ;
#1046 = ORIENTED_EDGE ( 'NONE', *, *, #15737, .F. ) ;
#1047 = CARTESIAN_POINT ( 'NONE',  ( 104.9952793366501851, 116.8754121666685393, -46.07500000273119412 ) ) ;
#1048 = CARTESIAN_POINT ( 'NONE',  ( -5.444914386472299306, 35.93984375108392726, 13.14518615778179722 ) ) ;
#1049 = CARTESIAN_POINT ( 'NONE',  ( 189.3771271284221314, 40.15664062716787441, -13.57481594606304753 ) ) ;
#1050 = DIRECTION ( 'NONE',  ( -0.000000000000000000, 1.000000000000000000, -0.000000000000000000 ) ) ;
#1051 = CARTESIAN_POINT ( 'NONE',  ( 135.4449143864723055, 38.42031250108393436, 13.14518615778179189 ) ) ;
#1052 = CARTESIAN_POINT ( 'NONE',  ( -13.14518615778179722, 38.32109375108394289, -5.444914386472297529 ) ) ;
#1053 = CARTESIAN_POINT ( 'NONE',  ( 13.14518615778179900, 33.06250000108393294, -5.444914386472297529 ) ) ;
#1054 = CARTESIAN_POINT ( 'NONE',  ( 96.84719886470463734, 93.18749999863440792, 3.152801135295351997 ) ) ;
#1055 = FACE_OUTER_BOUND ( 'NONE', #17673, .T. ) ;
#1056 = CARTESIAN_POINT ( 'NONE',  ( 104.9952793366501709, 116.8754121666685393, -50.07500000273120122 ) ) ;
#1057 = VECTOR ( 'NONE', #15274, 1000.000000000000000 ) ;
#1058 = EDGE_LOOP ( 'NONE', ( #11036, #3352, #21158, #7142 ) ) ;
#1059 = DIRECTION ( 'NONE',  ( -1.000000000000000000, 0.000000000000000000, 0.000000000000000000 ) ) ;
#1060 = CARTESIAN_POINT ( 'NONE',  ( 5.444914386472297529, 35.74140625108393721, -13.14518615778179900 ) ) ;
#1061 = CARTESIAN_POINT ( 'NONE',  ( 101.8468681455907046, 4.458734125000016313, 5.375000001365592972 ) ) ;
#1062 = CARTESIAN_POINT ( 'NONE',  ( 78.14518615778180788, 36.23750000108393010, -5.444914386472297529 ) ) ;
#1063 = DIRECTION ( 'NONE',  ( 0.000000000000000000, 1.000000000000000000, 0.000000000000000000 ) ) ;
#1064 = CARTESIAN_POINT ( 'NONE',  ( 51.42518405393695957, 38.61874999999999147, 0.000000000000000000 ) ) ;
#1065 = CARTESIAN_POINT ( 'NONE',  ( 204.2950502721270425, 37.08085937608393579, -9.295050272127046043 ) ) ;
#1066 = ORIENTED_EDGE ( 'NONE', *, *, #26446, .F. ) ;
#1067 = CARTESIAN_POINT ( 'NONE',  ( 9.295050272127046043, 35.69179687608394147, -9.295050272127046043 ) ) ;
#1068 = CARTESIAN_POINT ( 'NONE',  ( 102.4999999999999858, 123.1000000021849416, -9.847140817659276890E-15 ) ) ;
#1069 = CARTESIAN_POINT ( 'NONE',  ( 2.493653234604083739E-15, 36.43593749999999432, 13.57481594606304576 ) ) ;
#1070 = CARTESIAN_POINT ( 'NONE',  ( 181.8548138422182205, 36.78320312608393294, 0.000000000000000000 ) ) ;
#1071 = CARTESIAN_POINT ( 'NONE',  ( 106.5389055433250860, 114.7507929638356785, -46.67499999726882720 ) ) ;
#1072 = CARTESIAN_POINT ( 'NONE',  ( -13.57481594606304576, 32.26874999999999716, 0.000000000000000000 ) ) ;
#1073 = CARTESIAN_POINT ( 'NONE',  ( 13.14518615778179900, 34.65000000108393152, -5.444914386472297529 ) ) ;
#1074 = VERTEX_POINT ( 'NONE', #26671 ) ;
#1075 = CARTESIAN_POINT ( 'NONE',  ( 107.0000000000000000, 112.2744378736303332, -45.89999999999999858 ) ) ;
#1076 = CARTESIAN_POINT ( 'NONE',  ( 59.55508561352770158, 39.80937500108393579, -13.14518615778179722 ) ) ;
#1077 = CARTESIAN_POINT ( 'NONE',  ( 99.99999999999998579, 122.9500000010924765, -2.066987299999998751 ) ) ;
#1078 = AXIS2_PLACEMENT_3D ( 'NONE', #23281, #14280, #24991 ) ;
#1079 = CARTESIAN_POINT ( 'NONE',  ( 189.5550856135277229, 35.04687500108393294, -13.14518615778179900 ) ) ;
#1080 = VERTEX_POINT ( 'NONE', #2586 ) ;
#1081 = CARTESIAN_POINT ( 'NONE',  ( 99.99999999999998579, 123.9500000010924765, 2.066987299999980099 ) ) ;
#1082 = CARTESIAN_POINT ( 'NONE',  ( 95.00000000000000000, 91.37499999726880162, -7.551217303480904118E-15 ) ) ;
#1083 = DIRECTION ( 'NONE',  ( -0.000000000000000000, 0.000000000000000000, -1.000000000000000000 ) ) ;
#1084 = CARTESIAN_POINT ( 'NONE',  ( 120.4011555911795455, 37.22968750216787726, 9.598844408820459861 ) ) ;
#1085 =( BOUNDED_SURFACE ( )  B_SPLINE_SURFACE ( 1, 2, ( 
 ( #6719, #2182, #19557, #17555, #23979, #15404, #4457, #14983, #25832, #13112, #6445, #17414, #21984, #23837, #17129, #24119, #10709, #21850, #10573, #4039, #12703, #6306, #4316, #4593, #19838, #19282, #23700, #23561, #17271, #8441, #10843, #325, #27981, #21428, #4176, #9010, #19695, #28117, #12838, #26260, #8863, #2326, #21565, #26404, #15260, #6862, #181, #13253, #1907, #2040, #8582, #8722, #39, #11123, #19415, #2462, #17702, #25974, #15116, #12973, #21707, #26112, #6578, #10982, #5166, #2606, #13829, #466, #4886, #11268, #26981, #13693, #3166, #22127, #20266, #20414, #26837, #5027, #7426, #7285, #15975, #16119, #24689, #19988, #22409, #18416, #22554, #15549, #9149, #1042, #11691, #20128, #17843, #18275, #900, #3021, #13549, #27122, #9570, #24258, #24825, #5310, #4740, #26546, #609, #752, #9424, #11838, #22273, #13971, #22699, #9285, #7140, #13400, #2878, #18124, #7001, #20561, #9715, #15695, #24398, #2747, #11410, #17981, #26690, #11550, #15835, #24543, #25106, #20839, #5594, #27262, #9985, #14260, #22980, #18694, #3447, #5450, #7718, #25243, #12112, #27397, #7857, #14117, #9851, #7571, #16268, #1316, #22841, #16551, #24966, #3308, #18557, #11979, #20703, #1185, #16410, #6209, #18384, #17023, #27739, #11807, #3935, #22951, #25078, #1155, #22810, #10608, #25588, #7540, #19315, #16889, #21461, #8199, #27876, #4075, #3278, #7686, #27089, #14878, #16238, #25726, #12454 ),
 ( #24935, #23458, #16378, #6072, #12737, #5566, #5422, #23593, #20671, #12594, #20530, #13941, #22667, #14091, #14229, #1939, #28016, #1012, #11947, #5275, #27232, #9820, #21179, #8482, #9681, #18527, #21319, #3413, #1660, #10320, #19027, #17171, #14738, #1801, #3139, #10466, #19174, #8338, #19875, #24295, #23873, #77, #10744, #26441, #8620, #9048, #4494, #21890, #361, #26298, #17740, #6759, #17308, #28154, #15443, #8759, #19731, #4776, #26149, #19456, #6901, #13006, #24158, #12869, #6341, #15015, #26008, #6616, #15589, #22164, #21599, #6480, #25872, #19594, #15154, #13152, #2642, #2076, #23737, #4352, #11304, #22021, #2222, #21746, #13437, #11160, #4635, #10886, #505, #17591, #9186, #2498, #20026, #4211, #17450, #15300, #11019, #2363, #24016, #216, #8903, #13293, #22449, #9462, #17880, #16011, #22595, #2782, #18457, #7464, #4923, #16159, #11446, #7174, #13586, #1079, #24725, #5486, #24436, #3064, #22736, #936, #7322, #9747, #9607, #18310, #27163, #27018, #22308, #5204, #20736, #792, #26586, #3202, #25009, #5347, #18165, #24866, #2916, #20167, #649, #14013, #11872, #20595, #13868, #20307, #7034, #7615, #11728, #16308, #9322, #14156, #20454, #22876, #3343, #12012, #1221, #15871, #26877, #18018, #15732, #26729, #24581, #5063, #13727, #11587, #10291, #21287, #18998, #1358, #12147, #27708, #21013, #3766, #8304, #10147, #3483, #1771, #25278, #8171, #25139, #18594, #27299 ) ),
 .UNSPECIFIED., .F., .F., .T. ) 
 B_SPLINE_SURFACE_WITH_KNOTS ( ( 2, 2 ),
 ( 3, 2, 2, 2, 2, 2, 2, 2, 2, 2, 2, 2, 2, 2, 2, 2, 2, 2, 2, 2, 2, 2, 2, 2, 2, 2, 2, 2, 2, 2, 2, 2, 2, 2, 2, 2, 2, 2, 2, 2, 2, 2, 2, 2, 2, 2, 2, 2, 2, 2, 2, 2, 2, 2, 2, 2, 2, 2, 2, 2, 2, 2, 2, 2, 2, 2, 2, 2, 2, 2, 2, 2, 2, 2, 2, 2, 2, 2, 2, 2, 2, 2, 2, 2, 2, 2, 2, 2, 2, 2, 2, 3 ),
 ( 0.000000000000000000, 1.000000000000000000 ),
 ( 0.000000000000000000, 0.01041666666666666609, 0.02083333333333333218, 0.03125000000000000000, 0.04166666666666666435, 0.05208333333333333565, 0.06250000000000000000, 0.07291666666666667129, 0.08333333333333332871, 0.09375000000000000000, 0.1041666666666666713, 0.1145833333333333287, 0.1250000000000000000, 0.1354166666666666574, 0.1458333333333333426, 0.1562500000000000000, 0.1666666666666666574, 0.1770833333333333426, 0.1875000000000000000, 0.1979166666666666574, 0.2083333333333333426, 0.2187500000000000000, 0.2291666666666666574, 0.2395833333333333426, 0.2500000000000000000, 0.2604166666666666852, 0.2708333333333333148, 0.2812500000000000000, 0.2916666666666666852, 0.3020833333333333148, 0.3125000000000000000, 0.3229166666666666852, 0.3333333333333333148, 0.3437500000000000000, 0.3541666666666666852, 0.3645833333333333148, 0.3750000000000000000, 0.3854166666666666852, 0.3958333333333333148, 0.4062500000000000000, 0.4166666666666666852, 0.4270833333333333148, 0.4375000000000000000, 0.4479166666666666852, 0.4583333333333333148, 0.4687500000000000000, 0.4791666666666666852, 0.4895833333333333148, 0.5000000000000000000, 0.5104166666666666297, 0.5208333333333333703, 0.5312500000000000000, 0.5416666666666666297, 0.5520833333333333703, 0.5625000000000000000, 0.5729166666666666297, 0.5833333333333333703, 0.5937500000000000000, 0.6041666666666666297, 0.6145833333333333703, 0.6250000000000000000, 0.6354166666666666297, 0.6458333333333333703, 0.6562500000000000000, 0.6666666666666666297, 0.6770833333333333703, 0.6875000000000000000, 0.6979166666666666297, 0.7083333333333333703, 0.7187500000000000000, 0.7291666666666666297, 0.7395833333333333703, 0.7500000000000000000, 0.7604166666666666297, 0.7708333333333333703, 0.7812500000000000000, 0.7916666666666666297, 0.8020833333333333703, 0.8125000000000000000, 0.8229166666666666297, 0.8333333333333333703, 0.8437500000000000000, 0.8541666666666666297, 0.8645833333333333703, 0.8750000000000000000, 0.8854166666666666297, 0.8958333333333333703, 0.9062500000000000000, 0.9166666666666666297, 0.9270833333333333703, 0.9375000000000000000, 0.9448587001587775980 ),
 .UNSPECIFIED. ) 
 GEOMETRIC_REPRESENTATION_ITEM ( )  RATIONAL_B_SPLINE_SURFACE ( (
 ( 1.000000000000000000, 0.9238795325112867385, 1.000000000000000000, 0.9238795325112867385, 1.000000000000000000, 0.9238795325112867385, 1.000000000000000000, 0.9238795325112867385, 1.000000000000000000, 0.9238795325112867385, 1.000000000000000000, 0.9238795325112867385, 1.000000000000000000, 0.9238795325112867385, 1.000000000000000000, 0.9238795325112867385, 1.000000000000000000, 0.9238795325112867385, 1.000000000000000000, 0.9238795325112867385, 1.000000000000000000, 0.9238795325112867385, 1.000000000000000000, 0.9238795325112867385, 1.000000000000000000, 0.9238795325112867385, 1.000000000000000000, 0.9238795325112867385, 1.000000000000000000, 0.9238795325112867385, 1.000000000000000000, 0.9238795325112867385, 1.000000000000000000, 0.9238795325112867385, 1.000000000000000000, 0.9238795325112867385, 1.000000000000000000, 0.9238795325112867385, 1.000000000000000000, 0.9238795325112867385, 1.000000000000000000, 0.9238795325112867385, 1.000000000000000000, 0.9238795325112867385, 1.000000000000000000, 0.9238795325112867385, 1.000000000000000000, 0.9238795325112867385, 1.000000000000000000, 0.9238795325112867385, 1.000000000000000000, 0.9238795325112867385, 1.000000000000000000, 0.9238795325112867385, 1.000000000000000000, 0.9238795325112867385, 1.000000000000000000, 0.9238795325112867385, 1.000000000000000000, 0.9238795325112867385, 1.000000000000000000, 0.9238795325112867385, 1.000000000000000000, 0.9238795325112867385, 1.000000000000000000, 0.9238795325112867385, 1.000000000000000000, 0.9238795325112867385, 1.000000000000000000, 0.9238795325112867385, 1.000000000000000000, 0.9238795325112867385, 1.000000000000000000, 0.9238795325112867385, 1.000000000000000000, 0.9238795325112867385, 1.000000000000000000, 0.9238795325112867385, 1.000000000000000000, 0.9238795325112867385, 1.000000000000000000, 0.9238795325112867385, 1.000000000000000000, 0.9238795325112867385, 1.000000000000000000, 0.9238795325112867385, 1.000000000000000000, 0.9238795325112867385, 1.000000000000000000, 0.9238795325112867385, 1.000000000000000000, 0.9238795325112867385, 1.000000000000000000, 0.9238795325112867385, 1.000000000000000000, 0.9238795325112867385, 1.000000000000000000, 0.9238795325112867385, 1.000000000000000000, 0.9238795325112867385, 1.000000000000000000, 0.9238795325112867385, 1.000000000000000000, 0.9238795325112867385, 1.000000000000000000, 0.9238795325112867385, 1.000000000000000000, 0.9238795325112867385, 1.000000000000000000, 0.9238795325112867385, 1.000000000000000000, 0.9238795325112867385, 1.000000000000000000, 0.9238795325112867385, 1.000000000000000000, 0.9238795325112867385, 1.000000000000000000, 0.9238795325112867385, 1.000000000000000000, 0.9238795325112867385, 1.000000000000000000, 0.9238795325112867385, 1.000000000000000000, 0.9238795325112867385, 1.000000000000000000, 0.9238795325112867385, 1.000000000000000000, 0.9238795325112867385, 1.000000000000000000, 0.9238795325112867385, 1.000000000000000000, 0.9238795325112867385, 1.000000000000000000, 0.9238795325112867385, 1.000000000000000000, 0.9238795325112867385, 1.000000000000000000, 0.9238795325112867385, 1.000000000000000000, 0.9238795325112867385, 1.000000000000000000, 0.9238795325112867385, 1.000000000000000000, 0.9238795325112867385, 1.000000000000000000, 0.9238795325112867385, 1.000000000000000000, 0.9238795325112867385, 1.000000000000000000, 0.9238795325112867385, 1.000000000000000000, 0.9238795325112867385, 1.000000000000000000, 0.9238795325112867385, 1.000000000000000000, 0.9238795325112867385, 1.000000000000000000, 0.9238795325112867385, 1.000000000000000000, 0.9238795325112867385, 1.000000000000000000, 0.9238795325112867385, 1.000000000000000000, 0.9238795325112867385, 1.000000000000000000, 0.9238795325112867385, 1.000000000000000000, 0.9238795325112867385, 1.000000000000000000, 0.9238795325112867385, 1.000000000000000000, 0.9238795325112867385, 1.000000000000000000, 0.9238795325112867385, 1.000000000000000000, 0.9238795325112867385, 1.000000000000000000, 0.9238795325112867385, 1.000000000000000000, 0.9238795325112867385, 1.000000000000000000, 0.9462258211652395667, 0.9684275895297407288),
 ( 1.000000000000000000, 0.9238795325112867385, 1.000000000000000000, 0.9238795325112867385, 1.000000000000000000, 0.9238795325112867385, 1.000000000000000000, 0.9238795325112867385, 1.000000000000000000, 0.9238795325112867385, 1.000000000000000000, 0.9238795325112867385, 1.000000000000000000, 0.9238795325112867385, 1.000000000000000000, 0.9238795325112867385, 1.000000000000000000, 0.9238795325112867385, 1.000000000000000000, 0.9238795325112867385, 1.000000000000000000, 0.9238795325112867385, 1.000000000000000000, 0.9238795325112867385, 1.000000000000000000, 0.9238795325112867385, 1.000000000000000000, 0.9238795325112867385, 1.000000000000000000, 0.9238795325112867385, 1.000000000000000000, 0.9238795325112867385, 1.000000000000000000, 0.9238795325112867385, 1.000000000000000000, 0.9238795325112867385, 1.000000000000000000, 0.9238795325112867385, 1.000000000000000000, 0.9238795325112867385, 1.000000000000000000, 0.9238795325112867385, 1.000000000000000000, 0.9238795325112867385, 1.000000000000000000, 0.9238795325112867385, 1.000000000000000000, 0.9238795325112867385, 1.000000000000000000, 0.9238795325112867385, 1.000000000000000000, 0.9238795325112867385, 1.000000000000000000, 0.9238795325112867385, 1.000000000000000000, 0.9238795325112867385, 1.000000000000000000, 0.9238795325112867385, 1.000000000000000000, 0.9238795325112867385, 1.000000000000000000, 0.9238795325112867385, 1.000000000000000000, 0.9238795325112867385, 1.000000000000000000, 0.9238795325112867385, 1.000000000000000000, 0.9238795325112867385, 1.000000000000000000, 0.9238795325112867385, 1.000000000000000000, 0.9238795325112867385, 1.000000000000000000, 0.9238795325112867385, 1.000000000000000000, 0.9238795325112867385, 1.000000000000000000, 0.9238795325112867385, 1.000000000000000000, 0.9238795325112867385, 1.000000000000000000, 0.9238795325112867385, 1.000000000000000000, 0.9238795325112867385, 1.000000000000000000, 0.9238795325112867385, 1.000000000000000000, 0.9238795325112867385, 1.000000000000000000, 0.9238795325112867385, 1.000000000000000000, 0.9238795325112867385, 1.000000000000000000, 0.9238795325112867385, 1.000000000000000000, 0.9238795325112867385, 1.000000000000000000, 0.9238795325112867385, 1.000000000000000000, 0.9238795325112867385, 1.000000000000000000, 0.9238795325112867385, 1.000000000000000000, 0.9238795325112867385, 1.000000000000000000, 0.9238795325112867385, 1.000000000000000000, 0.9238795325112867385, 1.000000000000000000, 0.9238795325112867385, 1.000000000000000000, 0.9238795325112867385, 1.000000000000000000, 0.9238795325112867385, 1.000000000000000000, 0.9238795325112867385, 1.000000000000000000, 0.9238795325112867385, 1.000000000000000000, 0.9238795325112867385, 1.000000000000000000, 0.9238795325112867385, 1.000000000000000000, 0.9238795325112867385, 1.000000000000000000, 0.9238795325112867385, 1.000000000000000000, 0.9238795325112867385, 1.000000000000000000, 0.9238795325112867385, 1.000000000000000000, 0.9238795325112867385, 1.000000000000000000, 0.9238795325112867385, 1.000000000000000000, 0.9238795325112867385, 1.000000000000000000, 0.9238795325112867385, 1.000000000000000000, 0.9238795325112867385, 1.000000000000000000, 0.9238795325112867385, 1.000000000000000000, 0.9238795325112867385, 1.000000000000000000, 0.9238795325112867385, 1.000000000000000000, 0.9238795325112867385, 1.000000000000000000, 0.9238795325112867385, 1.000000000000000000, 0.9238795325112867385, 1.000000000000000000, 0.9238795325112867385, 1.000000000000000000, 0.9238795325112867385, 1.000000000000000000, 0.9238795325112867385, 1.000000000000000000, 0.9238795325112867385, 1.000000000000000000, 0.9238795325112867385, 1.000000000000000000, 0.9238795325112867385, 1.000000000000000000, 0.9238795325112867385, 1.000000000000000000, 0.9238795325112867385, 1.000000000000000000, 0.9238795325112867385, 1.000000000000000000, 0.9238795325112867385, 1.000000000000000000, 0.9238795325112867385, 1.000000000000000000, 0.9238795325112867385, 1.000000000000000000, 0.9238795325112867385, 1.000000000000000000, 0.9238795325112867385, 1.000000000000000000, 0.9462258211652395667, 0.9684275895297407288) ) ) 
 REPRESENTATION_ITEM ( '' )  SURFACE ( )  );
#1086 = CARTESIAN_POINT ( 'NONE',  ( 51.42518405393695957, 40.30546875216787583, 0.000000000000000000 ) ) ;
#1087 = FACE_OUTER_BOUND ( 'NONE', #25613, .T. ) ;
#1088 = CARTESIAN_POINT ( 'NONE',  ( 66.89218335708966379, 53.66387243067953960, 14.99999999999997868 ) ) ;
#1089 = VERTEX_POINT ( 'NONE', #18103 ) ;
#1090 = EDGE_CURVE ( 'NONE', #17873, #18589, #5904, .T. ) ;
#1091 = ORIENTED_EDGE ( 'NONE', *, *, #15947, .T. ) ;
#1092 = CARTESIAN_POINT ( 'NONE',  ( 95.54126587499996504, 1.387778780781445676E-14, 5.437500001365591196 ) ) ;
#1093 = CARTESIAN_POINT ( 'NONE',  ( 102.0710678118654329, 5.000000000000018652, 12.81250000273118772 ) ) ;
#1094 = CARTESIAN_POINT ( 'NONE',  ( 101.8468681455906903, -4.458734124999987891, 2.750000001365592084 ) ) ;
#1095 = CARTESIAN_POINT ( 'NONE',  ( 132.2761468445512776, 51.46995505939284499, 15.00000000000097700 ) ) ;
#1096 = CARTESIAN_POINT ( 'NONE',  ( -6.338290792350127489, 36.00000000000002132, 11.53992004314986453 ) ) ;
#1097 = CARTESIAN_POINT ( 'NONE',  ( 65.00000000000000000, 33.01289062608393721, 13.14518615778179544 ) ) ;
#1098 = CIRCLE ( 'NONE', #168, 5.000000000000000888 ) ;
#1099 = CARTESIAN_POINT ( 'NONE',  ( -9.598844408820458085, 40.20625000216787726, -9.598844408820458085 ) ) ;
#1100 = CARTESIAN_POINT ( 'NONE',  ( 189.3771271284220177, 37.97382812499999716, 13.57481594606295161 ) ) ;
#1101 = CARTESIAN_POINT ( 'NONE',  ( 94.99999999999995737, 80.93750000000001421, -2.071067811865491493 ) ) ;
#1102 = CARTESIAN_POINT ( 'NONE',  ( 99.99999999999995737, 80.00000000000000000, 4.999999999999990230 ) ) ;
#1103 = CARTESIAN_POINT ( 'NONE',  ( -3.716534113788169336, 51.46663580899896573, 15.00000000000068212 ) ) ;
#1104 = CARTESIAN_POINT ( 'NONE',  ( 104.9999999999999716, 90.93749999726880162, -2.071067811865478170 ) ) ;
#1105 = CARTESIAN_POINT ( 'NONE',  ( 143.5748159460630404, 35.89023437499999858, -5.622872871577873077 ) ) ;
#1106 = ORIENTED_EDGE ( 'NONE', *, *, #23640, .F. ) ;
#1107 = EDGE_LOOP ( 'NONE', ( #12800, #23533, #16863, #391 ) ) ;
#1108 = FACE_OUTER_BOUND ( 'NONE', #23717, .T. ) ;
#1109 = CARTESIAN_POINT ( 'NONE',  ( -9.295050272127046043, 33.50898437608393010, -9.295050272127046043 ) ) ;
#1110 = CARTESIAN_POINT ( 'NONE',  ( 2.493653234604083739E-15, 35.74140625216787015, 13.57481594606304576 ) ) ;
#1111 = CARTESIAN_POINT ( 'NONE',  ( 99.99999999999995737, -4.999999999999990230, 5.375000002731185056 ) ) ;
#1112 = CARTESIAN_POINT ( 'NONE',  ( 130.0000000000000000, 34.40195312608393152, 13.14518615778179544 ) ) ;
#1113 = CARTESIAN_POINT ( 'NONE',  ( 65.00000000000000000, 38.76757812608393294, -13.14518615778179544 ) ) ;
#1114 = CARTESIAN_POINT ( 'NONE',  ( 104.9999999999999858, 2.071067811865485719, 14.56249999999999822 ) ) ;
#1115 = CARTESIAN_POINT ( 'NONE',  ( -13.14518615778179544, 38.96601562608393721, 0.000000000000000000 ) ) ;
#1116 = CARTESIAN_POINT ( 'NONE',  ( 13.14518615778179722, 32.36796875108393579, 5.444914386472293977 ) ) ;
#1117 = CARTESIAN_POINT ( 'NONE',  ( 182.6241215996508629, 36.00000000000000711, 4.513979326318628971 ) ) ;
#1118 = CARTESIAN_POINT ( 'NONE',  ( 91.91746824999997045, 112.6261737610028320, -51.97499999726882436 ) ) ;
#1119 = EDGE_LOOP ( 'NONE', ( #16453, #20874 ) ) ;
#1120 = CARTESIAN_POINT ( 'NONE',  ( -9.598844408820454532, 39.61093750216787868, 9.598844408820459861 ) ) ;
#1121 = CARTESIAN_POINT ( 'NONE',  ( 0.000000000000000000, 36.00000000000000000, 0.000000000000000000 ) ) ;
#1122 = CARTESIAN_POINT ( 'NONE',  ( 134.8599772695820889, 36.00000000000000000, 12.29462155906280252 ) ) ;
#1123 = CARTESIAN_POINT ( 'NONE',  ( 2.493653234604083739E-15, 33.36015625216786873, 13.57481594606304576 ) ) ;
#1124 = CARTESIAN_POINT ( 'NONE',  ( 102.0669872999999939, 124.2000000010924907, -0.8561741729129507261 ) ) ;
#1125 = CARTESIAN_POINT ( 'NONE',  ( 120.1606183911117114, 36.00000000000001421, -9.004033604612676100 ) ) ;
#1126 = CARTESIAN_POINT ( 'NONE',  ( 99.99999999999995737, 85.00000000000000000, -1.387778780781445676E-14 ) ) ;
#1127 = CARTESIAN_POINT ( 'NONE',  ( 97.71650635000000307, 124.8750000005462368, -9.540979117872439019E-15 ) ) ;
#1128 = CARTESIAN_POINT ( 'NONE',  ( 13.57481594606304931, 34.99726562500000426, 5.622872871577869525 ) ) ;
#1129 = CARTESIAN_POINT ( 'NONE',  ( 13.57481594606304753, 40.65273437499999432, -5.622872871577873966 ) ) ;
#1130 = CARTESIAN_POINT ( 'NONE',  ( -13.14518615778179544, 33.60820312608393579, 0.000000000000000000 ) ) ;
#1131 = CARTESIAN_POINT ( 'NONE',  ( 13.14518615778179544, 33.80664062608393294, -1.609821015232357215E-15 ) ) ;
#1132 = ADVANCED_FACE ( 'NONE', ( #5008 ), #13671, .F. ) ;
#1133 = CARTESIAN_POINT ( 'NONE',  ( -8.049105076161786076E-16, 35.59257812608393579, -13.14518615778179544 ) ) ;
#1134 = CARTESIAN_POINT ( 'NONE',  ( 9.598844408820456309, 35.24531250216787726, -9.598844408820458085 ) ) ;
#1135 = CARTESIAN_POINT ( 'NONE',  ( 5.622872871577786924, 37.37851562716787157, 13.57481594606313813 ) ) ;
#1136 = LINE ( 'NONE', #16219, #13292 ) ;
#1137 = CARTESIAN_POINT ( 'NONE',  ( 74.29505027212704249, 32.91367187608393152, 9.295050272127046043 ) ) ;
#1138 = ADVANCED_FACE ( 'NONE', ( #11527 ), #24418, .T. ) ;
#1139 =( BOUNDED_CURVE ( )  B_SPLINE_CURVE ( 2, ( #3619, #1763, #16297, #14700, #12004, #8164, #16721, #14147, #25418 ),
 .UNSPECIFIED., .F., .F. ) 
 B_SPLINE_CURVE_WITH_KNOTS ( ( 3, 2, 2, 2, 3 ),
 ( 0.8541666666666670737, 0.8645833333333337034, 0.8750000000000003331, 0.8854166666666669627, 0.8958333333333335924 ),
 .UNSPECIFIED. ) 
 CURVE ( )  GEOMETRIC_REPRESENTATION_ITEM ( )  RATIONAL_B_SPLINE_CURVE ( ( 0.9999999999999967804, 0.9238795325112899581, 1.000000000000000000, 0.9238795325112867385, 1.000000000000000000, 0.9238795325112867385, 1.000000000000000000, 0.9238795325112850731, 1.000000000000001554 ) ) 
 REPRESENTATION_ITEM ( '' )  );
#1140 = CARTESIAN_POINT ( 'NONE',  ( 104.4587341249999781, 95.31249999863440792, -6.938893903907228378E-15 ) ) ;
#1141 = CARTESIAN_POINT ( 'NONE',  ( 107.0000000000000000, 110.0000000000000000, -46.00000000000001421 ) ) ;
#1142 = CARTESIAN_POINT ( 'NONE',  ( 97.93301269999999192, 123.7000000010924765, -0.8561741729129505041 ) ) ;
#1143 = CARTESIAN_POINT ( 'NONE',  ( -8.312177448680279460E-16, 33.65781249999999147, -13.57481594606304576 ) ) ;
#1144 = CARTESIAN_POINT ( 'NONE',  ( 102.4976396683250783, 117.6869444889999841, -54.47499999726881725 ) ) ;
#1145 = CARTESIAN_POINT ( 'NONE',  ( 116.8548138422182063, 35.93984375108393436, -5.444914386472297529 ) ) ;
#1146 = ORIENTED_EDGE ( 'NONE', *, *, #5026, .T. ) ;
#1147 = CARTESIAN_POINT ( 'NONE',  ( 96.46446609406721961, 82.12500000000000000, 3.535533905932727539 ) ) ;
#1148 = DIRECTION ( 'NONE',  ( -0.000000000000000000, -1.000000000000000000, -0.000000000000000000 ) ) ;
#1149 = CARTESIAN_POINT ( 'NONE',  ( 98.15313185440925281, 83.62500000136560629, 4.458734124999987891 ) ) ;
#1150 = CARTESIAN_POINT ( 'NONE',  ( 104.9999999999999716, 91.06249999999997158, -2.071067811865478170 ) ) ;
#1151 = CARTESIAN_POINT ( 'NONE',  ( 124.3771271284220319, 38.46992187499999005, -13.57481594606295339 ) ) ;
#1152 = EDGE_CURVE ( 'NONE', #6963, #2879, #8797, .T. ) ;
#1153 = CIRCLE ( 'NONE', #25254, 13.57481594606304398 ) ;
#1154 = CARTESIAN_POINT ( 'NONE',  ( 104.3262379212492448, 115.9545556584642867, -53.70000000000000284 ) ) ;
#1155 = CARTESIAN_POINT ( 'NONE',  ( 200.4449143864723055, 32.36796875108393579, -13.14518615778179900 ) ) ;
#1156 = CARTESIAN_POINT ( 'NONE',  ( 9.598844408820459861, 39.80937500216786873, 9.598844408820456309 ) ) ;
#1157 = ORIENTED_EDGE ( 'NONE', *, *, #6712, .F. ) ;
#1158 = CARTESIAN_POINT ( 'NONE',  ( 96.46446609406721961, 3.535533905932755072, 7.875000000000000000 ) ) ;
#1159 = ORIENTED_EDGE ( 'NONE', *, *, #479, .F. ) ;
#1160 = CARTESIAN_POINT ( 'NONE',  ( -5.444914386472299306, 32.16953125108393152, 13.14518615778179722 ) ) ;
#1161 = CARTESIAN_POINT ( 'NONE',  ( 208.5748159460630688, 32.76484375216787015, -1.662435489736055892E-15 ) ) ;
#1162 = CARTESIAN_POINT ( 'NONE',  ( 104.9999999999999858, 2.071067811865485719, 13.68750000273118417 ) ) ;
#1163 = CARTESIAN_POINT ( 'NONE',  ( 96.46446609406721961, 3.535533905932755072, 14.00000000273118594 ) ) ;
#1164 = LINE ( 'NONE', #26817, #17544 ) ;
#1165 = CARTESIAN_POINT ( 'NONE',  ( 97.50000000000000000, 123.5000000021849615, -9.540979117872439019E-15 ) ) ;
#1166 = CARTESIAN_POINT ( 'NONE',  ( 219.9999999999999716, 50.00000000000000000, -10.00000000000000000 ) ) ;
#1167 = CARTESIAN_POINT ( 'NONE',  ( 101.8468681455907330, 91.12499999863439371, 4.458734124999980786 ) ) ;
#1168 = CARTESIAN_POINT ( 'NONE',  ( 98.96446609406727646, 123.5499999999999972, 2.499999999999977796 ) ) ;
#1169 = ADVANCED_FACE ( 'NONE', ( #7696 ), #11699, .F. ) ;
#1170 = CARTESIAN_POINT ( 'NONE',  ( 0.000000000000000000, 0.000000000000000000, 0.000000000000000000 ) ) ;
#1171 = CARTESIAN_POINT ( 'NONE',  ( 9.598844408820459861, 35.84062500216786873, 9.598844408820456309 ) ) ;
#1172 = CARTESIAN_POINT ( 'NONE',  ( 95.54126587499995082, -1.846868145590724986, 7.750000001365592084 ) ) ;
#1173 = CARTESIAN_POINT ( 'NONE',  ( 94.99999999999995737, 1.387778780781445676E-14, 15.00000000000000000 ) ) ;
#1174 = CARTESIAN_POINT ( 'NONE',  ( 95.54126587499996504, -1.846868145590724986, 11.50000000136559208 ) ) ;
#1175 = CARTESIAN_POINT ( 'NONE',  ( 102.1631189606246295, 116.6573956140660897, -49.10000000546237686 ) ) ;
#1176 = CARTESIAN_POINT ( 'NONE',  ( 104.4587341249999923, 93.49999999863442213, 1.846868145590726318 ) ) ;
#1177 = CARTESIAN_POINT ( 'NONE',  ( 208.5748159460630688, 39.80937499999999574, -1.662435489736055892E-15 ) ) ;
#1178 = LINE ( 'NONE', #18689, #2546 ) ;
#1179 = CARTESIAN_POINT ( 'NONE',  ( -13.14518615778179900, 33.55859375108393294, -5.444914386472297529 ) ) ;
#1180 = EDGE_CURVE ( 'NONE', #27294, #8379, #26712, .T. ) ;
#1181 = ORIENTED_EDGE ( 'NONE', *, *, #10839, .F. ) ;
#1182 = DIRECTION ( 'NONE',  ( -0.000000000000000000, 1.000000000000000000, -0.000000000000000000 ) ) ;
#1183 = AXIS2_PLACEMENT_3D ( 'NONE', #15127, #17283, #25985 ) ;
#1184 = EDGE_CURVE ( 'NONE', #21487, #8092, #26713, .T. ) ;
#1185 = CARTESIAN_POINT ( 'NONE',  ( 200.4449143864723055, 32.86406250108392868, 13.14518615778179189 ) ) ;
#1186 = ORIENTED_EDGE ( 'NONE', *, *, #27057, .T. ) ;
#1187 = CARTESIAN_POINT ( 'NONE',  ( -9.598844408820454532, 37.13046874999999147, 9.598844408820459861 ) ) ;
#1188 = CARTESIAN_POINT ( 'NONE',  ( 98.15313185440925281, -4.458734124999987891, 5.875000001365591196 ) ) ;
#1189 = VERTEX_POINT ( 'NONE', #19650 ) ;
#1190 = CARTESIAN_POINT ( 'NONE',  ( 108.0825317500000153, 110.0000000000000000, -48.37500000273119838 ) ) ;
#1191 = CARTESIAN_POINT ( 'NONE',  ( -9.295050272127046043, 35.69179687608393436, -9.295050272127046043 ) ) ;
#1192 = DIRECTION ( 'NONE',  ( 0.000000000000000000, 0.000000000000000000, 1.000000000000000000 ) ) ;
#1193 = FACE_OUTER_BOUND ( 'NONE', #18306, .T. ) ;
#1194 = CARTESIAN_POINT ( 'NONE',  ( 143.1451861577818079, 36.93203125108394147, 5.444914386472293977 ) ) ;
#1195 = CARTESIAN_POINT ( 'NONE',  ( -9.295050272127044266, 36.88242187608393152, 9.295050272127047819 ) ) ;
#1196 = CARTESIAN_POINT ( 'NONE',  ( 5.444914386472302859, 33.65781250108393152, 13.14518615778179189 ) ) ;
#1197 = CARTESIAN_POINT ( 'NONE',  ( 101.8468681455907330, 90.74999999863439371, -4.458734124999994997 ) ) ;
#1198 = CIRCLE ( 'NONE', #17089, 5.000000000000000000 ) ;
#1199 = CARTESIAN_POINT ( 'NONE',  ( 0.000000000000000000, -1.000000000000001998, 23.26794919243113213 ) ) ;
#1200 = CARTESIAN_POINT ( 'NONE',  ( -9.598844408820454532, 37.22968750216787726, 9.598844408820459861 ) ) ;
#1201 = CARTESIAN_POINT ( 'NONE',  ( 9.295050272127046043, 33.31054687608394005, -9.295050272127046043 ) ) ;
#1202 = CARTESIAN_POINT ( 'NONE',  ( 96.84719886470459471, -3.152801135295355994, 5.812500001365591196 ) ) ;
#1203 = CARTESIAN_POINT ( 'NONE',  ( 95.54126587499996504, 84.62500000136560629, -1.846868145590750077 ) ) ;
#1204 = CARTESIAN_POINT ( 'NONE',  ( 104.9999999999999716, 1.449011120738813565E-14, 6.625000002731185944 ) ) ;
#1205 = ADVANCED_FACE ( 'NONE', ( #5406 ), #3396, .T. ) ;
#1206 = CARTESIAN_POINT ( 'NONE',  ( 195.0000000000000000, 38.81718749999999574, 13.57481594606304576 ) ) ;
#1207 = DIRECTION ( 'NONE',  ( 0.000000000000000000, -1.000000000000000000, 0.000000000000000000 ) ) ;
#1208 = ORIENTED_EDGE ( 'NONE', *, *, #12780, .T. ) ;
#1209 = CARTESIAN_POINT ( 'NONE',  ( 2.414731522848535132E-15, 36.18789062608393436, 13.14518615778179544 ) ) ;
#1210 = CARTESIAN_POINT ( 'NONE',  ( 98.53841926354351699, 124.4500000010924765, -1.461580736456474794 ) ) ;
#1211 = CARTESIAN_POINT ( 'NONE',  ( 103.1528011352953484, 93.68749999863440792, -3.152801135295366208 ) ) ;
#1212 = CARTESIAN_POINT ( 'NONE',  ( 94.99999999999995737, -2.071067811865466624, 3.187500002731184612 ) ) ;
#1213 = CARTESIAN_POINT ( 'NONE',  ( 108.0825317500000011, 110.0000000000000000, -46.87499999726882294 ) ) ;
#1214 = DIRECTION ( 'NONE',  ( 0.000000000000000000, -1.000000000000000000, 3.469446951953611231E-16 ) ) ;
#1215 = CARTESIAN_POINT ( 'NONE',  ( -5.622872871577828668, 33.21132812499999432, 13.57481594606309194 ) ) ;
#1216 = VECTOR ( 'NONE', #28178, 999.9999999999998863 ) ;
#1217 = ORIENTED_EDGE ( 'NONE', *, *, #20623, .T. ) ;
#1218 = CARTESIAN_POINT ( 'NONE',  ( 130.0000000000000000, 38.81718749999999574, 13.57481594606304576 ) ) ;
#1219 = CARTESIAN_POINT ( 'NONE',  ( 94.99999999999995737, 1.387778780781445676E-14, 0.1250000027311851669 ) ) ;
#1220 = CARTESIAN_POINT ( 'NONE',  ( 108.0825317500000153, 110.0000000000000000, -54.25000000273119838 ) ) ;
#1221 = CARTESIAN_POINT ( 'NONE',  ( 195.0000000000000000, 33.01289062608393721, 13.14518615778179544 ) ) ;
#1222 = EDGE_LOOP ( 'NONE', ( #15278, #5218, #11333, #3911 ) ) ;
#1223 = DIRECTION ( 'NONE',  ( 0.000000000000000000, 0.000000000000000000, -1.000000000000000000 ) ) ;
#1224 = CARTESIAN_POINT ( 'NONE',  ( 9.180175813647991845, 50.00000000000000711, -15.00000000000000000 ) ) ;
#1225 = CARTESIAN_POINT ( 'NONE',  ( -5.622872871577873966, 33.70742187499999432, -13.57481594606304753 ) ) ;
#1226 = CARTESIAN_POINT ( 'NONE',  ( 124.3771271284221314, 36.48554687716787015, 13.57481594606304753 ) ) ;
#1227 = CIRCLE ( 'NONE', #17124, 7.000000000000006217 ) ;
#1228 = DIRECTION ( 'NONE',  ( 0.000000000000000000, 1.000000000000000000, 0.000000000000000000 ) ) ;
#1229 = DIRECTION ( 'NONE',  ( 6.938893903907232322E-16, -1.000000000000000000, 0.000000000000000000 ) ) ;
#1230 = CARTESIAN_POINT ( 'NONE',  ( 195.0000000000000000, 36.98164062608393721, 13.14518615778179544 ) ) ;
#1231 = ORIENTED_EDGE ( 'NONE', *, *, #22053, .F. ) ;
#1232 =( NAMED_UNIT ( * ) SI_UNIT ( $, .STERADIAN. ) SOLID_ANGLE_UNIT ( ) );
#1233 = CARTESIAN_POINT ( 'NONE',  ( 95.54126587499996504, 1.387778780781445676E-14, 1.437500001365591196 ) ) ;
#1234 = CARTESIAN_POINT ( 'NONE',  ( -7.394032042335738630, 36.00000000000004263, -11.20317769887113180 ) ) ;
#1235 = CARTESIAN_POINT ( 'NONE',  ( 95.54126587499996504, 84.43750000136560629, -1.387778780781445676E-14 ) ) ;
#1236 = CARTESIAN_POINT ( 'NONE',  ( 59.55508561352770158, 32.66562500108393863, -13.14518615778179900 ) ) ;
#1237 =( NAMED_UNIT ( * ) PLANE_ANGLE_UNIT ( ) SI_UNIT ( $, .RADIAN. ) );
#1238 = CARTESIAN_POINT ( 'NONE',  ( -13.14518615778179544, 39.95820312608393010, 0.000000000000000000 ) ) ;
#1239 = CARTESIAN_POINT ( 'NONE',  ( 87.00000000000000000, 123.0000000000000000, 14.99999999999999112 ) ) ;
#1240 = CARTESIAN_POINT ( 'NONE',  ( 2.232327155337096691, 35.99999999999998579, 12.98409812936892926 ) ) ;
#1241 = DIRECTION ( 'NONE',  ( -0.000000000000000000, 1.000000000000000000, 0.000000000000000000 ) ) ;
#1242 = CARTESIAN_POINT ( 'NONE',  ( 135.6228728715778971, 34.89804687499999147, 13.57481594606304576 ) ) ;
#1243 = ORIENTED_EDGE ( 'NONE', *, *, #7208, .F. ) ;
#1244 = CARTESIAN_POINT ( 'NONE',  ( 195.0000000000000000, 38.12265625216787157, 13.57481594606304576 ) ) ;
#1245 = CARTESIAN_POINT ( 'NONE',  ( 2.414731522848535132E-15, 32.21914062608393436, 13.14518615778179544 ) ) ;
#1246 = CARTESIAN_POINT ( 'NONE',  ( -5.622872871577873077, 33.31054687716787299, 13.57481594606304753 ) ) ;
#1247 =( BOUNDED_CURVE ( )  B_SPLINE_CURVE ( 2, ( #18921, #23073, #10495, #20933, #21351, #16784, #5961, #3965, #10350 ),
 .UNSPECIFIED., .F., .F. ) 
 B_SPLINE_CURVE_WITH_KNOTS ( ( 3, 2, 2, 2, 3 ),
 ( 0.1458333333333336757, 0.1562500000000002776, 0.1666666666666669072, 0.1770833333333335369, 0.1875000000000001388 ),
 .UNSPECIFIED. ) 
 CURVE ( )  GEOMETRIC_REPRESENTATION_ITEM ( )  RATIONAL_B_SPLINE_CURVE ( ( 0.9999999999999975575, 0.9238795325112891810, 1.000000000000000000, 0.9238795325112867385, 1.000000000000000000, 0.9238795325112867385, 1.000000000000000000, 0.9238795325112857393, 1.000000000000001110 ) ) 
 REPRESENTATION_ITEM ( '' )  );
#1248 = CARTESIAN_POINT ( 'NONE',  ( 104.9999999999999574, 2.071067811865491937, 3.687500002731185056 ) ) ;
#1249 = CARTESIAN_POINT ( 'NONE',  ( 124.5550856135277087, 40.60312500108393863, -13.14518615778179900 ) ) ;
#1250 = CARTESIAN_POINT ( 'NONE',  ( 59.55508561352770158, 39.90859375108393436, 13.14518615778179722 ) ) ;
#1251 = ADVANCED_FACE ( 'NONE', ( #2837, #13927 ), #2972, .F. ) ;
#1252 = DIRECTION ( 'NONE',  ( 0.000000000000000000, 1.000000000000000000, 0.000000000000000000 ) ) ;
#1253 = CARTESIAN_POINT ( 'NONE',  ( -9.295050272127046043, 39.66054687608393436, -9.295050272127046043 ) ) ;
#1254 = CARTESIAN_POINT ( 'NONE',  ( 107.0000000000000142, 110.0000000000000000, -47.00000000000000711 ) ) ;
#1255 = DIRECTION ( 'NONE',  ( 0.000000000000000000, -1.000000000000000000, 0.000000000000000000 ) ) ;
#1256 = CARTESIAN_POINT ( 'NONE',  ( 93.46109445667489979, 114.7507929638356785, -52.07499999726881867 ) ) ;
#1257 = CARTESIAN_POINT ( 'NONE',  ( 207.0772764098356049, 36.00000000000000000, -6.197985357349214297 ) ) ;
#1258 = CARTESIAN_POINT ( 'NONE',  ( 181.8548138422181921, 32.66562500108393863, 5.444914386472304635 ) ) ;
#1259 = CARTESIAN_POINT ( 'NONE',  ( 102.4999999999999858, 123.0000000000000000, -9.847140817659276890E-15 ) ) ;
#1260 = CARTESIAN_POINT ( 'NONE',  ( 97.93301269999999192, 122.9000000010924936, -0.8561741729129505041 ) ) ;
#1261 = CARTESIAN_POINT ( 'NONE',  ( 117.1404900439224974, 36.00000000000000000, -3.245221471866906349 ) ) ;
#1262 = DIRECTION ( 'NONE',  ( 0.000000000000000000, 0.000000000000000000, -1.000000000000000000 ) ) ;
#1263 = CARTESIAN_POINT ( 'NONE',  ( 99.99999999999995737, 4.458734125000016313, 11.18750000136559208 ) ) ;
#1264 = CARTESIAN_POINT ( 'NONE',  ( -13.57481594606304753, 33.01289062500000426, -5.622872871577873077 ) ) ;
#1265 = LINE ( 'NONE', #3115, #23908 ) ;
#1266 = CARTESIAN_POINT ( 'NONE',  ( 13.14518615778179900, 32.36796875108393579, 5.444914386472293977 ) ) ;
#1267 = CARTESIAN_POINT ( 'NONE',  ( -13.14518615778179544, 34.20351562608393436, 0.000000000000000000 ) ) ;
#1268 = CARTESIAN_POINT ( 'NONE',  ( 189.3771271284221314, 32.11992187499999574, -13.57481594606304753 ) ) ;
#1269 = CARTESIAN_POINT ( 'NONE',  ( 13.57481594606304753, 33.60820312716787583, -5.622872871577873077 ) ) ;
#1270 = CARTESIAN_POINT ( 'NONE',  ( 104.9999999999999716, 1.449011120738813565E-14, 2.625000002731185500 ) ) ;
#1271 = CARTESIAN_POINT ( 'NONE',  ( 99.99999999999995737, 82.68750000136560629, 4.458734124999988779 ) ) ;
#1272 = CARTESIAN_POINT ( 'NONE',  ( 65.00000000000000000, 32.02070312608393010, 13.14518615778179544 ) ) ;
#1273 = CARTESIAN_POINT ( 'NONE',  ( 97.50236033167492167, 117.6869444889999841, -47.77500000273119696 ) ) ;
#1274 = CARTESIAN_POINT ( 'NONE',  ( 104.3262379212492448, 104.0454443415356991, -46.30000000000001137 ) ) ;
#1275 = CARTESIAN_POINT ( 'NONE',  ( 97.93301269999999192, 124.5000000010924879, -0.8561741729129505041 ) ) ;
#1276 = CARTESIAN_POINT ( 'NONE',  ( 9.598844408820456309, 34.35234374999999574, -9.598844408820458085 ) ) ;
#1277 = CARTESIAN_POINT ( 'NONE',  ( 99.99999999999997158, 118.4984768113314004, -54.37499999726880873 ) ) ;
#1278 = CARTESIAN_POINT ( 'NONE',  ( 124.5550856135277087, 33.75703125108393721, 13.14518615778179722 ) ) ;
#1279 = ORIENTED_EDGE ( 'NONE', *, *, #27941, .T. ) ;
#1280 = CARTESIAN_POINT ( 'NONE',  ( -3.039397050802532529, 53.88964894337312472, -15.00000000000000533 ) ) ;
#1281 = DIRECTION ( 'NONE',  ( 0.000000000000000000, 1.000000000000000000, 0.000000000000000000 ) ) ;
#1282 = CARTESIAN_POINT ( 'NONE',  ( 104.9999999999999574, 79.56250000273121259, 2.071067811865462627 ) ) ;
#1283 = CARTESIAN_POINT ( 'NONE',  ( 120.7049497278729575, 39.66054687608393436, -9.295050272127046043 ) ) ;
#1284 = CARTESIAN_POINT ( 'NONE',  ( 99.99999999999998579, 128.0000000000000000, 0.5000000000000034417 ) ) ;
#1285 = CARTESIAN_POINT ( 'NONE',  ( 102.4976396683250783, 102.3130555110000159, -47.02499999726882152 ) ) ;
#1286 = CARTESIAN_POINT ( 'NONE',  ( 9.598844408820459861, 38.22187500216787015, 9.598844408820456309 ) ) ;
#1287 = VERTEX_POINT ( 'NONE', #1140 ) ;
#1288 = CARTESIAN_POINT ( 'NONE',  ( 96.46446609406721961, -3.535533905932727539, 10.12499999999999822 ) ) ;
#1289 = ORIENTED_EDGE ( 'NONE', *, *, #10160, .T. ) ;
#1290 = CARTESIAN_POINT ( 'NONE',  ( 5.444914386472297529, 32.56640625108394005, -13.14518615778179900 ) ) ;
#1291 = CARTESIAN_POINT ( 'NONE',  ( 181.8548138422181921, 39.80937500108392868, 5.444914386472304635 ) ) ;
#1292 = CARTESIAN_POINT ( 'NONE',  ( 103.5355339059327093, 3.535533905932755072, 13.75000000273118594 ) ) ;
#1293 = CARTESIAN_POINT ( 'NONE',  ( 96.46446609406721961, -3.535533905932727539, 13.25000000273118417 ) ) ;
#1294 = CARTESIAN_POINT ( 'NONE',  ( 116.8548138422182205, 39.75976562608393294, 0.000000000000000000 ) ) ;
#1295 = CARTESIAN_POINT ( 'NONE',  ( -8.049105076161786076E-16, 33.40976562608393863, -13.14518615778179544 ) ) ;
#1296 =( BOUNDED_CURVE ( )  B_SPLINE_CURVE ( 2, ( #5886, #1472, #21125, #8006, #14273 ),
 .UNSPECIFIED., .F., .F. ) 
 B_SPLINE_CURVE_WITH_KNOTS ( ( 3, 2, 3 ),
 ( 0.7499999999999997780, 0.7916666666666665186, 0.8333333333333333703 ),
 .UNSPECIFIED. ) 
 CURVE ( )  GEOMETRIC_REPRESENTATION_ITEM ( )  RATIONAL_B_SPLINE_CURVE ( ( 1.000000000000000444, 0.9238795325112862944, 1.000000000000000000, 0.9238795325112867385, 1.000000000000000000 ) ) 
 REPRESENTATION_ITEM ( '' )  );
#1297 = DIRECTION ( 'NONE',  ( 0.000000000000000000, 1.000000000000000000, 0.000000000000000000 ) ) ;
#1298 = CARTESIAN_POINT ( 'NONE',  ( 78.57481594606305464, 32.66562499999999858, -1.662435489736055892E-15 ) ) ;
#1299 = CARTESIAN_POINT ( 'NONE',  ( 98.96446609406727646, 124.3499999999999943, 2.499999999999977796 ) ) ;
#1300 = CARTESIAN_POINT ( 'NONE',  ( 195.0000000000000000, 32.21914062608393436, 13.14518615778179544 ) ) ;
#1301 = CARTESIAN_POINT ( 'NONE',  ( 129.4067442974502171, 35.99999999999998579, 13.13889047851776226 ) ) ;
#1302 = CARTESIAN_POINT ( 'NONE',  ( 101.8468681455906903, 4.458734125000016313, 6.375000001365592084 ) ) ;
#1303 = DIRECTION ( 'NONE',  ( 0.000000000000000000, 0.000000000000000000, -1.000000000000000000 ) ) ;
#1304 = CARTESIAN_POINT ( 'NONE',  ( 103.1528011352953342, 3.152801135295383084, 9.062500001365592084 ) ) ;
#1305 = CARTESIAN_POINT ( 'NONE',  ( 107.0000000000000142, 107.7255621263696526, -49.60000000546238397 ) ) ;
#1306 = CARTESIAN_POINT ( 'NONE',  ( 95.54126587500000767, 93.06249999863440792, -7.484931351350258973E-15 ) ) ;
#1307 = CARTESIAN_POINT ( 'NONE',  ( 96.46446609406721961, -3.535533905932727539, 4.124999999999998224 ) ) ;
#1308 = CARTESIAN_POINT ( 'NONE',  ( 0.000000000000000000, 40.99999999999999289, 0.000000000000000000 ) ) ;
#1309 = CARTESIAN_POINT ( 'NONE',  ( 13.14518615778179900, 32.46718750108393436, -5.444914386472297529 ) ) ;
#1310 = AXIS2_PLACEMENT_3D ( 'NONE', #21064, #21343, #23065 ) ;
#1311 = ORIENTED_EDGE ( 'NONE', *, *, #23920, .F. ) ;
#1312 = CARTESIAN_POINT ( 'NONE',  ( 95.54126587499995082, 83.75000000136560629, 1.846868145590724986 ) ) ;
#1313 = EDGE_CURVE ( 'NONE', #21025, #17571, #11932, .T. ) ;
#1314 = PRODUCT_DEFINITION_FORMATION_WITH_SPECIFIED_SOURCE ( 'ANY', '', #11245, .NOT_KNOWN. ) ;
#1315 = CARTESIAN_POINT ( 'NONE',  ( 97.50000000000000000, 124.3000000021849587, -9.540979117872439019E-15 ) ) ;
#1316 = CARTESIAN_POINT ( 'NONE',  ( 189.5550856135277229, 33.26093750108393721, -13.14518615778179900 ) ) ;
#1317 = ORIENTED_EDGE ( 'NONE', *, *, #20419, .T. ) ;
#1318 = EDGE_CURVE ( 'NONE', #3280, #28194, #19784, .T. ) ;
#1319 = CARTESIAN_POINT ( 'NONE',  ( 0.000000000000000000, 36.00000000000000000, -13.57481594606304576 ) ) ;
#1320 = CARTESIAN_POINT ( 'NONE',  ( 95.54126587499995082, 1.846868145590750077, 5.625000001365593860 ) ) ;
#1321 = EDGE_CURVE ( 'NONE', #8614, #8271, #20654, .T. ) ;
#1322 = EDGE_LOOP ( 'NONE', ( #4647, #13285, #16586, #4240 ) ) ;
#1323 = CARTESIAN_POINT ( 'NONE',  ( 93.46109445667491400, 105.2492070361643215, -49.17500000273119554 ) ) ;
#1324 = CARTESIAN_POINT ( 'NONE',  ( 5.444914386472302859, 32.07031250108393294, 13.14518615778179189 ) ) ;
#1325 = FACE_OUTER_BOUND ( 'NONE', #808, .T. ) ;
#1326 = CARTESIAN_POINT ( 'NONE',  ( -5.444914386472297529, 39.61093750108393152, -13.14518615778179722 ) ) ;
#1327 = EDGE_CURVE ( 'NONE', #13666, #8880, #3265, .T. ) ;
#1328 = VECTOR ( 'NONE', #13463, 1000.000000000000000 ) ;
#1329 = CARTESIAN_POINT ( 'NONE',  ( 13.14518615778179722, 37.92421875108393436, 5.444914386472293977 ) ) ;
#1330 = CARTESIAN_POINT ( 'NONE',  ( 13.14518615778179900, 40.40468750108393436, -5.444914386472297529 ) ) ;
#1331 = VECTOR ( 'NONE', #22313, 1000.000000000000000 ) ;
#1332 = CARTESIAN_POINT ( 'NONE',  ( 104.4587341249999923, 92.49999999863442213, 1.846868145590726318 ) ) ;
#1333 = FACE_OUTER_BOUND ( 'NONE', #21397, .T. ) ;
#1334 = EDGE_CURVE ( 'NONE', #22247, #2357, #13649, .T. ) ;
#1335 = DIRECTION ( 'NONE',  ( 0.000000000000000000, 0.000000000000000000, -1.000000000000000000 ) ) ;
#1336 =( BOUNDED_CURVE ( )  B_SPLINE_CURVE ( 2, ( #22643, #11635, #15781, #20357, #552, #4972, #19926, #13916, #22073 ),
 .UNSPECIFIED., .F., .F. ) 
 B_SPLINE_CURVE_WITH_KNOTS ( ( 3, 2, 2, 2, 3 ),
 ( 0.3958333333333331483, 0.4062499999999999445, 0.4166666666666667407, 0.4270833333333335369, 0.4375000000000003331 ),
 .UNSPECIFIED. ) 
 CURVE ( )  GEOMETRIC_REPRESENTATION_ITEM ( )  RATIONAL_B_SPLINE_CURVE ( ( 1.000000000000001110, 0.9238795325112855172, 1.000000000000000000, 0.9238795325112867385, 1.000000000000000000, 0.9238795325112867385, 1.000000000000000000, 0.9238795325112842960, 1.000000000000002442 ) ) 
 REPRESENTATION_ITEM ( '' )  );
#1337 = CARTESIAN_POINT ( 'NONE',  ( 6.944426393311538881, 31.75150625057403175, -11.16113171639042356 ) ) ;
#1338 = CARTESIAN_POINT ( 'NONE',  ( 103.1528011352953342, 3.152801135295383084, 2.312500001365592084 ) ) ;
#1339 = CARTESIAN_POINT ( 'NONE',  ( 101.8468681455907046, 83.37500000136563472, -4.458734125000016313 ) ) ;
#1340 = CARTESIAN_POINT ( 'NONE',  ( 5.444914386472302859, 35.24531250108393010, 13.14518615778179189 ) ) ;
#1341 = CARTESIAN_POINT ( 'NONE',  ( 70.62287287157778337, 39.26367187716788010, -13.57481594606312036 ) ) ;
#1342 = CARTESIAN_POINT ( 'NONE',  ( 70.31735157747590392, 54.47013368152370560, 14.99999999999998224 ) ) ;
#1343 = ORIENTED_EDGE ( 'NONE', *, *, #14706, .F. ) ;
#1344 = CARTESIAN_POINT ( 'NONE',  ( -5.444914386472297529, 35.04687500108393294, -13.14518615778179722 ) ) ;
#1345 = CARTESIAN_POINT ( 'NONE',  ( 97.50000000000000000, 122.7000000021849502, -9.540979117872439019E-15 ) ) ;
#1346 = DIRECTION ( 'NONE',  ( 0.000000000000000000, 0.000000000000000000, 1.000000000000000000 ) ) ;
#1347 = CARTESIAN_POINT ( 'NONE',  ( 97.92893218813451028, -4.999999999999989342, 3.312500002731184612 ) ) ;
#1348 = CARTESIAN_POINT ( 'NONE',  ( 0.000000000000000000, 23.00000000000000000, 0.000000000000000000 ) ) ;
#1349 = ADVANCED_FACE ( 'NONE', ( #7672 ), #27789, .T. ) ;
#1350 = FACE_OUTER_BOUND ( 'NONE', #4598, .T. ) ;
#1351 = DIRECTION ( 'NONE',  ( 1.000000000000000000, 0.000000000000000000, 0.000000000000000000 ) ) ;
#1352 = ORIENTED_EDGE ( 'NONE', *, *, #16537, .F. ) ;
#1353 = CARTESIAN_POINT ( 'NONE',  ( 65.00000000000000000, 39.36289062608393152, 13.14518615778179544 ) ) ;
#1354 = STYLED_ITEM ( 'NONE', ( #12417 ), #7649 ) ;
#1355 = ORIENTED_EDGE ( 'NONE', *, *, #12984, .F. ) ;
#1356 = CARTESIAN_POINT ( 'NONE',  ( 94.99999999999995737, 1.387778780781445676E-14, 1.999999999999998224 ) ) ;
#1357 = ADVANCED_FACE ( 'NONE', ( #5225 ), #7343, .T. ) ;
#1358 = CARTESIAN_POINT ( 'NONE',  ( 208.1451861577817795, 32.36796875108393579, 5.444914386472293977 ) ) ;
#1359 = ORIENTED_EDGE ( 'NONE', *, *, #24123, .F. ) ;
#1360 = CARTESIAN_POINT ( 'NONE',  ( 95.67376207875072680, 115.9545556584642867, -54.30000000000001137 ) ) ;
#1361 = EDGE_CURVE ( 'NONE', #13666, #4294, #9219, .T. ) ;
#1362 = DIRECTION ( 'NONE',  ( 0.000000000000000000, -0.000000000000000000, 1.000000000000000000 ) ) ;
#1363 = CARTESIAN_POINT ( 'NONE',  ( 200.3173515774759608, 54.47013368152369139, 14.99999999999995026 ) ) ;
#1364 = ADVANCED_FACE ( 'NONE', ( #11468 ), #9382, .T. ) ;
#1365 = CARTESIAN_POINT ( 'NONE',  ( 124.3771271284221314, 38.07304687716787583, 13.57481594606304753 ) ) ;
#1366 = DIRECTION ( 'NONE',  ( 0.000000000000000000, 1.000000000000000000, 0.000000000000000000 ) ) ;
#1367 = CARTESIAN_POINT ( 'NONE',  ( -9.180175813647997174, 55.00000000000000000, 10.00000000000000000 ) ) ;
#1368 = CARTESIAN_POINT ( 'NONE',  ( 204.2950502721270425, 38.66835937608393436, 9.295050272127046043 ) ) ;
#1369 = VERTEX_POINT ( 'NONE', #14342 ) ;
#1370 = CARTESIAN_POINT ( 'NONE',  ( 95.54126587499995082, -1.846868145590724986, 13.75000000136559208 ) ) ;
#1371 = CARTESIAN_POINT ( 'NONE',  ( -15.00000000000000355, 75.00000000000000000, -10.00000000000000000 ) ) ;
#1372 = VECTOR ( 'NONE', #4847, 1000.000000000000227 ) ;
#1373 = CARTESIAN_POINT ( 'NONE',  ( 104.3262379212492590, 104.0454443415356991, -51.80000000546237970 ) ) ;
#1374 = CARTESIAN_POINT ( 'NONE',  ( -8.312177448680279460E-16, 34.55078125216787299, -13.57481594606304576 ) ) ;
#1375 = CARTESIAN_POINT ( 'NONE',  ( 102.0710678118654613, 91.68749999726880162, 4.999999999999974243 ) ) ;
#1376 = CARTESIAN_POINT ( 'NONE',  ( 13.14518615778179900, 39.51171875108392584, 5.444914386472293977 ) ) ;
#1377 = DIRECTION ( 'NONE',  ( 0.000000000000000000, 1.000000000000000000, 0.000000000000000000 ) ) ;
#1378 = DIRECTION ( 'NONE',  ( 0.000000000000000000, 0.000000000000000000, -1.000000000000000000 ) ) ;
#1379 = CARTESIAN_POINT ( 'NONE',  ( 97.92893218813449607, 83.18750000000001421, 4.999999999999968914 ) ) ;
#1380 = CARTESIAN_POINT ( 'NONE',  ( 97.50236033167490746, 117.6869444889999841, -46.02499999726882152 ) ) ;
#1381 = ORIENTED_EDGE ( 'NONE', *, *, #16100, .T. ) ;
#1382 = VECTOR ( 'NONE', #2864, 1000.000000000000000 ) ;
#1383 = VERTEX_POINT ( 'NONE', #1545 ) ;
#1384 = CARTESIAN_POINT ( 'NONE',  ( 104.9999999999999716, 84.50000000000000000, -1.449011120738813565E-14 ) ) ;
#1385 = CARTESIAN_POINT ( 'NONE',  ( -13.57481594606304753, 40.15664062500000142, -5.622872871577873077 ) ) ;
#1386 = CARTESIAN_POINT ( 'NONE',  ( -13.57481594606304753, 32.31835937716786589, -5.622872871577873077 ) ) ;
#1387 = CARTESIAN_POINT ( 'NONE',  ( 96.46446609406721961, -3.535533905932727539, 7.250000002731185056 ) ) ;
#1388 = CARTESIAN_POINT ( 'NONE',  ( 116.8548138422182205, 31.82226562608393650, 0.000000000000000000 ) ) ;
#1389 = CARTESIAN_POINT ( 'NONE',  ( 51.85481384221819923, 36.53515625108392584, -5.444914386472297529 ) ) ;
#1390 = CARTESIAN_POINT ( 'NONE',  ( 65.00000000000000000, -7.395377635281828788, -13.57481594606305109 ) ) ;
#1391 = CARTESIAN_POINT ( 'NONE',  ( -8.049105076161786076E-16, 37.97382812608393721, -13.14518615778179544 ) ) ;
#1392 = CARTESIAN_POINT ( 'NONE',  ( 214.9999999999999716, 80.00000000000000000, 0.000000000000000000 ) ) ;
#1393 = DIRECTION ( 'NONE',  ( 0.000000000000000000, 1.000000000000000000, 0.000000000000000000 ) ) ;
#1394 = ADVANCED_FACE ( 'NONE', ( #10481 ), #18907, .T. ) ;
#1395 = CARTESIAN_POINT ( 'NONE',  ( 94.99999999999995737, 81.93750000000001421, -2.071067811865491493 ) ) ;
#1396 = CARTESIAN_POINT ( 'NONE',  ( -13.57481594606304753, 33.80664062499999289, -5.622872871577872189 ) ) ;
#1397 = DIRECTION ( 'NONE',  ( 0.000000000000000000, 1.000000000000000000, 0.000000000000000000 ) ) ;
#1398 = DIRECTION ( 'NONE',  ( -0.000000000000000000, -1.000000000000000000, -0.000000000000000000 ) ) ;
#1399 = CARTESIAN_POINT ( 'NONE',  ( 99.99999999999998579, 124.7999999999999972, -2.499999999999997780 ) ) ;
#1400 = CARTESIAN_POINT ( 'NONE',  ( 97.93301269999999192, 123.9000000010924794, -0.8561741729129505041 ) ) ;
#1401 = CARTESIAN_POINT ( 'NONE',  ( 131.4643377203195485, 35.99999999999999289, -13.46163418879038076 ) ) ;
#1402 = CONICAL_SURFACE ( 'NONE', #958, 12.50000000000001599, 0.7853981633974491672 ) ;
#1403 = CARTESIAN_POINT ( 'NONE',  ( 0.000000000000000000, 40.99999999999999289, -13.57481594606304576 ) ) ;
#1404 = CARTESIAN_POINT ( 'NONE',  ( 98.15313185440925281, 4.458734125000016313, 14.25000000136559208 ) ) ;
#1405 = CARTESIAN_POINT ( 'NONE',  ( 94.99999999999994316, -2.071067811865454633, 13.18750000273118594 ) ) ;
#1406 = EDGE_LOOP ( 'NONE', ( #23949, #8331, #11999, #3725 ) ) ;
#1407 = CARTESIAN_POINT ( 'NONE',  ( -11.14554687309540348, 36.00000000000000711, -7.260818043107225783 ) ) ;
#1408 = CARTESIAN_POINT ( 'NONE',  ( -8.312177448680279460E-16, 39.21406249999999716, -13.57481594606304576 ) ) ;
#1409 = CARTESIAN_POINT ( 'NONE',  ( -9.295050272127046043, 32.51679687608393721, -9.295050272127046043 ) ) ;
#1410 = CARTESIAN_POINT ( 'NONE',  ( 13.57481594606304576, 31.97109375216787441, -1.662435489736055892E-15 ) ) ;
#1411 = DIRECTION ( 'NONE',  ( 5.782411586589357392E-17, 0.000000000000000000, 1.000000000000000000 ) ) ;
#1412 = CARTESIAN_POINT ( 'NONE',  ( 103.1528011352953342, 81.81250000136559208, 3.152801135295355106 ) ) ;
#1413 = CARTESIAN_POINT ( 'NONE',  ( 78.14518615778179367, 37.13046875108393863, 5.444914386472293977 ) ) ;
#1414 = CARTESIAN_POINT ( 'NONE',  ( 91.91746824999998466, 112.6261737610028320, -51.47500000273119980 ) ) ;
#1415 = CARTESIAN_POINT ( 'NONE',  ( 104.9999999999999716, 94.06250000000000000, -2.071067811865478170 ) ) ;
#1416 =( BOUNDED_CURVE ( )  B_SPLINE_CURVE ( 2, ( #25405, #18575, #1200, #26997, #3608, #14557, #27278, #18707, #25120 ),
 .UNSPECIFIED., .F., .F. ) 
 B_SPLINE_CURVE_WITH_KNOTS ( ( 3, 2, 2, 2, 3 ),
 ( 0.3125000000000002220, 0.3229166666666668517, 0.3333333333333334259, 0.3437500000000000555, 0.3541666666666666852 ),
 .UNSPECIFIED. ) 
 CURVE ( )  GEOMETRIC_REPRESENTATION_ITEM ( )  RATIONAL_B_SPLINE_CURVE ( ( 0.9999999999999983347, 0.9238795325112884038, 1.000000000000000000, 0.9238795325112867385, 1.000000000000000000, 0.9238795325112867385, 1.000000000000000000, 0.9238795325112867385, 1.000000000000000000 ) ) 
 REPRESENTATION_ITEM ( '' )  );
#1417 = CARTESIAN_POINT ( 'NONE',  ( 99.99999999999998579, 123.3500000010924680, 2.066987299999980099 ) ) ;
#1418 = CARTESIAN_POINT ( 'NONE',  ( 92.99999999999998579, 110.0000000000000000, -52.49999999453763877 ) ) ;
#1419 = CARTESIAN_POINT ( 'NONE',  ( 116.8548138422182063, 33.55859375108393294, -5.444914386472297529 ) ) ;
#1420 = VERTEX_POINT ( 'NONE', #3951 ) ;
#1421 = CARTESIAN_POINT ( 'NONE',  ( 135.6228728715778118, 37.37851562716787157, 13.57481594606313813 ) ) ;
#1422 = FACE_OUTER_BOUND ( 'NONE', #15581, .T. ) ;
#1423 = CARTESIAN_POINT ( 'NONE',  ( 101.8468681455906903, 79.75000000136560629, 4.458734124999987891 ) ) ;
#1424 = CARTESIAN_POINT ( 'NONE',  ( 143.1451861577818079, 40.20625000108393010, -5.444914386472297529 ) ) ;
#1425 = CARTESIAN_POINT ( 'NONE',  ( 78.57481594606304043, 37.47773437716787726, 5.622872871577869525 ) ) ;
#1426 = VECTOR ( 'NONE', #983, 1000.000000000000000 ) ;
#1427 = CARTESIAN_POINT ( 'NONE',  ( 120.8198241863519939, 55.00000000000000000, 14.99999999999996803 ) ) ;
#1428 = VERTEX_POINT ( 'NONE', #14617 ) ;
#1429 = CARTESIAN_POINT ( 'NONE',  ( 103.5355339059327093, 3.535533905932755072, 7.624999999999999112 ) ) ;
#1430 = ORIENTED_EDGE ( 'NONE', *, *, #18321, .F. ) ;
#1431 = CARTESIAN_POINT ( 'NONE',  ( -13.14518615778179900, 33.55859375108393294, -5.444914386472297529 ) ) ;
#1432 = CARTESIAN_POINT ( 'NONE',  ( 204.5988444088204687, 32.66562500216787157, 9.598844408820456309 ) ) ;
#1433 = B_SPLINE_CURVE_WITH_KNOTS ( 'NONE', 3,
 ( #17705, #15552, #13832, #5029, #15697, #4888, #2608, #22275, #26839, #754, #13695, #2749, #2329, #184, #15977, #15408, #24691, #20132 ),
 .UNSPECIFIED., .F., .F.,
 ( 4, 2, 2, 2, 2, 2, 2, 2, 4 ),
 ( 0.000000000000000000, 0.004618502246277256425, 0.006927753369415884203, 0.009237004492554512849, 0.01039163005412378597, 0.01154625561569305736, 0.01385550673883160361, 0.01616475786197014985, 0.01847400898510869610 ),
 .UNSPECIFIED. ) ;
#1434 = CARTESIAN_POINT ( 'NONE',  ( 9.598844408820459861, 36.63437500216787157, 9.598844408820456309 ) ) ;
#1435 = CARTESIAN_POINT ( 'NONE',  ( 104.9999999999999716, 1.449011120738813565E-14, 12.62500000273118594 ) ) ;
#1436 = AXIS2_PLACEMENT_3D ( 'NONE', #21286, #10435, #12707 ) ;
#1437 = CARTESIAN_POINT ( 'NONE',  ( 135.4449143864723339, 38.71796875108393721, -13.14518615778179722 ) ) ;
#1438 = CARTESIAN_POINT ( 'NONE',  ( 99.99999999999998579, 123.3000000021849587, -2.499999999999997780 ) ) ;
#1439 = FACE_OUTER_BOUND ( 'NONE', #2427, .T. ) ;
#1440 = CARTESIAN_POINT ( 'NONE',  ( 95.54126587499999346, 93.74999999863439371, -1.846868145590737864 ) ) ;
#1441 = CARTESIAN_POINT ( 'NONE',  ( 101.7677669529663547, 123.8999999999999915, -1.767766952966370209 ) ) ;
#1442 = CARTESIAN_POINT ( 'NONE',  ( 204.5988444088204687, 37.32890624999999574, 9.598844408820456309 ) ) ;
#1443 = APPLICATION_PROTOCOL_DEFINITION ( 'draft international standard', 'automotive_design', 1998, #20626 ) ;
#1444 = CARTESIAN_POINT ( 'NONE',  ( 100.0000000000000000, 110.0000000000000000, -55.00000000000000711 ) ) ;
#1445 = CARTESIAN_POINT ( 'NONE',  ( 103.1528011352953342, 3.152801135295383084, 4.312500001365592084 ) ) ;
#1446 = FACE_OUTER_BOUND ( 'NONE', #17803, .T. ) ;
#1447 = EDGE_CURVE ( 'NONE', #17326, #28027, #2482, .T. ) ;
#1448 = CARTESIAN_POINT ( 'NONE',  ( 98.15313185440923860, -4.458734124999987891, 5.625000001365591196 ) ) ;
#1449 = CARTESIAN_POINT ( 'NONE',  ( 99.99999999999998579, 102.6397644303321215, -46.00000000546238255 ) ) ;
#1450 = CARTESIAN_POINT ( 'NONE',  ( 104.4587341249999923, 90.37499999863440792, -1.846868145590737198 ) ) ;
#1451 = CARTESIAN_POINT ( 'NONE',  ( 204.5988444088204403, 39.90859374999999432, -9.598844408820458085 ) ) ;
#1452 = LINE ( 'NONE', #25516, #24843 ) ;
#1453 = CARTESIAN_POINT ( 'NONE',  ( -5.622872871577873077, 40.85117187499999147, -13.57481594606304753 ) ) ;
#1454 = ORIENTED_EDGE ( 'NONE', *, *, #17510, .T. ) ;
#1455 = CARTESIAN_POINT ( 'NONE',  ( 95.54126587499995082, 84.62500000136560629, -1.846868145590750077 ) ) ;
#1456 = CARTESIAN_POINT ( 'NONE',  ( 114.9999999999999858, 99.99999999999998579, -45.00000000000000711 ) ) ;
#1457 = VERTEX_POINT ( 'NONE', #5814 ) ;
#1458 = ORIENTED_EDGE ( 'NONE', *, *, #9332, .T. ) ;
#1459 = CARTESIAN_POINT ( 'NONE',  ( 199.9250267836615649, 49.99999999893046976, -12.67776588291885176 ) ) ;
#1460 = CARTESIAN_POINT ( 'NONE',  ( 104.4587341249999639, 1.442382525525748735E-14, 7.187500001365592972 ) ) ;
#1461 = EDGE_LOOP ( 'NONE', ( #5171, #21822, #933, #7782 ) ) ;
#1462 = CARTESIAN_POINT ( 'NONE',  ( 108.0825317500000153, 110.0000000000000000, -44.37500000273119838 ) ) ;
#1463 =( BOUNDED_CURVE ( )  B_SPLINE_CURVE ( 2, ( #3272, #22370, #11799, #20523, #11941, #1005, #20662, #22231, #2710, #12486, #18925 ),
 .UNSPECIFIED., .F., .F. ) 
 B_SPLINE_CURVE_WITH_KNOTS ( ( 3, 2, 2, 2, 2, 3 ),
 ( 0.4000000000000003553, 0.4200000000000002065, 0.4400000000000000577, 0.4599999999999999645, 0.4799999999999997602, 0.4999999999999996669 ),
 .UNSPECIFIED. ) 
 CURVE ( )  GEOMETRIC_REPRESENTATION_ITEM ( )  RATIONAL_B_SPLINE_CURVE ( ( 0.9999999999999992228, 0.9510565162951543083, 1.000000000000000000, 0.9510565162951535312, 1.000000000000000000, 0.9510565162951535312, 1.000000000000000000, 0.9510565162951535312, 1.000000000000000000, 0.9510565162951543083, 0.9999999999999992228 ) ) 
 REPRESENTATION_ITEM ( '' )  );
#1464 = CARTESIAN_POINT ( 'NONE',  ( -13.14518615778179900, 34.94765625108392726, -5.444914386472297529 ) ) ;
#1465 = CARTESIAN_POINT ( 'NONE',  ( 104.9999999999999716, 1.449011120738813565E-14, 34.79898987322334136 ) ) ;
#1466 = CARTESIAN_POINT ( 'NONE',  ( -5.444914386472297529, 38.02343750108394005, -13.14518615778179722 ) ) ;
#1467 = CARTESIAN_POINT ( 'NONE',  ( 95.00472066334981491, 103.1245878333314465, -46.82500000273118701 ) ) ;
#1468 = CARTESIAN_POINT ( 'NONE',  ( 116.8548138422182205, 39.90859375108393436, -5.444914386472297529 ) ) ;
#1469 = CARTESIAN_POINT ( 'NONE',  ( -8.049105076161786076E-16, 32.41757812608393863, -13.14518615778179544 ) ) ;
#1470 = ORIENTED_EDGE ( 'NONE', *, *, #4634, .F. ) ;
#1471 = CARTESIAN_POINT ( 'NONE',  ( 59.37712712842213136, 37.18007812500000853, 13.57481594606304753 ) ) ;
#1472 = CARTESIAN_POINT ( 'NONE',  ( 101.0355339059327235, 123.1500000000000057, -2.500000000000001776 ) ) ;
#1473 = CARTESIAN_POINT ( 'NONE',  ( 93.00000000000001421, 107.7255621263696241, -50.90000000000001279 ) ) ;
#1474 = CARTESIAN_POINT ( 'NONE',  ( 2.414731522848535132E-15, 33.80664062608393294, 13.14518615778179544 ) ) ;
#1475 = CARTESIAN_POINT ( 'NONE',  ( 101.8468681455907046, -4.458734124999987891, 4.000000001365592084 ) ) ;
#1476 = EDGE_CURVE ( 'NONE', #8561, #27429, #3939, .T. ) ;
#1477 = CARTESIAN_POINT ( 'NONE',  ( 103.1528011352953342, 83.31250000136560629, -3.152801135295383084 ) ) ;
#1478 = CARTESIAN_POINT ( 'NONE',  ( 9.295050272127046043, 33.90585937608393152, -9.295050272127046043 ) ) ;
#1479 = CARTESIAN_POINT ( 'NONE',  ( -5.444914386472297529, 40.60312500108393863, -13.14518615778179900 ) ) ;
#1480 = CARTESIAN_POINT ( 'NONE',  ( 189.3771271284221598, 38.76757812499998579, 13.57481594606308128 ) ) ;
#1481 = ORIENTED_EDGE ( 'NONE', *, *, #18913, .F. ) ;
#1482 = EDGE_CURVE ( 'NONE', #4790, #7853, #17201, .T. ) ;
#1483 = CYLINDRICAL_SURFACE ( 'NONE', #6331, 5.000000000000000888 ) ;
#1484 = CARTESIAN_POINT ( 'NONE',  ( 97.93301270000000613, 123.8000000010924566, 0.8561741729129328515 ) ) ;
#1485 = CARTESIAN_POINT ( 'NONE',  ( 99.99999999999998579, 95.31249999863440792, 4.458734124999981674 ) ) ;
#1486 = CARTESIAN_POINT ( 'NONE',  ( 99.99999999999995737, 84.75000000000000000, -5.000000000000018652 ) ) ;
#1487 = CARTESIAN_POINT ( 'NONE',  ( 102.4976396683250783, 102.3130555110000159, -53.27499999726882862 ) ) ;
#1488 = DIRECTION ( 'NONE',  ( -0.000000000000000000, 1.000000000000000000, -0.000000000000000000 ) ) ;
#1489 = ORIENTED_EDGE ( 'NONE', *, *, #5307, .T. ) ;
#1490 = CARTESIAN_POINT ( 'NONE',  ( 70.44491438647229131, 39.71015625108393010, -13.14518615778179722 ) ) ;
#1491 = CARTESIAN_POINT ( 'NONE',  ( 65.00000000000000000, -7.395377635281828788, -7.517135062566165128E-15 ) ) ;
#1492 = EDGE_CURVE ( 'NONE', #8895, #21015, #19189, .T. ) ;
#1493 = DIRECTION ( 'NONE',  ( 0.000000000000000000, 0.000000000000000000, 1.000000000000000000 ) ) ;
#1494 = VERTEX_POINT ( 'NONE', #14891 ) ;
#1495 = CARTESIAN_POINT ( 'NONE',  ( 78.57481594606305464, 37.47773437500001137, -5.622872871577873966 ) ) ;
#1496 = CARTESIAN_POINT ( 'NONE',  ( -6.119843627700299216, 51.28708186914936817, -15.00000000000000178 ) ) ;
#1497 = CARTESIAN_POINT ( 'NONE',  ( 99.99999999999995737, 79.37500000273119838, 4.999999999999990230 ) ) ;
#1498 =( BOUNDED_SURFACE ( )  B_SPLINE_SURFACE ( 1, 2, ( 
 ( #23433, #8595, #1778, #1639, #19293, #25842, #27993, #10298, #12848, #25703, #2196, #27854, #21723, #17427, #6317, #3907, #12569, #10858, #2051, #10443, #21576, #10721, #19430, #19150, #17285, #54, #8734, #14852, #26125, #6592, #27717, #19004, #8178, #4470, #26272, #26418, #2337, #9024, #13413, #26560, #11424, #24271, #24410, #4899, #17716, #2761, #13562, #15419, #17855, #10995, #481, #5040, #24133, #20143, #2474, #624, #9299, #19709, #337, #24558, #23992, #2618, #21863, #22285, #193, #15708, #4753, #6877, #11135, #13266, #15849, #9163, #6733, #13128, #8875, #15562, #17995, #17567, #4609, #22139, #7012, #11281, #21998, #20001, #19850, #26704, #7153, #15227, #21671, #4425, #2148, #12671, #23527, #10810, #4143, #15083, #19664, #21528, #14804, #13079, #8404, #19525, #10953, #10397, #23803, #10538, #2005, #21818, #17522, #16955, #4005, #21251, #14949, #6138, #28085, #26225, #25656, #1733, #21396, #6684, #17381, #25795, #1874, #23945, #6547, #6, #19245, #24087, #12938, #4561, #26079, #2294, #19105, #27812, #6272, #6414, #25940, #8832, #27945, #147, #15370, #23668, #12806, #8267, #19381, #4281, #17093, #10672, #8691, #8548, #17237, #26370, #2575, #8975, #24659, #11379, #869, #19806, #17951, #18091, #24511, #2718, #5132, #4999, #13662, #13798, #22377, #17664, #20100, #16087, #24365, #21955, #26803, #20383, #719, #13518, #20237, #26514, #17811, #19954, #11518, #7108, #9394 ),
 ( #2434, #6971, #6829, #290, #24793, #577, #22522, #9541, #22097, #9258, #4853, #15806, #11236, #13223, #11094, #2849, #2987, #15519, #15943, #7253, #11661, #22239, #18242, #24227, #4708, #13368, #26950, #7393, #15666, #432, #26661, #9116, #16842, #12538, #16705, #5744, #27685, #18840, #21265, #10689, #10128, #14414, #27548, #19396, #1890, #10267, #8004, #8419, #19262, #6154, #3742, #8565, #25671, #17255, #10553, #14964, #23129, #12264, #18977, #19121, #10414, #21545, #23269, #17108, #27962, #8149, #25539, #3605, #3878, #27828, #25403, #6287, #23543, #20990, #4019, #5885, #12402, #1471, #25813, #1748, #2020, #14554, #8281, #23684, #16972, #23403, #4161, #14820, #12685, #12821, #21411, #21124, #28101, #1610, #6019, #14682, #11252, #4869, #13383, #26241, #4723, #10967, #2310, #4440, #24241, #19822, #22111, #24100, #165, #25956, #2590, #15386, #26529, #10825, #9131, #306, #4297, #19969, #4578, #17537, #21833, #15241, #2730, #17682, #23, #11395, #13533, #13092, #8992, #6985, #24381, #6699, #8705, #6561, #17824, #448, #26096, #26388, #13238, #21970, #19541, #11108, #15680, #6843, #17398, #15533, #23961, #21688, #19679, #9270, #6429, #8847, #2447, #12955, #22253, #20114, #591, #15098, #23819, #2163, #22824, #9555, #9833, #3292, #26820, #16250, #13676, #18397, #1298, #7267, #18540, #22535, #7700, #27244, #22392, #883, #20820, #17966, #22682, #7122, #11962, #26675, #3003 ) ),
 .UNSPECIFIED., .F., .F., .F. ) 
 B_SPLINE_SURFACE_WITH_KNOTS ( ( 2, 2 ),
 ( 3, 2, 2, 2, 2, 2, 2, 2, 2, 2, 2, 2, 2, 2, 2, 2, 2, 2, 2, 2, 2, 2, 2, 2, 2, 2, 2, 2, 2, 2, 2, 2, 2, 2, 2, 2, 2, 2, 2, 2, 2, 2, 2, 2, 2, 2, 2, 2, 2, 2, 2, 2, 2, 2, 2, 2, 2, 2, 2, 2, 2, 2, 2, 2, 2, 2, 2, 2, 2, 2, 2, 2, 2, 2, 2, 2, 2, 2, 2, 2, 2, 2, 2, 2, 2, 2, 2, 2, 2, 2, 2, 3 ),
 ( 0.000000000000000000, 1.000000000000000000 ),
 ( 0.000000000000000000, 0.01041666666666666609, 0.02083333333333333218, 0.03125000000000000000, 0.04166666666666666435, 0.05208333333333333565, 0.06250000000000000000, 0.07291666666666667129, 0.08333333333333332871, 0.09375000000000000000, 0.1041666666666666713, 0.1145833333333333287, 0.1250000000000000000, 0.1354166666666666574, 0.1458333333333333426, 0.1562500000000000000, 0.1666666666666666574, 0.1770833333333333426, 0.1875000000000000000, 0.1979166666666666574, 0.2083333333333333426, 0.2187500000000000000, 0.2291666666666666574, 0.2395833333333333426, 0.2500000000000000000, 0.2604166666666666852, 0.2708333333333333148, 0.2812500000000000000, 0.2916666666666666852, 0.3020833333333333148, 0.3125000000000000000, 0.3229166666666666852, 0.3333333333333333148, 0.3437500000000000000, 0.3541666666666666852, 0.3645833333333333148, 0.3750000000000000000, 0.3854166666666666852, 0.3958333333333333148, 0.4062500000000000000, 0.4166666666666666852, 0.4270833333333333148, 0.4375000000000000000, 0.4479166666666666852, 0.4583333333333333148, 0.4687500000000000000, 0.4791666666666666852, 0.4895833333333333148, 0.5000000000000000000, 0.5104166666666666297, 0.5208333333333333703, 0.5312500000000000000, 0.5416666666666666297, 0.5520833333333333703, 0.5625000000000000000, 0.5729166666666666297, 0.5833333333333333703, 0.5937500000000000000, 0.6041666666666666297, 0.6145833333333333703, 0.6250000000000000000, 0.6354166666666666297, 0.6458333333333333703, 0.6562500000000000000, 0.6666666666666666297, 0.6770833333333333703, 0.6875000000000000000, 0.6979166666666666297, 0.7083333333333333703, 0.7187500000000000000, 0.7291666666666666297, 0.7395833333333333703, 0.7500000000000000000, 0.7604166666666666297, 0.7708333333333333703, 0.7812500000000000000, 0.7916666666666666297, 0.8020833333333333703, 0.8125000000000000000, 0.8229166666666666297, 0.8333333333333333703, 0.8437500000000000000, 0.8541666666666666297, 0.8645833333333333703, 0.8750000000000000000, 0.8854166666666666297, 0.8958333333333333703, 0.9062500000000000000, 0.9166666666666666297, 0.9270833333333333703, 0.9375000000000000000, 0.9448586968893691873 ),
 .UNSPECIFIED. ) 
 GEOMETRIC_REPRESENTATION_ITEM ( )  RATIONAL_B_SPLINE_SURFACE ( (
 ( 1.000000000000000000, 0.9238795325112867385, 1.000000000000000000, 0.9238795325112867385, 1.000000000000000000, 0.9238795325112867385, 1.000000000000000000, 0.9238795325112867385, 1.000000000000000000, 0.9238795325112867385, 1.000000000000000000, 0.9238795325112867385, 1.000000000000000000, 0.9238795325112867385, 1.000000000000000000, 0.9238795325112867385, 1.000000000000000000, 0.9238795325112867385, 1.000000000000000000, 0.9238795325112867385, 1.000000000000000000, 0.9238795325112867385, 1.000000000000000000, 0.9238795325112867385, 1.000000000000000000, 0.9238795325112867385, 1.000000000000000000, 0.9238795325112867385, 1.000000000000000000, 0.9238795325112867385, 1.000000000000000000, 0.9238795325112867385, 1.000000000000000000, 0.9238795325112867385, 1.000000000000000000, 0.9238795325112867385, 1.000000000000000000, 0.9238795325112867385, 1.000000000000000000, 0.9238795325112867385, 1.000000000000000000, 0.9238795325112867385, 1.000000000000000000, 0.9238795325112867385, 1.000000000000000000, 0.9238795325112867385, 1.000000000000000000, 0.9238795325112867385, 1.000000000000000000, 0.9238795325112867385, 1.000000000000000000, 0.9238795325112867385, 1.000000000000000000, 0.9238795325112867385, 1.000000000000000000, 0.9238795325112867385, 1.000000000000000000, 0.9238795325112867385, 1.000000000000000000, 0.9238795325112867385, 1.000000000000000000, 0.9238795325112867385, 1.000000000000000000, 0.9238795325112867385, 1.000000000000000000, 0.9238795325112867385, 1.000000000000000000, 0.9238795325112867385, 1.000000000000000000, 0.9238795325112867385, 1.000000000000000000, 0.9238795325112867385, 1.000000000000000000, 0.9238795325112867385, 1.000000000000000000, 0.9238795325112867385, 1.000000000000000000, 0.9238795325112867385, 1.000000000000000000, 0.9238795325112867385, 1.000000000000000000, 0.9238795325112867385, 1.000000000000000000, 0.9238795325112867385, 1.000000000000000000, 0.9238795325112867385, 1.000000000000000000, 0.9238795325112867385, 1.000000000000000000, 0.9238795325112867385, 1.000000000000000000, 0.9238795325112867385, 1.000000000000000000, 0.9238795325112867385, 1.000000000000000000, 0.9238795325112867385, 1.000000000000000000, 0.9238795325112867385, 1.000000000000000000, 0.9238795325112867385, 1.000000000000000000, 0.9238795325112867385, 1.000000000000000000, 0.9238795325112867385, 1.000000000000000000, 0.9238795325112867385, 1.000000000000000000, 0.9238795325112867385, 1.000000000000000000, 0.9238795325112867385, 1.000000000000000000, 0.9238795325112867385, 1.000000000000000000, 0.9238795325112867385, 1.000000000000000000, 0.9238795325112867385, 1.000000000000000000, 0.9238795325112867385, 1.000000000000000000, 0.9238795325112867385, 1.000000000000000000, 0.9238795325112867385, 1.000000000000000000, 0.9238795325112867385, 1.000000000000000000, 0.9238795325112867385, 1.000000000000000000, 0.9238795325112867385, 1.000000000000000000, 0.9238795325112867385, 1.000000000000000000, 0.9238795325112867385, 1.000000000000000000, 0.9238795325112867385, 1.000000000000000000, 0.9238795325112867385, 1.000000000000000000, 0.9238795325112867385, 1.000000000000000000, 0.9238795325112867385, 1.000000000000000000, 0.9238795325112867385, 1.000000000000000000, 0.9238795325112867385, 1.000000000000000000, 0.9238795325112867385, 1.000000000000000000, 0.9238795325112867385, 1.000000000000000000, 0.9238795325112867385, 1.000000000000000000, 0.9238795325112867385, 1.000000000000000000, 0.9238795325112867385, 1.000000000000000000, 0.9238795325112867385, 1.000000000000000000, 0.9238795325112867385, 1.000000000000000000, 0.9238795325112867385, 1.000000000000000000, 0.9238795325112867385, 1.000000000000000000, 0.9238795325112867385, 1.000000000000000000, 0.9238795325112867385, 1.000000000000000000, 0.9238795325112867385, 1.000000000000000000, 0.9238795325112867385, 1.000000000000000000, 0.9238795325112867385, 1.000000000000000000, 0.9238795325112867385, 1.000000000000000000, 0.9238795325112867385, 1.000000000000000000, 0.9238795325112867385, 1.000000000000000000, 0.9238795325112867385, 1.000000000000000000, 0.9462258450566536361, 0.9684275698016389100),
 ( 1.000000000000000000, 0.9238795325112867385, 1.000000000000000000, 0.9238795325112867385, 1.000000000000000000, 0.9238795325112867385, 1.000000000000000000, 0.9238795325112867385, 1.000000000000000000, 0.9238795325112867385, 1.000000000000000000, 0.9238795325112867385, 1.000000000000000000, 0.9238795325112867385, 1.000000000000000000, 0.9238795325112867385, 1.000000000000000000, 0.9238795325112867385, 1.000000000000000000, 0.9238795325112867385, 1.000000000000000000, 0.9238795325112867385, 1.000000000000000000, 0.9238795325112867385, 1.000000000000000000, 0.9238795325112867385, 1.000000000000000000, 0.9238795325112867385, 1.000000000000000000, 0.9238795325112867385, 1.000000000000000000, 0.9238795325112867385, 1.000000000000000000, 0.9238795325112867385, 1.000000000000000000, 0.9238795325112867385, 1.000000000000000000, 0.9238795325112867385, 1.000000000000000000, 0.9238795325112867385, 1.000000000000000000, 0.9238795325112867385, 1.000000000000000000, 0.9238795325112867385, 1.000000000000000000, 0.9238795325112867385, 1.000000000000000000, 0.9238795325112867385, 1.000000000000000000, 0.9238795325112867385, 1.000000000000000000, 0.9238795325112867385, 1.000000000000000000, 0.9238795325112867385, 1.000000000000000000, 0.9238795325112867385, 1.000000000000000000, 0.9238795325112867385, 1.000000000000000000, 0.9238795325112867385, 1.000000000000000000, 0.9238795325112867385, 1.000000000000000000, 0.9238795325112867385, 1.000000000000000000, 0.9238795325112867385, 1.000000000000000000, 0.9238795325112867385, 1.000000000000000000, 0.9238795325112867385, 1.000000000000000000, 0.9238795325112867385, 1.000000000000000000, 0.9238795325112867385, 1.000000000000000000, 0.9238795325112867385, 1.000000000000000000, 0.9238795325112867385, 1.000000000000000000, 0.9238795325112867385, 1.000000000000000000, 0.9238795325112867385, 1.000000000000000000, 0.9238795325112867385, 1.000000000000000000, 0.9238795325112867385, 1.000000000000000000, 0.9238795325112867385, 1.000000000000000000, 0.9238795325112867385, 1.000000000000000000, 0.9238795325112867385, 1.000000000000000000, 0.9238795325112867385, 1.000000000000000000, 0.9238795325112867385, 1.000000000000000000, 0.9238795325112867385, 1.000000000000000000, 0.9238795325112867385, 1.000000000000000000, 0.9238795325112867385, 1.000000000000000000, 0.9238795325112867385, 1.000000000000000000, 0.9238795325112867385, 1.000000000000000000, 0.9238795325112867385, 1.000000000000000000, 0.9238795325112867385, 1.000000000000000000, 0.9238795325112867385, 1.000000000000000000, 0.9238795325112867385, 1.000000000000000000, 0.9238795325112867385, 1.000000000000000000, 0.9238795325112867385, 1.000000000000000000, 0.9238795325112867385, 1.000000000000000000, 0.9238795325112867385, 1.000000000000000000, 0.9238795325112867385, 1.000000000000000000, 0.9238795325112867385, 1.000000000000000000, 0.9238795325112867385, 1.000000000000000000, 0.9238795325112867385, 1.000000000000000000, 0.9238795325112867385, 1.000000000000000000, 0.9238795325112867385, 1.000000000000000000, 0.9238795325112867385, 1.000000000000000000, 0.9238795325112867385, 1.000000000000000000, 0.9238795325112867385, 1.000000000000000000, 0.9238795325112867385, 1.000000000000000000, 0.9238795325112867385, 1.000000000000000000, 0.9238795325112867385, 1.000000000000000000, 0.9238795325112867385, 1.000000000000000000, 0.9238795325112867385, 1.000000000000000000, 0.9238795325112867385, 1.000000000000000000, 0.9238795325112867385, 1.000000000000000000, 0.9238795325112867385, 1.000000000000000000, 0.9238795325112867385, 1.000000000000000000, 0.9238795325112867385, 1.000000000000000000, 0.9238795325112867385, 1.000000000000000000, 0.9238795325112867385, 1.000000000000000000, 0.9238795325112867385, 1.000000000000000000, 0.9238795325112867385, 1.000000000000000000, 0.9238795325112867385, 1.000000000000000000, 0.9238795325112867385, 1.000000000000000000, 0.9238795325112867385, 1.000000000000000000, 0.9238795325112867385, 1.000000000000000000, 0.9238795325112867385, 1.000000000000000000, 0.9238795325112867385, 1.000000000000000000, 0.9462258450566536361, 0.9684275698016389100) ) ) 
 REPRESENTATION_ITEM ( '' )  SURFACE ( )  );
#1499 = AXIS2_PLACEMENT_3D ( 'NONE', #4264, #19936, #23788 ) ;
#1500 = CARTESIAN_POINT ( 'NONE',  ( 135.6228728715778686, 33.70742187716787441, -13.57481594606304753 ) ) ;
#1501 =( BOUNDED_CURVE ( )  B_SPLINE_CURVE ( 2, ( #1852, #10515, #4538, #21934, #6393, #26055, #11071, #23778, #19781 ),
 .UNSPECIFIED., .F., .F. ) 
 B_SPLINE_CURVE_WITH_KNOTS ( ( 3, 2, 2, 2, 3 ),
 ( 0.5714285714285713969, 0.5803571428571429047, 0.5892857142857143016, 0.5982142857142856984, 0.6071428571428570953 ),
 .UNSPECIFIED. ) 
 CURVE ( )  GEOMETRIC_REPRESENTATION_ITEM ( )  RATIONAL_B_SPLINE_CURVE ( ( 1.000000000000000000, 0.9238795325112867385, 1.000000000000000000, 0.9238795325112867385, 1.000000000000000000, 0.9238795325112867385, 1.000000000000000000, 0.9238795325112867385, 1.000000000000000000 ) ) 
 REPRESENTATION_ITEM ( '' )  );
#1502 = CARTESIAN_POINT ( 'NONE',  ( 104.9999999999999716, 90.06249999999998579, -2.071067811865478170 ) ) ;
#1503 = DIRECTION ( 'NONE',  ( -0.8490667072653959035, 1.618318251311064231E-06, -0.5282856486891157610 ) ) ;
#1504 = CARTESIAN_POINT ( 'NONE',  ( 200.4449143864723055, 36.53515625108393294, -13.14518615778179900 ) ) ;
#1505 = EDGE_CURVE ( 'NONE', #756, #13519, #5408, .T. ) ;
#1506 = VERTEX_POINT ( 'NONE', #23202 ) ;
#1507 = ORIENTED_EDGE ( 'NONE', *, *, #23758, .T. ) ;
#1508 = CARTESIAN_POINT ( 'NONE',  ( 94.99999999999995737, 83.93750000000001421, -2.071067811865491493 ) ) ;
#1509 = CARTESIAN_POINT ( 'NONE',  ( 9.598844408820456309, 33.65781250216787157, -9.598844408820458085 ) ) ;
#1510 = EDGE_CURVE ( 'NONE', #3788, #10198, #24708, .T. ) ;
#1511 = CARTESIAN_POINT ( 'NONE',  ( 104.4587341249999639, 82.93750000136560629, -1.442382525525748735E-14 ) ) ;
#1512 = CARTESIAN_POINT ( 'NONE',  ( 102.0669872999999797, 122.7500000010924737, -9.794112055954760458E-15 ) ) ;
#1513 = CARTESIAN_POINT ( 'NONE',  ( 9.295050272127047819, 40.25585937608393294, 9.295050272127046043 ) ) ;
#1514 = DIRECTION ( 'NONE',  ( 1.000000000000000000, -0.000000000000000000, -5.782411586589357392E-17 ) ) ;
#1515 = CARTESIAN_POINT ( 'NONE',  ( 3.829562757991920474, 36.00000000000001421, 12.63428651647591749 ) ) ;
#1516 = CARTESIAN_POINT ( 'NONE',  ( 103.5355339059327235, 93.99999999726881583, -3.535533905932738197 ) ) ;
#1517 = CARTESIAN_POINT ( 'NONE',  ( 139.5988444088204687, 32.56640625000000000, 9.598844408820456309 ) ) ;
#1518 = EDGE_CURVE ( 'NONE', #12537, #26666, #15283, .T. ) ;
#1519 = AXIS2_PLACEMENT_3D ( 'NONE', #14564, #16851, #14693 ) ;
#1520 = EDGE_LOOP ( 'NONE', ( #5314, #1279, #18882, #7280 ) ) ;
#1521 = PRODUCT_DEFINITION_CONTEXT ( 'detailed design', #52, 'design' ) ;
#1522 = CARTESIAN_POINT ( 'NONE',  ( 5.622872871577871301, 38.37070312499999147, -13.57481594606304753 ) ) ;
#1523 = CARTESIAN_POINT ( 'NONE',  ( 2.493653234604083739E-15, 32.56640625216787299, 13.57481594606304576 ) ) ;
#1524 = ORIENTED_EDGE ( 'NONE', *, *, #2921, .T. ) ;
#1525 = CARTESIAN_POINT ( 'NONE',  ( 97.92893218813451028, 5.000000000000018652, 5.937500002731185056 ) ) ;
#1526 = CARTESIAN_POINT ( 'NONE',  ( 139.2950502721270425, 38.66835937608393436, 9.295050272127046043 ) ) ;
#1527 = CARTESIAN_POINT ( 'NONE',  ( 78.14518615778179367, 35.39414062608393152, -1.609821015232357215E-15 ) ) ;
#1528 = LINE ( 'NONE', #1390, #19800 ) ;
#1529 = CARTESIAN_POINT ( 'NONE',  ( -13.14518615778179900, 34.94765625108392726, -5.444914386472297529 ) ) ;
#1530 = CARTESIAN_POINT ( 'NONE',  ( 194.8277102352230941, 36.00000000000000000, -13.51468191220837056 ) ) ;
#1531 = DIRECTION ( 'NONE',  ( 0.000000000000000000, 0.000000000000000000, -1.000000000000000000 ) ) ;
#1532 = FACE_OUTER_BOUND ( 'NONE', #20108, .T. ) ;
#1533 = CARTESIAN_POINT ( 'NONE',  ( 96.46446609406721961, 82.12500000000000000, 3.535533905932727539 ) ) ;
#1534 = ORIENTED_EDGE ( 'NONE', *, *, #25184, .T. ) ;
#1535 = FACE_OUTER_BOUND ( 'NONE', #27394, .T. ) ;
#1536 = CARTESIAN_POINT ( 'NONE',  ( -13.14518615778179900, 39.71015625108393010, -5.444914386472297529 ) ) ;
#1537 = CARTESIAN_POINT ( 'NONE',  ( 132.2323271553379698, 35.99999999999999289, 12.98409812936879426 ) ) ;
#1538 = CARTESIAN_POINT ( 'NONE',  ( 98.23223304703363112, 123.3069999999781459, -1.767766952966370209 ) ) ;
#1539 = CARTESIAN_POINT ( 'NONE',  ( 100.8561741729129295, 124.2000000010924907, 2.066987299999979211 ) ) ;
#1540 = CARTESIAN_POINT ( 'NONE',  ( 101.4615807364564546, 124.4500000010924765, -1.461580736456474794 ) ) ;
#1541 = AXIS2_PLACEMENT_3D ( 'NONE', #2821, #839, #9509 ) ;
#1542 =( BOUNDED_CURVE ( )  B_SPLINE_CURVE ( 2, ( #3779, #12436, #18609, #21027, #7771, #19010, #8743, #12991, #15573 ),
 .UNSPECIFIED., .F., .F. ) 
 B_SPLINE_CURVE_WITH_KNOTS ( ( 3, 2, 2, 2, 3 ),
 ( 0.1500000000000001332, 0.1750000000000001554, 0.2000000000000001776, 0.2250000000000001998, 0.2500000000000002220 ),
 .UNSPECIFIED. ) 
 CURVE ( )  GEOMETRIC_REPRESENTATION_ITEM ( )  RATIONAL_B_SPLINE_CURVE ( ( 0.9999999999999995559, 0.9238795325112871826, 1.000000000000000000, 0.9238795325112867385, 1.000000000000000000, 0.9238795325112867385, 1.000000000000000000, 0.9238795325112860723, 1.000000000000000666 ) ) 
 REPRESENTATION_ITEM ( '' )  );
#1543 = DIRECTION ( 'NONE',  ( -0.000000000000000000, -1.000000000000000000, -0.000000000000000000 ) ) ;
#1544 = CARTESIAN_POINT ( 'NONE',  ( 103.5355339059327093, 3.535533905932755072, 12.62499999999999822 ) ) ;
#1545 = CARTESIAN_POINT ( 'NONE',  ( 107.0000000000000142, 110.0000000000000000, -51.00000000000000711 ) ) ;
#1546 = ORIENTED_EDGE ( 'NONE', *, *, #12281, .T. ) ;
#1547 = ORIENTED_EDGE ( 'NONE', *, *, #18203, .T. ) ;
#1548 = CARTESIAN_POINT ( 'NONE',  ( 104.3262379212492448, 104.0454443415356991, -49.79999999453762882 ) ) ;
#1549 = CARTESIAN_POINT ( 'NONE',  ( 9.598844408820456309, 39.11484374999999858, -9.598844408820458085 ) ) ;
#1550 = CARTESIAN_POINT ( 'NONE',  ( 13.14518615778179544, 33.80664062608393294, -1.609821015232357215E-15 ) ) ;
#1551 = CARTESIAN_POINT ( 'NONE',  ( -5.622872871577873077, 32.21914062716787441, -13.57481594606304753 ) ) ;
#1552 = CARTESIAN_POINT ( 'NONE',  ( 102.0710678118654329, 5.000000000000018652, 2.812500002731185944 ) ) ;
#1553 = CARTESIAN_POINT ( 'NONE',  ( 103.1528011352953342, 84.06250000136560629, 3.152801135295355106 ) ) ;
#1554 = CARTESIAN_POINT ( 'NONE',  ( 65.00000000000000000, 38.96601562608393721, -13.14518615778179544 ) ) ;
#1555 = CARTESIAN_POINT ( 'NONE',  ( 95.00472066334982912, 103.1245878333314323, -51.07500000273118701 ) ) ;
#1556 = CARTESIAN_POINT ( 'NONE',  ( 102.0710678118655039, 93.81250000000000000, 4.999999999999940492 ) ) ;
#1557 = CARTESIAN_POINT ( 'NONE',  ( 99.99999999999998579, 124.5500000010924708, -2.066987299999998751 ) ) ;
#1558 = DIRECTION ( 'NONE',  ( 0.000000000000000000, 0.000000000000000000, 1.000000000000000000 ) ) ;
#1559 = CARTESIAN_POINT ( 'NONE',  ( 107.0000000000000000, 107.7255621263696668, -49.59999999453764019 ) ) ;
#1560 = CARTESIAN_POINT ( 'NONE',  ( 139.5988444088204403, 39.90859374999999432, -9.598844408820458085 ) ) ;
#1561 = ADVANCED_FACE ( 'NONE', ( #20006 ), #6356, .F. ) ;
#1562 = ORIENTED_EDGE ( 'NONE', *, *, #19274, .F. ) ;
#1563 = CARTESIAN_POINT ( 'NONE',  ( 93.00000000000001421, 107.7255621263696241, -52.39999999453765156 ) ) ;
#1564 = CARTESIAN_POINT ( 'NONE',  ( 9.295050272127046043, 39.66054687608393436, -9.295050272127046043 ) ) ;
#1565 = CARTESIAN_POINT ( 'NONE',  ( 101.8468681455906903, 80.75000000136560629, 4.458734124999987891 ) ) ;
#1566 = CARTESIAN_POINT ( 'NONE',  ( 135.4449143864723055, 38.42031250108393436, 13.14518615778179189 ) ) ;
#1567 = CARTESIAN_POINT ( 'NONE',  ( 51.42518405393695957, 35.54296875216788010, 0.000000000000000000 ) ) ;
#1568 = CARTESIAN_POINT ( 'NONE',  ( 106.5389055433250860, 105.2492070361643215, -54.82499999726882578 ) ) ;
#1569 = CARTESIAN_POINT ( 'NONE',  ( -13.57481594606304576, 37.18007812716787441, 5.622872871577880183 ) ) ;
#1570 = ORIENTED_EDGE ( 'NONE', *, *, #18211, .T. ) ;
#1571 = CARTESIAN_POINT ( 'NONE',  ( 104.9999999999999574, 2.071067811865491937, 9.562499999999998224 ) ) ;
#1572 = LINE ( 'NONE', #17352, #10785 ) ;
#1573 = CARTESIAN_POINT ( 'NONE',  ( 2.414731522848535132E-15, 33.01289062608393721, 13.14518615778179544 ) ) ;
#1574 = CARTESIAN_POINT ( 'NONE',  ( 200.4449143864723055, 37.62656250108393863, 13.14518615778179189 ) ) ;
#1575 = CARTESIAN_POINT ( 'NONE',  ( 92.99999999999998579, 110.0000000000000000, -145.0000000000000284 ) ) ;
#1576 = CARTESIAN_POINT ( 'NONE',  ( 143.1451861577818363, 37.72578125108393010, 5.444914386472293977 ) ) ;
#1577 = CARTESIAN_POINT ( 'NONE',  ( 98.23223304703363112, 123.6000000021849416, 1.767766952966351557 ) ) ;
#1578 = CARTESIAN_POINT ( 'NONE',  ( 94.99999999999995737, -2.071067811865466624, 11.06250000000000000 ) ) ;
#1579 = CARTESIAN_POINT ( 'NONE',  ( 104.4587341249999781, 93.31249999863440792, -6.938893903907228378E-15 ) ) ;
#1580 =( BOUNDED_CURVE ( )  B_SPLINE_CURVE ( 2, ( #24727, #5206, #13870, #3204, #7466, #18312, #22597, #22310, #9324 ),
 .UNSPECIFIED., .F., .T. ) 
 B_SPLINE_CURVE_WITH_KNOTS ( ( 3, 2, 2, 2, 3 ),
 ( 0.1071428571428571092, 0.1160714285714285476, 0.1249999999999999861, 0.1339285714285714246, 0.1428571428571428492 ),
 .UNSPECIFIED. ) 
 CURVE ( )  GEOMETRIC_REPRESENTATION_ITEM ( )  RATIONAL_B_SPLINE_CURVE ( ( 1.000000000000000222, 0.9238795325112865164, 1.000000000000000000, 0.9238795325112867385, 1.000000000000000000, 0.9238795325112867385, 1.000000000000000000, 0.9238795325112867385, 1.000000000000000000 ) ) 
 REPRESENTATION_ITEM ( '' )  );
#1581 = CARTESIAN_POINT ( 'NONE',  ( 55.40115559117954547, 36.93203124999999432, -9.598844408820458085 ) ) ;
#1582 = CARTESIAN_POINT ( 'NONE',  ( 99.99999999999998579, 124.3999999999999915, 2.499999999999978684 ) ) ;
#1583 = CARTESIAN_POINT ( 'NONE',  ( 195.0000000000000000, 38.02343749999999289, 13.57481594606304576 ) ) ;
#1584 = CARTESIAN_POINT ( 'NONE',  ( 130.7050241099688606, 36.00000000000000711, 13.13343125082108465 ) ) ;
#1585 = CARTESIAN_POINT ( 'NONE',  ( 99.99999999999995737, -4.458734124999988779, 2.937500001365592528 ) ) ;
#1586 = CARTESIAN_POINT ( 'NONE',  ( 70.44491438647230552, 37.62656250108393863, 13.14518615778179189 ) ) ;
#1587 = CARTESIAN_POINT ( 'NONE',  ( 95.54126587499996504, 1.387778780781445676E-14, 4.437500001365592084 ) ) ;
#1588 = CARTESIAN_POINT ( 'NONE',  ( 102.1631189606246295, 103.3426043859339103, -51.90000000546238113 ) ) ;
#1589 = CARTESIAN_POINT ( 'NONE',  ( 104.4587341249999781, 94.56249999863440792, -6.938893903907228378E-15 ) ) ;
#1590 = CARTESIAN_POINT ( 'NONE',  ( 99.99999999999998579, 130.0000000000000000, -5.204170427930421283E-15 ) ) ;
#1591 = CARTESIAN_POINT ( 'NONE',  ( -10.78684676818415689, 36.00000000000000000, 7.561388982944556858 ) ) ;
#1592 = CARTESIAN_POINT ( 'NONE',  ( 9.598844408820456309, 38.32109374999999574, -9.598844408820458085 ) ) ;
#1593 = ORIENTED_EDGE ( 'NONE', *, *, #14238, .T. ) ;
#1594 = CARTESIAN_POINT ( 'NONE',  ( 99.99999999999995737, 83.93750000136560629, 4.458734124999988779 ) ) ;
#1595 = CARTESIAN_POINT ( 'NONE',  ( 101.8468681455907330, 91.12499999863439371, 4.458734124999979898 ) ) ;
#1596 = VERTEX_POINT ( 'NONE', #7017 ) ;
#1597 = ORIENTED_EDGE ( 'NONE', *, *, #44, .F. ) ;
#1598 = CARTESIAN_POINT ( 'NONE',  ( 133.1165920804657787, 53.90895096933309105, -15.00000000000000178 ) ) ;
#1599 = CARTESIAN_POINT ( 'NONE',  ( 104.4587341249999639, 1.442382525525748735E-14, 8.187500001365592084 ) ) ;
#1600 = ADVANCED_FACE ( 'NONE', ( #7157 ), #15853, .T. ) ;
#1601 = ORIENTED_EDGE ( 'NONE', *, *, #2716, .F. ) ;
#1602 = CARTESIAN_POINT ( 'NONE',  ( 106.5389055433251002, 114.7507929638356785, -46.17500000273119554 ) ) ;
#1603 = CARTESIAN_POINT ( 'NONE',  ( -13.14518615778179189, 34.25312500108393010, 5.444914386472304635 ) ) ;
#1604 = CARTESIAN_POINT ( 'NONE',  ( 181.4251840539369596, 39.51171875216787299, 0.000000000000000000 ) ) ;
#1605 = CARTESIAN_POINT ( 'NONE',  ( 9.295050272127046043, 37.87460937608393152, -9.295050272127046043 ) ) ;
#1606 = CARTESIAN_POINT ( 'NONE',  ( 99.99999999999998579, 101.5015231886685712, -48.62500000273119838 ) ) ;
#1607 = CARTESIAN_POINT ( 'NONE',  ( 2.414731522848535132E-15, 32.02070312608393010, 13.14518615778179544 ) ) ;
#1608 = CIRCLE ( 'NONE', #13387, 4.999999999999989342 ) ;
#1609 = ORIENTED_EDGE ( 'NONE', *, *, #12107, .F. ) ;
#1610 = CARTESIAN_POINT ( 'NONE',  ( 59.37712712842213136, 36.38632812499999858, 13.57481594606304753 ) ) ;
#1611 = FACE_OUTER_BOUND ( 'NONE', #17106, .T. ) ;
#1612 = CARTESIAN_POINT ( 'NONE',  ( 202.7541239759955829, 36.00000000000001421, 10.77549638133708676 ) ) ;
#1613 = CARTESIAN_POINT ( 'NONE',  ( 95.54126587499995082, -1.846868145590724986, 5.500000001365591196 ) ) ;
#1614 = CARTESIAN_POINT ( 'NONE',  ( 9.295050272127046043, 34.10429687608393579, -9.295050272127046043 ) ) ;
#1615 = CARTESIAN_POINT ( 'NONE',  ( 98.15313185440923860, 4.458734125000016313, 2.500000001365592084 ) ) ;
#1616 = CARTESIAN_POINT ( 'NONE',  ( 99.99999999999995737, 83.93750000136560629, 4.458734124999988779 ) ) ;
#1617 = CARTESIAN_POINT ( 'NONE',  ( 9.295050272127046043, 32.31835937608393294, -9.295050272127046043 ) ) ;
#1618 = CARTESIAN_POINT ( 'NONE',  ( -5.444914386472297529, 39.01562500108394005, -13.14518615778179900 ) ) ;
#1619 = DIRECTION ( 'NONE',  ( 1.000000000000000000, -0.000000000000000000, -5.782411586589357392E-17 ) ) ;
#1620 = ORIENTED_EDGE ( 'NONE', *, *, #6276, .F. ) ;
#1621 = CARTESIAN_POINT ( 'NONE',  ( 13.14518615778179544, 32.41757812608393863, -1.609821015232357215E-15 ) ) ;
#1622 = CARTESIAN_POINT ( 'NONE',  ( 101.4615807364564546, 124.2500000010924879, -1.461580736456474794 ) ) ;
#1623 = CYLINDRICAL_SURFACE ( 'NONE', #4366, 13.57481594606304398 ) ;
#1624 = DIRECTION ( 'NONE',  ( -0.000000000000000000, -0.000000000000000000, -1.000000000000000000 ) ) ;
#1625 = CARTESIAN_POINT ( 'NONE',  ( 102.0541222904681575, 123.0000000000000142, -1.218761725175215416 ) ) ;
#1626 = AXIS2_PLACEMENT_3D ( 'NONE', #4454, #2324, #10980 ) ;
#1627 = CARTESIAN_POINT ( 'NONE',  ( -5.622872871577965448, 32.41757812499999858, 13.57481594606295161 ) ) ;
#1628 = ORIENTED_EDGE ( 'NONE', *, *, #5003, .T. ) ;
#1629 = CARTESIAN_POINT ( 'NONE',  ( 78.14518615778180788, 39.51171875108393294, 5.444914386472293977 ) ) ;
#1630 = DIRECTION ( 'NONE',  ( 0.000000000000000000, 0.000000000000000000, 1.000000000000000000 ) ) ;
#1631 = CARTESIAN_POINT ( 'NONE',  ( 72.62394196192546758, 55.00000000000000000, -14.99999999999999822 ) ) ;
#1632 = ORIENTED_EDGE ( 'NONE', *, *, #20818, .T. ) ;
#1633 = CARTESIAN_POINT ( 'NONE',  ( -6.873508243570724652, 51.14166184781385027, -15.00000000000000000 ) ) ;
#1634 = VECTOR ( 'NONE', #11959, 1000.000000000000114 ) ;
#1635 = CIRCLE ( 'NONE', #17545, 11.57481594606304398 ) ;
#1636 = CARTESIAN_POINT ( 'NONE',  ( 198.7974518689581203, 54.08938259242987101, 14.99999999999995204 ) ) ;
#1637 = CARTESIAN_POINT ( 'NONE',  ( 120.4011555911795455, 33.06250000216787299, -9.598844408820458085 ) ) ;
#1638 = EDGE_CURVE ( 'NONE', #13131, #13869, #14467, .T. ) ;
#1639 = CARTESIAN_POINT ( 'NONE',  ( 59.55508561352770158, 40.60312500108393863, -13.14518615778179900 ) ) ;
#1640 = CARTESIAN_POINT ( 'NONE',  ( 9.598844408820459861, 31.87187500216787228, 9.598844408820456309 ) ) ;
#1641 = CARTESIAN_POINT ( 'NONE',  ( 181.8548138422181921, 37.62656250108393863, 5.444914386472304635 ) ) ;
#1642 = ORIENTED_EDGE ( 'NONE', *, *, #5660, .T. ) ;
#1643 = CARTESIAN_POINT ( 'NONE',  ( 104.9999999999999716, 1.449011120738813565E-14, 34.79898987322334136 ) ) ;
#1644 = CARTESIAN_POINT ( 'NONE',  ( 97.92893218813451028, 5.000000000000018652, 13.81250000000000000 ) ) ;
#1645 = CARTESIAN_POINT ( 'NONE',  ( 1.662435489736055498E-15, -7.395377635281828788, -13.57481594606304398 ) ) ;
#1646 = CARTESIAN_POINT ( 'NONE',  ( 143.5748159460630688, 39.90859375216787441, -1.662435489736055892E-15 ) ) ;
#1647 = DIRECTION ( 'NONE',  ( 0.000000000000000000, -1.000000000000000000, -0.000000000000000000 ) ) ;
#1648 = AXIS2_PLACEMENT_3D ( 'NONE', #12860, #351, #11008 ) ;
#1649 = CARTESIAN_POINT ( 'NONE',  ( 13.40642364673431786, 36.00000000000000000, 1.227293221036820592 ) ) ;
#1650 = CARTESIAN_POINT ( 'NONE',  ( 104.9999999999999716, 1.449011120738813565E-14, 34.79898987322334136 ) ) ;
#1651 = CARTESIAN_POINT ( 'NONE',  ( 106.5389055433250860, 114.7507929638356785, -46.42499999726882720 ) ) ;
#1652 = EDGE_LOOP ( 'NONE', ( #21390, #1458 ) ) ;
#1653 = EDGE_CURVE ( 'NONE', #19205, #1889, #9028, .T. ) ;
#1654 = CARTESIAN_POINT ( 'NONE',  ( 5.622872871577878406, 39.66054687500000142, 13.57481594606304576 ) ) ;
#1655 = CARTESIAN_POINT ( 'NONE',  ( -5.444914386472297529, 40.40468750108393436, -13.14518615778179900 ) ) ;
#1656 =( BOUNDED_CURVE ( )  B_SPLINE_CURVE ( 2, ( #6524, #26347, #15202, #4832, #23922, #4400, #13055, #13492, #1985 ),
 .UNSPECIFIED., .F., .F. ) 
 B_SPLINE_CURVE_WITH_KNOTS ( ( 3, 2, 2, 2, 3 ),
 ( 0.4375000000000003331, 0.4479166666666669627, 0.4583333333333335369, 0.4687500000000001665, 0.4791666666666667962 ),
 .UNSPECIFIED. ) 
 CURVE ( )  GEOMETRIC_REPRESENTATION_ITEM ( )  RATIONAL_B_SPLINE_CURVE ( ( 0.9999999999999975575, 0.9238795325112891810, 1.000000000000000000, 0.9238795325112867385, 1.000000000000000000, 0.9238795325112867385, 1.000000000000000000, 0.9238795325112859613, 1.000000000000000888 ) ) 
 REPRESENTATION_ITEM ( '' )  );
#1657 = CARTESIAN_POINT ( 'NONE',  ( 99.99999999999995737, 5.000000000000018652, 6.875000002731185056 ) ) ;
#1658 = CARTESIAN_POINT ( 'NONE',  ( 130.0000000000000000, 38.96601562608393721, -13.14518615778179544 ) ) ;
#1659 = CARTESIAN_POINT ( 'NONE',  ( 74.29505027212704249, 36.88242187608393152, 9.295050272127046043 ) ) ;
#1660 = CARTESIAN_POINT ( 'NONE',  ( 195.0000000000000000, 39.36289062608393152, 13.14518615778179544 ) ) ;
#1661 = ORIENTED_EDGE ( 'NONE', *, *, #20702, .T. ) ;
#1662 = DIRECTION ( 'NONE',  ( 0.000000000000000000, 1.000000000000000000, 0.000000000000000000 ) ) ;
#1663 = CARTESIAN_POINT ( 'NONE',  ( -5.444914386472297529, 34.05468750108393294, -13.14518615778179900 ) ) ;
#1664 = CARTESIAN_POINT ( 'NONE',  ( 59.37712712842208873, 36.08867187500000284, -13.57481594606300135 ) ) ;
#1665 = VECTOR ( 'NONE', #12127, 1000.000000000000000 ) ;
#1666 = ADVANCED_FACE ( 'NONE', ( #9303 ), #6880, .T. ) ;
#1667 = CARTESIAN_POINT ( 'NONE',  ( 195.0000000000000000, 36.00000000000000000, 11.57481594606302266 ) ) ;
#1668 = CARTESIAN_POINT ( 'NONE',  ( 0.000000000000000000, 50.00000000000000000, 0.000000000000000000 ) ) ;
#1669 = EDGE_CURVE ( 'NONE', #22877, #13724, #8295, .T. ) ;
#1670 = CARTESIAN_POINT ( 'NONE',  ( -8.312177448680279460E-16, 33.65781249999999147, -13.57481594606304576 ) ) ;
#1671 = CARTESIAN_POINT ( 'NONE',  ( -5.444914386472299306, 37.52734375108393294, 13.14518615778179722 ) ) ;
#1672 = CIRCLE ( 'NONE', #19864, 5.000000000000004441 ) ;
#1673 = CARTESIAN_POINT ( 'NONE',  ( 87.00000000000000000, 97.00000000000000000, 14.99999999999999467 ) ) ;
#1674 = CARTESIAN_POINT ( 'NONE',  ( 98.96446609406727646, 123.5569999999781459, 2.499999999999977796 ) ) ;
#1675 = EDGE_CURVE ( 'NONE', #8859, #12248, #1227, .T. ) ;
#1676 = CARTESIAN_POINT ( 'NONE',  ( 100.8561741729129437, 123.4000000010924509, 2.066987299999979655 ) ) ;
#1677 = CARTESIAN_POINT ( 'NONE',  ( 195.0000000000000000, 39.31328125216787583, -13.57481594606304576 ) ) ;
#1678 = CARTESIAN_POINT ( 'NONE',  ( 99.99999999999995737, -4.458734124999988779, 11.68750000136559208 ) ) ;
#1679 = CARTESIAN_POINT ( 'NONE',  ( 3.878385297391210518, 32.03609435653363136, -13.57481594606304576 ) ) ;
#1680 = ORIENTED_EDGE ( 'NONE', *, *, #8274, .T. ) ;
#1681 = CARTESIAN_POINT ( 'NONE',  ( 13.14518615778179900, 32.46718750108393436, -5.444914386472297529 ) ) ;
#1682 = CARTESIAN_POINT ( 'NONE',  ( 13.14518615778179722, 32.96328125108393436, 5.444914386472293977 ) ) ;
#1683 = EDGE_CURVE ( 'NONE', #22301, #23304, #28064, .T. ) ;
#1684 = CARTESIAN_POINT ( 'NONE',  ( -13.57481594606304576, 32.36796875216787583, 0.000000000000000000 ) ) ;
#1685 = DIRECTION ( 'NONE',  ( 0.000000000000000000, 0.000000000000000000, 1.000000000000000000 ) ) ;
#1686 = CARTESIAN_POINT ( 'NONE',  ( 95.54126587499995082, 81.50000000136560629, 1.846868145590724986 ) ) ;
#1687 = CARTESIAN_POINT ( 'NONE',  ( 59.55508561352770158, 39.01562500108394005, -13.14518615778179900 ) ) ;
#1688 = CARTESIAN_POINT ( 'NONE',  ( 106.5389055433251002, 114.7507929638356785, -48.17500000273120264 ) ) ;
#1689 = DIRECTION ( 'NONE',  ( 5.782411586589358625E-17, -0.000000000000000000, 1.000000000000000000 ) ) ;
#1690 = APPLICATION_CONTEXT ( 'automotive_design' ) ;
#1691 = CIRCLE ( 'NONE', #24441, 7.000000000000006217 ) ;
#1692 = CARTESIAN_POINT ( 'NONE',  ( 97.93301270000000613, 123.9500000010924765, -9.540979117872439019E-15 ) ) ;
#1693 = CARTESIAN_POINT ( 'NONE',  ( 65.00000000000000000, -7.395377635281828788, 13.57481594606303688 ) ) ;
#1694 = CARTESIAN_POINT ( 'NONE',  ( 107.0000000000000000, 110.0000000000000000, -53.49999999453763877 ) ) ;
#1695 = CARTESIAN_POINT ( 'NONE',  ( 116.8548138422182063, 32.86406250108393579, 5.444914386472304635 ) ) ;
#1696 = VERTEX_POINT ( 'NONE', #3462 ) ;
#1697 = CARTESIAN_POINT ( 'NONE',  ( -5.317351577475888824, 54.47013368152369850, -14.99999999999999822 ) ) ;
#1698 = CARTESIAN_POINT ( 'NONE',  ( 13.14518615778179900, 40.40468750108393436, -5.444914386472297529 ) ) ;
#1699 = CARTESIAN_POINT ( 'NONE',  ( 98.15313185440925281, 80.62500000136559208, 4.458734124999987891 ) ) ;
#1700 = CARTESIAN_POINT ( 'NONE',  ( 102.0710678118654613, 94.81249999999998579, 4.999999999999983125 ) ) ;
#1701 = CARTESIAN_POINT ( 'NONE',  ( 55.40115559117954547, 37.03125000216787299, -9.598844408820458085 ) ) ;
#1702 = CARTESIAN_POINT ( 'NONE',  ( 106.5389055433250860, 114.7507929638356785, -50.42499999726882010 ) ) ;
#1703 = CARTESIAN_POINT ( 'NONE',  ( 2.493653234604083739E-15, 34.94765625216787441, 13.57481594606304576 ) ) ;
#1704 = ORIENTED_EDGE ( 'NONE', *, *, #25691, .F. ) ;
#1705 = EDGE_CURVE ( 'NONE', #14872, #27029, #26233, .T. ) ;
#1706 = CARTESIAN_POINT ( 'NONE',  ( 104.9999999999999574, 2.071067811865491937, 10.56249999999999822 ) ) ;
#1707 = CARTESIAN_POINT ( 'NONE',  ( 103.5355339059327093, 3.535533905932755072, 1.624999999999999778 ) ) ;
#1708 =( BOUNDED_CURVE ( )  B_SPLINE_CURVE ( 2, ( #10650, #19637, #12913, #120, #4534, #13197, #2408, #11068, #8945 ),
 .UNSPECIFIED., .F., .F. ) 
 B_SPLINE_CURVE_WITH_KNOTS ( ( 3, 2, 2, 2, 3 ),
 ( 0.5500000000000004885, 0.5750000000000003997, 0.6000000000000005329, 0.6250000000000005551, 0.6500000000000005773 ),
 .UNSPECIFIED. ) 
 CURVE ( )  GEOMETRIC_REPRESENTATION_ITEM ( )  RATIONAL_B_SPLINE_CURVE ( ( 0.9999999999999986677, 0.9238795325112880708, 1.000000000000000000, 0.9238795325112867385, 1.000000000000000000, 0.9238795325112867385, 1.000000000000000000, 0.9238795325112850731, 1.000000000000001776 ) ) 
 REPRESENTATION_ITEM ( '' )  );
#1709 = CARTESIAN_POINT ( 'NONE',  ( 204.2950502721270425, 37.67617187608393436, 9.295050272127046043 ) ) ;
#1710 = EDGE_CURVE ( 'NONE', #11248, #1428, #16566, .T. ) ;
#1711 = CARTESIAN_POINT ( 'NONE',  ( 120.7049497278729575, 36.68398437608392726, 9.295050272127047819 ) ) ;
#1712 = CARTESIAN_POINT ( 'NONE',  ( 185.4011555911795313, 37.82500000216787583, -9.598844408820458085 ) ) ;
#1713 = DIRECTION ( 'NONE',  ( 0.000000000000000000, 0.000000000000000000, -1.000000000000000000 ) ) ;
#1714 = CARTESIAN_POINT ( 'NONE',  ( 99.99999999999998579, 93.56249999863440792, -4.458734124999994997 ) ) ;
#1715 = DIRECTION ( 'NONE',  ( 0.000000000000000000, 0.000000000000000000, -1.000000000000000000 ) ) ;
#1716 = CARTESIAN_POINT ( 'NONE',  ( -5.444914386472299306, 39.11484375108394573, 13.14518615778179722 ) ) ;
#1717 = CARTESIAN_POINT ( 'NONE',  ( 189.3771271284221314, 37.67617187499999432, -13.57481594606304753 ) ) ;
#1718 = CARTESIAN_POINT ( 'NONE',  ( 94.99999999999995737, -2.071067811865466624, 8.187500002731185944 ) ) ;
#1719 = CARTESIAN_POINT ( 'NONE',  ( 95.54126587499995082, 1.846868145590750077, 3.625000001365592972 ) ) ;
#1720 = CARTESIAN_POINT ( 'NONE',  ( 74.29505027212704249, 38.66835937608393436, -9.295050272127046043 ) ) ;
#1721 = CARTESIAN_POINT ( 'NONE',  ( 103.1528011352953342, 3.152801135295383084, 8.062500001365592084 ) ) ;
#1722 = DIRECTION ( 'NONE',  ( 1.374060148949977908E-06, 0.9999999999986906030, 8.549343071804204525E-07 ) ) ;
#1723 = CARTESIAN_POINT ( 'NONE',  ( 96.84719886470463734, 94.18749999863440792, 3.152801135295351997 ) ) ;
#1724 = CARTESIAN_POINT ( 'NONE',  ( 124.3771271284219893, 39.56132812500000284, 13.57481594606290720 ) ) ;
#1725 = CARTESIAN_POINT ( 'NONE',  ( 9.598844408820459861, 39.71015624999999716, 9.598844408820456309 ) ) ;
#1726 = CARTESIAN_POINT ( 'NONE',  ( 93.00000000000000000, 110.0000000000000000, -46.00000000000000711 ) ) ;
#1727 = ORIENTED_EDGE ( 'NONE', *, *, #14552, .F. ) ;
#1728 = CARTESIAN_POINT ( 'NONE',  ( 98.15313185440925281, 81.50000000136560629, -4.458734125000016313 ) ) ;
#1729 = VECTOR ( 'NONE', #17391, 1000.000000000000000 ) ;
#1730 = CARTESIAN_POINT ( 'NONE',  ( 103.1528011352953484, 91.43749999863440792, -3.152801135295366208 ) ) ;
#1731 = EDGE_LOOP ( 'NONE', ( #25793, #7572, #13083, #7304 ) ) ;
#1732 = CARTESIAN_POINT ( 'NONE',  ( 107.0000000000000000, 107.7255621263696668, -46.10000000000000142 ) ) ;
#1733 = CARTESIAN_POINT ( 'NONE',  ( 70.44491438647230552, 34.94765625108394147, -13.14518615778179900 ) ) ;
#1734 = ORIENTED_EDGE ( 'NONE', *, *, #1871, .F. ) ;
#1735 = CARTESIAN_POINT ( 'NONE',  ( -9.598844408820458085, 36.93203124999999432, -9.598844408820458085 ) ) ;
#1736 = CARTESIAN_POINT ( 'NONE',  ( 95.54126587499996504, 1.387778780781445676E-14, 5.687500001365591196 ) ) ;
#1737 = ORIENTED_EDGE ( 'NONE', *, *, #3048, .T. ) ;
#1738 = DIRECTION ( 'NONE',  ( 1.000000000000000000, 0.000000000000000000, -7.228014483236696740E-18 ) ) ;
#1739 = CARTESIAN_POINT ( 'NONE',  ( -13.14518615778179900, 33.36015625108393579, -5.444914386472297529 ) ) ;
#1740 = CARTESIAN_POINT ( 'NONE',  ( 200.6228728715778686, 36.88242187716787157, -13.57481594606304753 ) ) ;
#1741 =( BOUNDED_CURVE ( )  B_SPLINE_CURVE ( 2, ( #23362, #21084, #12781, #16798, #25630, #3703, #6111, #16665, #12365, #3834, #25361 ),
 .UNSPECIFIED., .F., .F. ) 
 B_SPLINE_CURVE_WITH_KNOTS ( ( 3, 2, 2, 2, 2, 3 ),
 ( 0.2000000000000001776, 0.2200000000000001676, 0.2400000000000001854, 0.2600000000000002309, 0.2800000000000002487, 0.3000000000000002109 ),
 .UNSPECIFIED. ) 
 CURVE ( )  GEOMETRIC_REPRESENTATION_ITEM ( )  RATIONAL_B_SPLINE_CURVE ( ( 0.9999999999999995559, 0.9510565162951539753, 1.000000000000000000, 0.9510565162951535312, 1.000000000000000000, 0.9510565162951535312, 1.000000000000000000, 0.9510565162951535312, 1.000000000000000000, 0.9510565162951529761, 1.000000000000000444 ) ) 
 REPRESENTATION_ITEM ( '' )  );
#1742 = CARTESIAN_POINT ( 'NONE',  ( -5.444914386472297529, 38.81718750108393579, -13.14518615778179722 ) ) ;
#1743 = FACE_OUTER_BOUND ( 'NONE', #8237, .T. ) ;
#1744 = CARTESIAN_POINT ( 'NONE',  ( 201.4128666762415492, 50.00000000108515508, 11.99502265408284707 ) ) ;
#1745 = CARTESIAN_POINT ( 'NONE',  ( 120.7049497278729575, 40.05742187608393579, 9.295050272127047819 ) ) ;
#1746 = CARTESIAN_POINT ( 'NONE',  ( -5.444914386472299306, 38.51953125108393294, 13.14518615778179722 ) ) ;
#1747 = ORIENTED_EDGE ( 'NONE', *, *, #23271, .F. ) ;
#1748 = CARTESIAN_POINT ( 'NONE',  ( 51.42518405393695957, 37.08085937499999574, 5.622872871577880183 ) ) ;
#1749 = DIRECTION ( 'NONE',  ( -0.000000000000000000, -0.000000000000000000, -1.000000000000000000 ) ) ;
#1750 = VECTOR ( 'NONE', #2106, 1000.000000000000000 ) ;
#1751 = CARTESIAN_POINT ( 'NONE',  ( 102.1631189606246295, 116.6573956140660897, -46.60000000000000142 ) ) ;
#1752 = CARTESIAN_POINT ( 'NONE',  ( 104.4587341249999781, 1.846868145590750299, 6.000000001365591196 ) ) ;
#1753 = CARTESIAN_POINT ( 'NONE',  ( 13.14518615778179544, 32.41757812608393863, -1.609821015232357215E-15 ) ) ;
#1754 = CARTESIAN_POINT ( 'NONE',  ( 98.15313185440923860, 4.458734125000016313, 4.500000001365592084 ) ) ;
#1755 = CARTESIAN_POINT ( 'NONE',  ( 104.4587341249999781, 84.25000000136559208, -1.846868145590750521 ) ) ;
#1756 = CARTESIAN_POINT ( 'NONE',  ( -13.14518615778179900, 34.15390625108393863, -5.444914386472297529 ) ) ;
#1757 = CARTESIAN_POINT ( 'NONE',  ( 13.14518615778179900, 38.81718750108393579, -5.444914386472297529 ) ) ;
#1758 = CARTESIAN_POINT ( 'NONE',  ( 185.4011555911795597, 38.71796874999999716, 9.598844408820459861 ) ) ;
#1759 = ORIENTED_EDGE ( 'NONE', *, *, #25499, .F. ) ;
#1760 = LINE ( 'NONE', #12550, #16351 ) ;
#1761 = CARTESIAN_POINT ( 'NONE',  ( 1.417506129906585004E-15, -7.395377635281828788, -11.57481594606304398 ) ) ;
#1762 = CARTESIAN_POINT ( 'NONE',  ( 104.4587341249999923, 94.49999999863439371, 1.846868145590726318 ) ) ;
#1763 = CARTESIAN_POINT ( 'NONE',  ( 5.622872871578054266, 32.11992187716787583, -13.57481594606286635 ) ) ;
#1764 = CARTESIAN_POINT ( 'NONE',  ( 93.46109445667489979, 105.2492070361643215, -55.67499999726882720 ) ) ;
#1765 = CARTESIAN_POINT ( 'NONE',  ( 87.00000000000000000, 125.0000000000000000, -13.00000000000000888 ) ) ;
#1766 = ORIENTED_EDGE ( 'NONE', *, *, #21989, .F. ) ;
#1767 = CARTESIAN_POINT ( 'NONE',  ( 78.14518615778180788, 38.81718750108393579, -5.444914386472297529 ) ) ;
#1768 = DIRECTION ( 'NONE',  ( 1.000000000000000000, 0.000000000000000000, -0.000000000000000000 ) ) ;
#1769 = AXIS2_PLACEMENT_3D ( 'NONE', #11651, #14079, #22799 ) ;
#1770 = VECTOR ( 'NONE', #15736, 1000.000000000000227 ) ;
#1771 = CARTESIAN_POINT ( 'NONE',  ( 181.8548138422181921, 31.97109375108393436, -5.444914386472297529 ) ) ;
#1772 = ORIENTED_EDGE ( 'NONE', *, *, #956, .T. ) ;
#1773 = CARTESIAN_POINT ( 'NONE',  ( 74.59884440882045453, 37.32890624999999574, 9.598844408820456309 ) ) ;
#1774 = CARTESIAN_POINT ( 'NONE',  ( 104.9999999999999716, 1.449011120738813565E-14, 3.499999999999999556 ) ) ;
#1775 = CIRCLE ( 'NONE', #2235, 2.999999999999989786 ) ;
#1776 = CARTESIAN_POINT ( 'NONE',  ( 96.46446609406721961, 81.25000000273119838, 3.535533905932727539 ) ) ;
#1777 = CARTESIAN_POINT ( 'NONE',  ( 139.5988444088204687, 34.25312500216787015, 9.598844408820456309 ) ) ;
#1778 = CARTESIAN_POINT ( 'NONE',  ( 55.70494972787295751, 40.65273437608393436, -9.295050272127046043 ) ) ;
#1779 = CARTESIAN_POINT ( 'NONE',  ( 104.3262379212492448, 115.9545556584642867, -47.19999999453763451 ) ) ;
#1780 = CARTESIAN_POINT ( 'NONE',  ( 204.2950502721270425, 37.27929687608394005, -9.295050272127046043 ) ) ;
#1781 = VERTEX_POINT ( 'NONE', #8007 ) ;
#1782 = ORIENTED_EDGE ( 'NONE', *, *, #17385, .T. ) ;
#1783 = CARTESIAN_POINT ( 'NONE',  ( -8.049105076161786076E-16, 33.21132812608393436, -13.14518615778179544 ) ) ;
#1784 = CARTESIAN_POINT ( 'NONE',  ( 99.99999999999998579, 128.0000000000000000, -5.204170427930421283E-15 ) ) ;
#1785 = CARTESIAN_POINT ( 'NONE',  ( 2.493653234604083739E-15, 38.02343749999999289, 13.57481594606304576 ) ) ;
#1786 = CARTESIAN_POINT ( 'NONE',  ( 101.8468681455907046, 84.12500000136560629, -4.458734125000016313 ) ) ;
#1787 = DIRECTION ( 'NONE',  ( -1.000000000000000000, 0.000000000000000000, 2.385244779468110248E-16 ) ) ;
#1788 = EDGE_CURVE ( 'NONE', #12549, #24077, #12551, .T. ) ;
#1789 = CARTESIAN_POINT ( 'NONE',  ( 102.4999999999999858, 123.0500000000000114, -1.035533905932742638 ) ) ;
#1790 = VECTOR ( 'NONE', #15167, 1000.000000000000000 ) ;
#1791 = CARTESIAN_POINT ( 'NONE',  ( 94.99999999999997158, -2.071067811865486608, 6.062500000000000000 ) ) ;
#1792 = COLOUR_RGB ( '', 0.09019608, 0.27058824, 0.51372549) ;
#1793 = CARTESIAN_POINT ( 'NONE',  ( 97.92893218813452449, 82.81250000000001421, -5.000000000000043521 ) ) ;
#1794 = CARTESIAN_POINT ( 'NONE',  ( 116.4251840539369454, 32.21914062500000142, -5.622872871577873077 ) ) ;
#1795 = ORIENTED_EDGE ( 'NONE', *, *, #9386, .F. ) ;
#1796 = CARTESIAN_POINT ( 'NONE',  ( -13.57481594606304753, 40.95039062499999005, -5.622872871577873077 ) ) ;
#1797 = CARTESIAN_POINT ( 'NONE',  ( 5.444914386472302859, 39.21406250108392300, 13.14518615778179189 ) ) ;
#1798 = CARTESIAN_POINT ( 'NONE',  ( 99.99999999999995737, 5.000000000000018652, 1.875000002731185056 ) ) ;
#1799 = CARTESIAN_POINT ( 'NONE',  ( 139.2950502721270425, 36.48554687608393721, -9.295050272127046043 ) ) ;
#1800 = CARTESIAN_POINT ( 'NONE',  ( 70.44491438647230552, 36.83281250108392868, 13.14518615778179189 ) ) ;
#1801 = CARTESIAN_POINT ( 'NONE',  ( 181.8548138422181921, 39.11484375108394573, -5.444914386472297529 ) ) ;
#1802 = FACE_OUTER_BOUND ( 'NONE', #21363, .T. ) ;
#1803 = CARTESIAN_POINT ( 'NONE',  ( 5.444914386472302859, 36.03906250108394005, 13.14518615778179189 ) ) ;
#1804 = FACE_OUTER_BOUND ( 'NONE', #3387, .T. ) ;
#1805 = CARTESIAN_POINT ( 'NONE',  ( 99.99999999999998579, 90.00000000000000000, -6.938893903907228378E-15 ) ) ;
#1806 = CARTESIAN_POINT ( 'NONE',  ( 99.99999999999995737, 82.25000000000000000, 4.999999999999990230 ) ) ;
#1807 = ORIENTED_EDGE ( 'NONE', *, *, #16489, .F. ) ;
#1808 = CARTESIAN_POINT ( 'NONE',  ( -5.444914386472299306, 39.11484375108394573, 13.14518615778179722 ) ) ;
#1809 = CARTESIAN_POINT ( 'NONE',  ( -5.622872871577873966, 34.79882812499999289, 13.57481594606304753 ) ) ;
#1810 = CARTESIAN_POINT ( 'NONE',  ( 97.50000000000000000, 124.2000000000000028, -9.540979117872439019E-15 ) ) ;
#1811 = CONICAL_SURFACE ( 'NONE', #27315, 17.49444650053485972, 0.5235987755983000369 ) ;
#1812 = CARTESIAN_POINT ( 'NONE',  ( 102.0669872999999797, 122.7500000010924737, -9.794112055954760458E-15 ) ) ;
#1813 = CARTESIAN_POINT ( 'NONE',  ( 99.14382582708708469, 123.3000000010924708, 2.066987299999979655 ) ) ;
#1814 = EDGE_CURVE ( 'NONE', #4816, #9474, #1416, .T. ) ;
#1815 = CARTESIAN_POINT ( 'NONE',  ( 104.4587341249999639, 1.442382525525748735E-14, 10.93750000136559208 ) ) ;
#1816 = ORIENTED_EDGE ( 'NONE', *, *, #14513, .T. ) ;
#1817 = DIRECTION ( 'NONE',  ( 0.000000000000000000, 0.000000000000000000, 1.000000000000000000 ) ) ;
#1818 = CARTESIAN_POINT ( 'NONE',  ( -13.57481594606304753, 40.15664062500000142, -5.622872871577873077 ) ) ;
#1819 = CARTESIAN_POINT ( 'NONE',  ( -13.14518615778179189, 31.87187500108393223, 5.444914386472304635 ) ) ;
#1820 = AXIS2_PLACEMENT_3D ( 'NONE', #15006, #28143, #23728 ) ;
#1821 = CARTESIAN_POINT ( 'NONE',  ( -5.622872871577873077, 32.51679687716787726, 13.57481594606304753 ) ) ;
#1822 = CARTESIAN_POINT ( 'NONE',  ( 65.00000000000000000, 37.72578125216787726, -13.57481594606304576 ) ) ;
#1823 = CARTESIAN_POINT ( 'NONE',  ( 95.54126587499996504, 84.68750000136560629, -1.387778780781445676E-14 ) ) ;
#1824 = CARTESIAN_POINT ( 'NONE',  ( 55.70494972787295751, 39.85898437608393152, -9.295050272127046043 ) ) ;
#1825 = CARTESIAN_POINT ( 'NONE',  ( 91.91746824999998466, 107.3738262389971538, -47.27500000273118275 ) ) ;
#1826 = CARTESIAN_POINT ( 'NONE',  ( 13.14518615778179722, 40.10703125108393152, 5.444914386472293977 ) ) ;
#1827 =( BOUNDED_CURVE ( )  B_SPLINE_CURVE ( 2, ( #15862, #22440, #22726, #22583, #26575, #3052, #24425, #24284, #5053 ),
 .UNSPECIFIED., .F., .T. ) 
 B_SPLINE_CURVE_WITH_KNOTS ( ( 3, 2, 2, 2, 3 ),
 ( 0.6874999999999997780, 0.6979166666666665186, 0.7083333333333333703, 0.7187500000000001110, 0.7291666666666668517 ),
 .UNSPECIFIED. ) 
 CURVE ( )  GEOMETRIC_REPRESENTATION_ITEM ( )  RATIONAL_B_SPLINE_CURVE ( ( 1.000000000000001554, 0.9238795325112850731, 1.000000000000000000, 0.9238795325112867385, 1.000000000000000000, 0.9238795325112867385, 1.000000000000000000, 0.9238795325112850731, 1.000000000000001554 ) ) 
 REPRESENTATION_ITEM ( '' )  );
#1828 = ORIENTED_EDGE ( 'NONE', *, *, #13179, .F. ) ;
#1829 = EDGE_CURVE ( 'NONE', #20267, #3776, #7205, .T. ) ;
#1830 = CARTESIAN_POINT ( 'NONE',  ( 97.93301269999999192, 122.9000000010924936, -0.8561741729129505041 ) ) ;
#1831 = CARTESIAN_POINT ( 'NONE',  ( 143.5748159460630688, 39.01562500000000000, -1.662435489736055892E-15 ) ) ;
#1832 = CARTESIAN_POINT ( 'NONE',  ( 95.67376207875069838, 115.9545556584642867, -54.79999999453764303 ) ) ;
#1833 = CARTESIAN_POINT ( 'NONE',  ( 120.4011555911795455, 40.30546874999999574, 9.598844408820459861 ) ) ;
#1834 = ORIENTED_EDGE ( 'NONE', *, *, #7584, .T. ) ;
#1835 = CARTESIAN_POINT ( 'NONE',  ( -0.3247243111960383954, 53.49346745874647979, -15.00000000000000533 ) ) ;
#1836 = EDGE_CURVE ( 'NONE', #22508, #6997, #16140, .T. ) ;
#1837 = DIRECTION ( 'NONE',  ( 0.000000000000000000, -1.000000000000000000, 0.000000000000000000 ) ) ;
#1838 = CARTESIAN_POINT ( 'NONE',  ( -9.598844408820458085, 40.20625000216787726, -9.598844408820458085 ) ) ;
#1839 = CARTESIAN_POINT ( 'NONE',  ( 116.8548138422182063, 39.71015625108393010, -5.444914386472297529 ) ) ;
#1840 = CARTESIAN_POINT ( 'NONE',  ( 51.42518405393695957, 37.97382812716787726, 5.622872871577880183 ) ) ;
#1841 = CONICAL_SURFACE ( 'NONE', #10015, 19.22649730810373470, 0.5235987755983000369 ) ;
#1842 = CARTESIAN_POINT ( 'NONE',  ( 104.9952793366501709, 103.1245878333314323, -54.92499999726882720 ) ) ;
#1843 = CARTESIAN_POINT ( 'NONE',  ( 13.57481594606304931, 35.09648437716787583, 5.622872871577869525 ) ) ;
#1844 = ORIENTED_EDGE ( 'NONE', *, *, #3092, .T. ) ;
#1845 = CARTESIAN_POINT ( 'NONE',  ( 99.99999999999995737, 5.000000000000018652, 5.750000000000000000 ) ) ;
#1846 = ADVANCED_FACE ( 'NONE', ( #10130 ), #18842, .F. ) ;
#1847 = CARTESIAN_POINT ( 'NONE',  ( 99.99999999999998579, 117.3602355696678643, -47.00000000546238255 ) ) ;
#1848 = CARTESIAN_POINT ( 'NONE',  ( 208.1451861577818079, 37.77539062608393294, -1.609821015232357215E-15 ) ) ;
#1849 = CARTESIAN_POINT ( 'NONE',  ( 107.0000000000000000, 110.0000000000000000, -52.00000000000001421 ) ) ;
#1850 = CARTESIAN_POINT ( 'NONE',  ( 120.7049497278729575, 37.27929687608393294, -9.295050272127046043 ) ) ;
#1851 = CARTESIAN_POINT ( 'NONE',  ( 13.57481594606304753, 35.89023437499999858, -5.622872871577873966 ) ) ;
#1852 = CARTESIAN_POINT ( 'NONE',  ( 94.99999999999995737, 1.387778780781445676E-14, 6.999999999999999112 ) ) ;
#1853 = CARTESIAN_POINT ( 'NONE',  ( 98.15313185440923860, 92.99999999863439371, 4.458734124999980786 ) ) ;
#1854 = CARTESIAN_POINT ( 'NONE',  ( -5.444914386472297529, 38.02343750108394005, -13.14518615778179900 ) ) ;
#1855 = CARTESIAN_POINT ( 'NONE',  ( 181.4251840539369596, 36.23749999999999005, 0.000000000000000000 ) ) ;
#1856 = EDGE_CURVE ( 'NONE', #24599, #1420, #20434, .T. ) ;
#1857 = PRODUCT_CONTEXT ( 'NONE', #6415, 'mechanical' ) ;
#1858 = CARTESIAN_POINT ( 'NONE',  ( 96.46446609406721961, -3.535533905932727539, 8.250000002731185944 ) ) ;
#1859 = CARTESIAN_POINT ( 'NONE',  ( 104.4587341249999781, -1.846868145590721655, 3.125000001365592528 ) ) ;
#1860 = CARTESIAN_POINT ( 'NONE',  ( 51.85481384221819923, 38.12265625108393152, -5.444914386472297529 ) ) ;
#1861 = CARTESIAN_POINT ( 'NONE',  ( 104.4587341249999639, 1.442382525525748735E-14, 6.937500001365592972 ) ) ;
#1862 = CARTESIAN_POINT ( 'NONE',  ( 99.99999999999998579, 117.3602355696678501, -45.00000000546238255 ) ) ;
#1863 = CARTESIAN_POINT ( 'NONE',  ( 103.1528011352953484, 94.18749999863440792, 3.152801135295352886 ) ) ;
#1864 = CARTESIAN_POINT ( 'NONE',  ( -12.37587840034922770, 35.99999999999998579, 4.513979326318623642 ) ) ;
#1865 = CARTESIAN_POINT ( 'NONE',  ( 5.622872871577878406, 38.07304687499998863, 13.57481594606304576 ) ) ;
#1866 = CARTESIAN_POINT ( 'NONE',  ( 105.6631189606246295, 105.8855032339526758, -45.20000000000000284 ) ) ;
#1867 = ORIENTED_EDGE ( 'NONE', *, *, #16501, .T. ) ;
#1868 = CARTESIAN_POINT ( 'NONE',  ( 95.54126587499996504, 83.68750000136560629, -1.387778780781445676E-14 ) ) ;
#1869 = DIRECTION ( 'NONE',  ( -0.000000000000000000, -1.000000000000000000, -0.000000000000000000 ) ) ;
#1870 = ORIENTED_EDGE ( 'NONE', *, *, #22385, .F. ) ;
#1871 = EDGE_CURVE ( 'NONE', #9928, #16597, #27628, .T. ) ;
#1872 =( BOUNDED_CURVE ( )  B_SPLINE_CURVE ( 2, ( #24453, #20324, #14172, #14029, #9479, #27179, #22466, #4939, #7481 ),
 .UNSPECIFIED., .F., .F. ) 
 B_SPLINE_CURVE_WITH_KNOTS ( ( 3, 2, 2, 2, 3 ),
 ( 0.2708333333333330928, 0.2812499999999998890, 0.2916666666666666852, 0.3020833333333334259, 0.3125000000000002220 ),
 .UNSPECIFIED. ) 
 CURVE ( )  GEOMETRIC_REPRESENTATION_ITEM ( )  RATIONAL_B_SPLINE_CURVE ( ( 1.000000000000001554, 0.9238795325112850731, 1.000000000000000000, 0.9238795325112867385, 1.000000000000000000, 0.9238795325112867385, 1.000000000000000000, 0.9238795325112850731, 1.000000000000001554 ) ) 
 REPRESENTATION_ITEM ( '' )  );
#1873 = CARTESIAN_POINT ( 'NONE',  ( 97.83688103937537051, 103.3426043859339103, -46.60000000000000853 ) ) ;
#1874 = CARTESIAN_POINT ( 'NONE',  ( 74.29505027212704249, 34.69960937608393436, 9.295050272127046043 ) ) ;
#1875 = VERTEX_POINT ( 'NONE', #26 ) ;
#1876 = CARTESIAN_POINT ( 'NONE',  ( -13.57481594606304398, 33.21132812716787441, 5.622872871577880183 ) ) ;
#1877 = AXIS2_PLACEMENT_3D ( 'NONE', #27298, #24865, #9884 ) ;
#1878 = CARTESIAN_POINT ( 'NONE',  ( 101.8468681455906903, -4.458734124999987891, 4.000000001365592084 ) ) ;
#1879 = ORIENTED_EDGE ( 'NONE', *, *, #9511, .T. ) ;
#1880 = CARTESIAN_POINT ( 'NONE',  ( 99.99999999999995737, 82.37500000273119838, 4.999999999999990230 ) ) ;
#1881 = CARTESIAN_POINT ( 'NONE',  ( -9.295050272127046043, 34.10429687608393579, -9.295050272127046043 ) ) ;
#1882 = CARTESIAN_POINT ( 'NONE',  ( 181.4251840539369596, 36.38632812716788578, 5.622872871577880183 ) ) ;
#1883 = CARTESIAN_POINT ( 'NONE',  ( 5.444914386472302859, 39.21406250108392300, 13.14518615778179189 ) ) ;
#1884 = CARTESIAN_POINT ( 'NONE',  ( 70.62287287157801074, 36.08867187716787583, -13.57481594606290898 ) ) ;
#1885 = CARTESIAN_POINT ( 'NONE',  ( 95.67376207875072680, 104.0454443415356991, -51.70000000000001705 ) ) ;
#1886 = CARTESIAN_POINT ( 'NONE',  ( 143.1451861577818363, 40.30546875108393579, 5.444914386472293977 ) ) ;
#1887 = CARTESIAN_POINT ( 'NONE',  ( -13.14518615778179189, 37.62656250108393863, 5.444914386472304635 ) ) ;
#1888 = VECTOR ( 'NONE', #18464, 1000.000000000000000 ) ;
#1889 = VERTEX_POINT ( 'NONE', #21693 ) ;
#1890 = CARTESIAN_POINT ( 'NONE',  ( 65.00000000000000000, 38.81718749999999574, 13.57481594606304576 ) ) ;
#1891 = DIRECTION ( 'NONE',  ( 0.000000000000000000, -1.000000000000000000, 3.469446951953611231E-16 ) ) ;
#1892 = CARTESIAN_POINT ( 'NONE',  ( 103.1528011352953342, 3.152801135295383084, 13.31250000136559386 ) ) ;
#1893 = CARTESIAN_POINT ( 'NONE',  ( 104.4587341249999781, -1.846868145590721655, 2.875000001365592084 ) ) ;
#1894 = CARTESIAN_POINT ( 'NONE',  ( 108.0825317500000011, 107.3738262389971538, -50.22500000273118559 ) ) ;
#1895 = CARTESIAN_POINT ( 'NONE',  ( 95.54126587499996504, -1.846868145590724986, 4.750000001365592084 ) ) ;
#1896 = CARTESIAN_POINT ( 'NONE',  ( 95.54126587499996504, 80.62500000136559208, -1.846868145590750077 ) ) ;
#1897 = CARTESIAN_POINT ( 'NONE',  ( -8.049105076161786076E-16, 33.21132812608393436, -13.14518615778179544 ) ) ;
#1898 = CARTESIAN_POINT ( 'NONE',  ( -5.444914386472299306, 38.51953125108393294, 13.14518615778179722 ) ) ;
#1899 = EDGE_CURVE ( 'NONE', #27401, #26813, #6301, .T. ) ;
#1900 = CARTESIAN_POINT ( 'NONE',  ( 91.91746824999997045, 107.3738262389971538, -47.77499999726880731 ) ) ;
#1901 = ORIENTED_EDGE ( 'NONE', *, *, #9674, .T. ) ;
#1902 = FACE_OUTER_BOUND ( 'NONE', #14942, .T. ) ;
#1903 = CARTESIAN_POINT ( 'NONE',  ( 99.14382582708708469, 123.9000000010924794, 2.066987299999979655 ) ) ;
#1904 = CARTESIAN_POINT ( 'NONE',  ( 98.41882588794221931, 123.0000000000000284, 1.462731629774626230 ) ) ;
#1905 = CARTESIAN_POINT ( 'NONE',  ( -5.622872871577947684, 40.05742187499998863, -13.57481594606297293 ) ) ;
#1906 = CARTESIAN_POINT ( 'NONE',  ( -13.57481594606304576, 37.13046875216787868, 0.000000000000000000 ) ) ;
#1907 = CARTESIAN_POINT ( 'NONE',  ( 181.8548138422182205, 38.17226562608393436, 0.000000000000000000 ) ) ;
#1908 =( BOUNDED_CURVE ( )  B_SPLINE_CURVE ( 2, ( #9226, #22347, #21928, #19919, #17490, #13339, #403, #26188, #17781, #11486, #9086, #2404, #6798, #6519, #20202, #15340, #26629, #26484, #6654, #24055, #8661, #15484, #19774, #6939, #4677, #26049, #22066, #257, #4965, #8941, #7077, #15194, #10925, #23912, #13482, #4393, #21785, #17630, #2265, #15635, #2544, #11205, #24335, #4822, #7506, #18057, #9505, #26772, #12046, #9363, #7654, #5529, #24624, #27336, #14195, #7216, #20635, #22914, #11912, #12184, #18495, #1118, #1256, #25179, #5667, #3376, #20771, #20351, #9646, #15906, #20496, #3526, #5101, #18206, #18633, #688, #2954, #9917, #23051, #14056, #7796, #979, #13908, #7360, #16483, #14331, #5243, #9786, #26915, #5386, #27202, #836, #16346, #13765, #25045, #22636, #27056, #22488, #11627, #16053, #24763 ),
 .UNSPECIFIED., .F., .T. ) 
 B_SPLINE_CURVE_WITH_KNOTS ( ( 3, 2, 2, 2, 2, 2, 2, 2, 2, 2, 2, 2, 2, 2, 2, 2, 2, 2, 2, 2, 2, 2, 2, 2, 2, 2, 2, 2, 2, 2, 2, 2, 2, 2, 2, 2, 2, 2, 2, 2, 2, 2, 2, 2, 2, 2, 2, 2, 2, 2, 3 ),
 ( 0.000000000000000000, 0.02000000000000000042, 0.04000000000000000083, 0.05999999999999999778, 0.08000000000000000167, 0.1000000000000000056, 0.1199999999999999956, 0.1400000000000000133, 0.1600000000000000033, 0.1799999999999999933, 0.2000000000000000111, 0.2200000000000000011, 0.2399999999999999911, 0.2600000000000000089, 0.2800000000000000266, 0.2999999999999999889, 0.3200000000000000067, 0.3400000000000000244, 0.3599999999999999867, 0.3800000000000000044, 0.4000000000000000222, 0.4199999999999999845, 0.4400000000000000022, 0.4600000000000000200, 0.4799999999999999822, 0.5000000000000000000, 0.5200000000000000178, 0.5400000000000000355, 0.5600000000000000533, 0.5799999999999999600, 0.5999999999999999778, 0.6199999999999999956, 0.6400000000000000133, 0.6600000000000000311, 0.6800000000000000488, 0.6999999999999999556, 0.7199999999999999734, 0.7399999999999999911, 0.7600000000000000089, 0.7800000000000000266, 0.8000000000000000444, 0.8199999999999999512, 0.8399999999999999689, 0.8599999999999999867, 0.8800000000000000044, 0.9000000000000000222, 0.9200000000000000400, 0.9399999999999999467, 0.9599999999999999645, 0.9799999999999999822, 1.000000000000000000 ),
 .UNSPECIFIED. ) 
 CURVE ( )  GEOMETRIC_REPRESENTATION_ITEM ( )  RATIONAL_B_SPLINE_CURVE ( ( 1.000000000000000000, 0.9510565162951535312, 1.000000000000000000, 0.9510565162951535312, 1.000000000000000000, 0.9510565162951535312, 1.000000000000000000, 0.9510565162951535312, 1.000000000000000000, 0.9510565162951535312, 1.000000000000000000, 0.9510565162951535312, 1.000000000000000000, 0.9510565162951535312, 1.000000000000000000, 0.9510565162951535312, 1.000000000000000000, 0.9510565162951535312, 1.000000000000000000, 0.9510565162951535312, 1.000000000000000000, 0.9510565162951535312, 1.000000000000000000, 0.9510565162951535312, 1.000000000000000000, 0.9510565162951535312, 1.000000000000000000, 0.9510565162951535312, 1.000000000000000000, 0.9510565162951535312, 1.000000000000000000, 0.9510565162951535312, 1.000000000000000000, 0.9510565162951535312, 1.000000000000000000, 0.9510565162951535312, 1.000000000000000000, 0.9510565162951535312, 1.000000000000000000, 0.9510565162951535312, 1.000000000000000000, 0.9510565162951535312, 1.000000000000000000, 0.9510565162951535312, 1.000000000000000000, 0.9510565162951535312, 1.000000000000000000, 0.9510565162951535312, 1.000000000000000000, 0.9510565162951535312, 1.000000000000000000, 0.9510565162951535312, 1.000000000000000000, 0.9510565162951535312, 1.000000000000000000, 0.9510565162951535312, 1.000000000000000000, 0.9510565162951535312, 1.000000000000000000, 0.9510565162951535312, 1.000000000000000000, 0.9510565162951535312, 1.000000000000000000, 0.9510565162951535312, 1.000000000000000000, 0.9510565162951535312, 1.000000000000000000, 0.9510565162951535312, 1.000000000000000000, 0.9510565162951535312, 1.000000000000000000, 0.9510565162951535312, 1.000000000000000000, 0.9510565162951535312, 1.000000000000000000, 0.9510565162951535312, 1.000000000000000000, 0.9510565162951535312, 1.000000000000000000, 0.9510565162951535312, 1.000000000000000000, 0.9510565162951535312, 1.000000000000000000, 0.9510565162951535312, 1.000000000000000000, 0.9510565162951535312, 1.000000000000000000, 0.9510565162951535312, 1.000000000000000000, 0.9510565162951535312, 1.000000000000000000, 0.9510565162951535312, 1.000000000000000000, 0.9510565162951535312, 1.000000000000000000, 0.9510565162951535312, 1.000000000000000000, 0.9510565162951535312, 1.000000000000000000, 0.9510565162951535312, 1.000000000000000000 ) ) 
 REPRESENTATION_ITEM ( '' )  );
#1909 = VERTEX_POINT ( 'NONE', #12689 ) ;
#1910 = CARTESIAN_POINT ( 'NONE',  ( 52.31840720293882185, 36.04503594658365984, 5.908507747192915716 ) ) ;
#1911 = DIRECTION ( 'NONE',  ( 1.000000000000000000, 0.000000000000000000, -0.000000000000000000 ) ) ;
#1912 = CARTESIAN_POINT ( 'NONE',  ( 0.000000000000000000, 40.99999999999999289, 0.000000000000000000 ) ) ;
#1913 = ORIENTED_EDGE ( 'NONE', *, *, #9353, .T. ) ;
#1914 = CARTESIAN_POINT ( 'NONE',  ( 105.6631189606246295, 105.8855032339526758, -51.20000000000000995 ) ) ;
#1915 = CARTESIAN_POINT ( 'NONE',  ( -8.395938741299726615, 54.99999999495823033, -15.00000000000000000 ) ) ;
#1916 = CARTESIAN_POINT ( 'NONE',  ( 98.53841926354351699, 124.6500000010924651, -1.461580736456474794 ) ) ;
#1917 = CARTESIAN_POINT ( 'NONE',  ( 130.0000000000000000, 36.13828125216787157, -13.57481594606304576 ) ) ;
#1918 = CARTESIAN_POINT ( 'NONE',  ( 181.4251840539369596, 40.99999999999999289, 0.000000000000000000 ) ) ;
#1919 = CYLINDRICAL_SURFACE ( 'NONE', #9601, 13.57481594606304576 ) ;
#1920 = CARTESIAN_POINT ( 'NONE',  ( 204.2950502721270425, 34.69960937608393436, 9.295050272127046043 ) ) ;
#1921 = ORIENTED_EDGE ( 'NONE', *, *, #18755, .F. ) ;
#1922 = VERTEX_POINT ( 'NONE', #16975 ) ;
#1923 = CARTESIAN_POINT ( 'NONE',  ( 5.444914386472302859, 38.61875000108393152, 13.14518615778179189 ) ) ;
#1924 = CARTESIAN_POINT ( 'NONE',  ( 104.4587341249999781, -1.846868145590721655, 14.12500000136559208 ) ) ;
#1925 = CARTESIAN_POINT ( 'NONE',  ( 74.29505027212704249, 39.26367187608393294, 9.295050272127046043 ) ) ;
#1926 = CARTESIAN_POINT ( 'NONE',  ( 98.15313185440923860, 80.25000000136559208, -4.458734125000016313 ) ) ;
#1927 = CARTESIAN_POINT ( 'NONE',  ( 70.62287287157788285, 39.75976562716787299, 13.57481594606306174 ) ) ;
#1928 = CARTESIAN_POINT ( 'NONE',  ( 2.414731522848535132E-15, 40.15664062608393436, 13.14518615778179544 ) ) ;
#1929 = PLANE ( 'NONE',  #20036 ) ;
#1930 = DIRECTION ( 'NONE',  ( -0.000000000000000000, 1.000000000000000000, -0.000000000000000000 ) ) ;
#1931 = CARTESIAN_POINT ( 'NONE',  ( 185.7049497278729575, 39.85898437608393152, -9.295050272127046043 ) ) ;
#1932 = CARTESIAN_POINT ( 'NONE',  ( 91.91746824999997045, 112.6261737610028320, -47.72499999726881725 ) ) ;
#1933 = ORIENTED_EDGE ( 'NONE', *, *, #21365, .F. ) ;
#1934 = CARTESIAN_POINT ( 'NONE',  ( -5.622872871577873077, 39.26367187499999289, -13.57481594606304753 ) ) ;
#1935 = CARTESIAN_POINT ( 'NONE',  ( 5.444914386472297529, 40.30546875108393579, -13.14518615778179900 ) ) ;
#1936 = CARTESIAN_POINT ( 'NONE',  ( 104.9999999999999574, 2.071067811865491937, 0.6875000027311858330 ) ) ;
#1937 = CARTESIAN_POINT ( 'NONE',  ( 135.4449143864723055, 35.74140625108393721, -13.14518615778179900 ) ) ;
#1938 = CARTESIAN_POINT ( 'NONE',  ( 51.85481384221820633, 36.58476562608393579, 0.000000000000000000 ) ) ;
#1939 = CARTESIAN_POINT ( 'NONE',  ( 181.8548138422181921, 40.00781250108393294, 5.444914386472304635 ) ) ;
#1940 = DIRECTION ( 'NONE',  ( -0.000000000000000000, -1.000000000000000000, -0.000000000000000000 ) ) ;
#1941 = CARTESIAN_POINT ( 'NONE',  ( -13.14518615778179189, 35.04687500108393294, 5.444914386472304635 ) ) ;
#1942 = CARTESIAN_POINT ( 'NONE',  ( 124.6762090360452504, 54.47170356488336296, -14.99999999999999645 ) ) ;
#1943 = LINE ( 'NONE', #2081, #9860 ) ;
#1944 = CARTESIAN_POINT ( 'NONE',  ( 94.99999999999995737, 82.00000000000000000, -1.387778780781445676E-14 ) ) ;
#1945 = EDGE_CURVE ( 'NONE', #5360, #20854, #20129, .T. ) ;
#1946 = CARTESIAN_POINT ( 'NONE',  ( -9.295050272127044266, 39.85898437608393152, 9.295050272127047819 ) ) ;
#1947 = CARTESIAN_POINT ( 'NONE',  ( 9.180175813647995398, 55.00000000000000000, 14.99999999999999467 ) ) ;
#1948 = CARTESIAN_POINT ( 'NONE',  ( 102.4999999999999858, 123.1000000021849416, -9.847140817659276890E-15 ) ) ;
#1949 =( LENGTH_UNIT ( ) NAMED_UNIT ( * ) SI_UNIT ( .MILLI., .METRE. ) );
#1950 = CARTESIAN_POINT ( 'NONE',  ( 99.99999999999995737, 4.458734125000016313, 10.18750000136559208 ) ) ;
#1951 = CARTESIAN_POINT ( 'NONE',  ( 105.6631189606246295, 105.8855032339526758, -47.70000000546237828 ) ) ;
#1952 = ORIENTED_EDGE ( 'NONE', *, *, #18274, .F. ) ;
#1953 = CARTESIAN_POINT ( 'NONE',  ( 97.50000000000000000, 123.4500000021849502, -1.035533905932742416 ) ) ;
#1954 = CARTESIAN_POINT ( 'NONE',  ( 101.8468681455906903, -4.458734124999987891, 11.75000000136559208 ) ) ;
#1955 = CARTESIAN_POINT ( 'NONE',  ( 5.444914386472297529, 32.36796875108393579, -13.14518615778179722 ) ) ;
#1956 = AXIS2_PLACEMENT_3D ( 'NONE', #3228, #16186, #13751 ) ;
#1957 = CARTESIAN_POINT ( 'NONE',  ( 9.295050272127047819, 39.26367187608393294, 9.295050272127046043 ) ) ;
#1958 = CARTESIAN_POINT ( 'NONE',  ( 99.99999999999995737, 85.00000000000000000, -1.387778780781445676E-14 ) ) ;
#1959 = CARTESIAN_POINT ( 'NONE',  ( 98.15313185440925281, 83.50000000136560629, -4.458734125000016313 ) ) ;
#1960 = CARTESIAN_POINT ( 'NONE',  ( 51.85481384221819923, 38.32109375108394289, -5.444914386472297529 ) ) ;
#1961 = CARTESIAN_POINT ( 'NONE',  ( 91.91746824999998466, 112.6261737610028320, -51.22500000273119980 ) ) ;
#1962 = CARTESIAN_POINT ( 'NONE',  ( 2.414731522848535132E-15, 39.95820312608393010, 13.14518615778179544 ) ) ;
#1963 = ORIENTED_EDGE ( 'NONE', *, *, #22425, .T. ) ;
#1964 = FACE_OUTER_BOUND ( 'NONE', #11666, .T. ) ;
#1965 = CARTESIAN_POINT ( 'NONE',  ( 99.99999999999995737, -4.999999999999990230, 11.37500000273118594 ) ) ;
#1966 = CARTESIAN_POINT ( 'NONE',  ( 97.83688103937537051, 103.3426043859339103, -54.09999999453764019 ) ) ;
#1967 = CARTESIAN_POINT ( 'NONE',  ( 135.6228728715778686, 40.75195312500000711, -13.57481594606304753 ) ) ;
#1968 = ORIENTED_EDGE ( 'NONE', *, *, #8452, .F. ) ;
#1969 = CARTESIAN_POINT ( 'NONE',  ( 92.99999999999998579, 107.7255621263696526, -56.39999999453763024 ) ) ;
#1970 = CARTESIAN_POINT ( 'NONE',  ( 13.14518615778179900, 38.81718750108393579, -5.444914386472297529 ) ) ;
#1971 = CARTESIAN_POINT ( 'NONE',  ( 104.4587341249999781, 79.87500000136559208, 1.846868145590721655 ) ) ;
#1972 = CARTESIAN_POINT ( 'NONE',  ( 135.4449143864723055, 36.33671875108394289, -13.14518615778179900 ) ) ;
#1973 = CARTESIAN_POINT ( 'NONE',  ( 55.40115559117954547, 37.82500000216787583, -9.598844408820458085 ) ) ;
#1974 = CARTESIAN_POINT ( 'NONE',  ( 102.4976396683250783, 117.6869444889999841, -50.22499999726882436 ) ) ;
#1975 = CARTESIAN_POINT ( 'NONE',  ( -8.312177448680279460E-16, 35.34453125216787583, -13.57481594606304576 ) ) ;
#1976 = AXIS2_PLACEMENT_3D ( 'NONE', #26715, #492, #16144 ) ;
#1977 = CARTESIAN_POINT ( 'NONE',  ( 96.46446609406721961, 3.535533905932755072, 4.874999999999999112 ) ) ;
#1978 = EDGE_LOOP ( 'NONE', ( #4745, #16470, #24296, #6881 ) ) ;
#1979 = CARTESIAN_POINT ( 'NONE',  ( 189.5550856135277229, 36.73359375108393010, 13.14518615778179722 ) ) ;
#1980 = CARTESIAN_POINT ( 'NONE',  ( 74.59884440882045453, 39.11484374999999858, -9.598844408820458085 ) ) ;
#1981 = CARTESIAN_POINT ( 'NONE',  ( 120.7049497278729575, 38.07304687608393579, -9.295050272127046043 ) ) ;
#1982 = CARTESIAN_POINT ( 'NONE',  ( 185.4011555911795597, 38.02343750216788010, 9.598844408820459861 ) ) ;
#1983 = ADVANCED_FACE ( 'NONE', ( #14968 ), #6432, .T. ) ;
#1984 = CARTESIAN_POINT ( 'NONE',  ( 104.9999999999999574, 2.071067811865511032, 4.687500002731188609 ) ) ;
#1985 = CARTESIAN_POINT ( 'NONE',  ( 195.0000000000000000, 36.43593749999999432, 13.57481594606304576 ) ) ;
#1986 = CARTESIAN_POINT ( 'NONE',  ( 214.9999999999999716, 80.00000000000000000, -10.00000000000000000 ) ) ;
#1987 =( BOUNDED_CURVE ( )  B_SPLINE_CURVE ( 2, ( #10735, #19721, #207, #2488, #8892, #28142, #17582, #8609, #17297 ),
 .UNSPECIFIED., .F., .F. ) 
 B_SPLINE_CURVE_WITH_KNOTS ( ( 3, 2, 2, 2, 3 ),
 ( 0.1785714285714286031, 0.1875000000000000000, 0.1964285714285713969, 0.2053571428571428215, 0.2142857142857142183 ),
 .UNSPECIFIED. ) 
 CURVE ( )  GEOMETRIC_REPRESENTATION_ITEM ( )  RATIONAL_B_SPLINE_CURVE ( ( 0.9999999999999997780, 0.9238795325112869605, 1.000000000000000000, 0.9238795325112867385, 1.000000000000000000, 0.9238795325112867385, 1.000000000000000000, 0.9238795325112871826, 0.9999999999999995559 ) ) 
 REPRESENTATION_ITEM ( '' )  );
#1988 = CARTESIAN_POINT ( 'NONE',  ( -9.295050272127046043, 38.27148437608393294, -9.295050272127046043 ) ) ;
#1989 = CARTESIAN_POINT ( 'NONE',  ( -13.14518615778179900, 38.12265625108393152, -5.444914386472297529 ) ) ;
#1990 = CARTESIAN_POINT ( 'NONE',  ( 208.5748159460630120, 38.17226562499999432, 5.622872871577869525 ) ) ;
#1991 = CARTESIAN_POINT ( 'NONE',  ( 102.4976396683250925, 102.3130555110000159, -44.77500000273119696 ) ) ;
#1992 = CARTESIAN_POINT ( 'NONE',  ( 103.1528011352953342, 3.152801135295383084, 3.312500001365592972 ) ) ;
#1993 = CARTESIAN_POINT ( 'NONE',  ( 59.55508561352770158, 39.90859375108393436, 13.14518615778179722 ) ) ;
#1994 = CARTESIAN_POINT ( 'NONE',  ( 99.99999999999995737, -4.458734124999988779, 5.687500001365591196 ) ) ;
#1995 = FACE_OUTER_BOUND ( 'NONE', #27457, .T. ) ;
#1996 = CARTESIAN_POINT ( 'NONE',  ( 95.54126587499999346, 92.74999999863439371, -1.846868145590737864 ) ) ;
#1997 = CARTESIAN_POINT ( 'NONE',  ( -4.780039198850967175, 35.99999999999999289, 12.25280873422855699 ) ) ;
#1998 = CARTESIAN_POINT ( 'NONE',  ( 13.57481594606304576, 39.01562500000000000, -1.662435489736055892E-15 ) ) ;
#1999 = LINE ( 'NONE', #19096, #21722 ) ;
#2000 = VERTEX_POINT ( 'NONE', #4164 ) ;
#2001 = CARTESIAN_POINT ( 'NONE',  ( 103.5355339059327093, 83.62500000000000000, -3.535533905932755072 ) ) ;
#2002 = VECTOR ( 'NONE', #11775, 1000.000000000000000 ) ;
#2003 = CARTESIAN_POINT ( 'NONE',  ( 95.54126587499999346, 94.74999999863440792, -1.846868145590737864 ) ) ;
#2004 = ORIENTED_EDGE ( 'NONE', *, *, #25146, .F. ) ;
#2005 = CARTESIAN_POINT ( 'NONE',  ( 74.29505027212704249, 35.49335937608393721, 9.295050272127046043 ) ) ;
#2006 = EDGE_LOOP ( 'NONE', ( #20300, #6817, #20484, #23254 ) ) ;
#2007 = CARTESIAN_POINT ( 'NONE',  ( -8.312177448680279460E-16, 36.83281249999999574, -13.57481594606304576 ) ) ;
#2008 = CARTESIAN_POINT ( 'NONE',  ( 96.84719886470459471, -3.152801135295355994, 1.812500001365591640 ) ) ;
#2009 = ORIENTED_EDGE ( 'NONE', *, *, #16296, .F. ) ;
#2010 = CARTESIAN_POINT ( 'NONE',  ( 96.46446609406721961, 82.25000000273119838, 3.535533905932727539 ) ) ;
#2011 = CARTESIAN_POINT ( 'NONE',  ( 13.14518615778179900, 38.71796875108393721, 5.444914386472293977 ) ) ;
#2012 = CARTESIAN_POINT ( 'NONE',  ( 204.5988444088204687, 37.42812500216787441, 9.598844408820456309 ) ) ;
#2013 = ADVANCED_FACE ( 'NONE', ( #23687 ), #17400, .F. ) ;
#2014 = CARTESIAN_POINT ( 'NONE',  ( 13.14518615778179544, 36.18789062608393436, -1.609821015232357215E-15 ) ) ;
#2015 = CARTESIAN_POINT ( 'NONE',  ( 1.662435489736055892E-15, 40.99999999999999289, 13.57481594606304576 ) ) ;
#2016 = CARTESIAN_POINT ( 'NONE',  ( 104.3262379212492590, 104.0454443415356991, -51.29999999999999716 ) ) ;
#2017 = CARTESIAN_POINT ( 'NONE',  ( 143.1451861577818363, 40.40468750108393436, -5.444914386472297529 ) ) ;
#2018 = CARTESIAN_POINT ( 'NONE',  ( -13.14518615778179900, 37.52734375108393294, -5.444914386472297529 ) ) ;
#2019 = CARTESIAN_POINT ( 'NONE',  ( 130.0000000000000000, 34.79882812608393294, -13.14518615778179544 ) ) ;
#2020 = CARTESIAN_POINT ( 'NONE',  ( 51.42518405393695957, 37.03124999999999289, 0.000000000000000000 ) ) ;
#2021 = DIRECTION ( 'NONE',  ( -0.000000000000000000, -1.000000000000000000, -0.000000000000000000 ) ) ;
#2022 = EDGE_CURVE ( 'NONE', #19200, #27429, #21550, .T. ) ;
#2023 = CARTESIAN_POINT ( 'NONE',  ( 104.4587341249999781, 1.846868145590750299, 14.25000000136559208 ) ) ;
#2024 = CARTESIAN_POINT ( 'NONE',  ( 97.71650635000000307, 124.8750000005462368, -9.540979117872439019E-15 ) ) ;
#2025 = CONICAL_SURFACE ( 'NONE', #17016, 23.26794919243113213, 0.5235987755983000369 ) ;
#2026 = CARTESIAN_POINT ( 'NONE',  ( 104.4587341249999781, -1.846868145590721655, 3.875000001365592084 ) ) ;
#2027 = CARTESIAN_POINT ( 'NONE',  ( 106.5389055433251002, 105.2492070361643215, -52.32500000273119412 ) ) ;
#2028 = CYLINDRICAL_SURFACE ( 'NONE', #12076, 13.57481594606304576 ) ;
#2029 = CARTESIAN_POINT ( 'NONE',  ( 1.662435489736055892E-15, 40.99999999999999289, 13.57481594606304576 ) ) ;
#2030 = CARTESIAN_POINT ( 'NONE',  ( 9.295050272127047819, 32.11992187608393579, 9.295050272127046043 ) ) ;
#2031 = CARTESIAN_POINT ( 'NONE',  ( 99.99999999999995737, 5.000000000000018652, 7.875000002731185056 ) ) ;
#2032 = ADVANCED_FACE ( 'NONE', ( #10693 ), #23546, .T. ) ;
#2033 = CARTESIAN_POINT ( 'NONE',  ( 97.50236033167490746, 117.6869444889999841, -46.27499999726882152 ) ) ;
#2034 = ORIENTED_EDGE ( 'NONE', *, *, #20288, .F. ) ;
#2035 = CARTESIAN_POINT ( 'NONE',  ( 99.14382582708708469, 123.8000000010924566, -2.066987299999998751 ) ) ;
#2036 =( BOUNDED_CURVE ( )  B_SPLINE_CURVE ( 2, ( #5619, #3892, #12554, #27420, #10283, #1347, #27561, #1212, #18447 ),
 .UNSPECIFIED., .F., .F. ) 
 B_SPLINE_CURVE_WITH_KNOTS ( ( 3, 2, 2, 2, 3 ),
 ( 0.7500000000000000000, 0.7589285714285713969, 0.7678571428571429047, 0.7767857142857143016, 0.7857142857142856984 ),
 .UNSPECIFIED. ) 
 CURVE ( )  GEOMETRIC_REPRESENTATION_ITEM ( )  RATIONAL_B_SPLINE_CURVE ( ( 1.000000000000000000, 0.9238795325112867385, 1.000000000000000000, 0.9238795325112867385, 1.000000000000000000, 0.9238795325112867385, 1.000000000000000000, 0.9238795325112867385, 1.000000000000000000 ) ) 
 REPRESENTATION_ITEM ( '' )  );
#2037 = LINE ( 'NONE', #1761, #7534 ) ;
#2038 = CYLINDRICAL_SURFACE ( 'NONE', #23496, 7.000000000000006217 ) ;
#2039 = CARTESIAN_POINT ( 'NONE',  ( 0.000000000000000000, -1.000000000000001998, 0.000000000000000000 ) ) ;
#2040 = CARTESIAN_POINT ( 'NONE',  ( 181.8548138422181921, 38.12265625108393152, -5.444914386472297529 ) ) ;
#2041 = ORIENTED_EDGE ( 'NONE', *, *, #24047, .F. ) ;
#2042 = CARTESIAN_POINT ( 'NONE',  ( 99.99999999999995737, -4.999999999999990230, 7.375000002731185944 ) ) ;
#2043 = CARTESIAN_POINT ( 'NONE',  ( 92.99999999999998579, 107.7255621263696526, -54.90000000000001279 ) ) ;
#2044 = CARTESIAN_POINT ( 'NONE',  ( 57.38347467451918504, 54.91574374957784954, -14.99999999999999822 ) ) ;
#2045 = VERTEX_POINT ( 'NONE', #10416 ) ;
#2046 = CARTESIAN_POINT ( 'NONE',  ( 93.00000000000001421, 107.7255621263696668, -53.90000000000000568 ) ) ;
#2047 = CIRCLE ( 'NONE', #21610, 11.50000000000001421 ) ;
#2048 = CARTESIAN_POINT ( 'NONE',  ( 5.444914386472302859, 39.21406250108392300, 13.14518615778179189 ) ) ;
#2049 = CARTESIAN_POINT ( 'NONE',  ( 94.99999999999995737, 81.06250000273119838, -2.071067811865491493 ) ) ;
#2050 = CARTESIAN_POINT ( 'NONE',  ( 143.5748159460630404, 33.50898437716787015, 5.622872871577869525 ) ) ;
#2051 = CARTESIAN_POINT ( 'NONE',  ( 55.70494972787295751, 39.85898437608393152, -9.295050272127046043 ) ) ;
#2052 = LINE ( 'NONE', #21864, #24111 ) ;
#2053 = EDGE_CURVE ( 'NONE', #16548, #16918, #28122, .T. ) ;
#2054 = CARTESIAN_POINT ( 'NONE',  ( 208.1451861577817795, 33.95546875108393436, 5.444914386472293977 ) ) ;
#2055 = EDGE_LOOP ( 'NONE', ( #9944, #7722, #18909, #19495 ) ) ;
#2056 = VERTEX_POINT ( 'NONE', #9275 ) ;
#2057 = ORIENTED_EDGE ( 'NONE', *, *, #17510, .F. ) ;
#2058 = CARTESIAN_POINT ( 'NONE',  ( 9.295050272127046043, 38.07304687608393579, -9.295050272127046043 ) ) ;
#2059 = CARTESIAN_POINT ( 'NONE',  ( 96.84719886470459471, 3.152801135295383084, 10.56250000136559208 ) ) ;
#2060 = CARTESIAN_POINT ( 'NONE',  ( 78.14518615778179367, 40.15664062608393436, -1.609821015232357215E-15 ) ) ;
#2061 = CARTESIAN_POINT ( 'NONE',  ( 96.84719886470459471, 80.56250000136559208, 3.152801135295355994 ) ) ;
#2062 = CARTESIAN_POINT ( 'NONE',  ( 181.8548138422182205, 37.32890625108393579, -5.444914386472297529 ) ) ;
#2063 = CARTESIAN_POINT ( 'NONE',  ( 13.14518615778179722, 40.40468750108393436, -5.444914386472297529 ) ) ;
#2064 = LINE ( 'NONE', #4200, #25387 ) ;
#2065 = CARTESIAN_POINT ( 'NONE',  ( -13.57481594606304753, 37.77539062499998579, -5.622872871577872189 ) ) ;
#2066 = CARTESIAN_POINT ( 'NONE',  ( 78.57481594606305464, 39.75976562499999289, 5.622872871577868636 ) ) ;
#2067 = CARTESIAN_POINT ( 'NONE',  ( 104.9952793366501709, 103.1245878333314323, -52.92499999726882010 ) ) ;
#2068 = ORIENTED_EDGE ( 'NONE', *, *, #19448, .F. ) ;
#2069 = CARTESIAN_POINT ( 'NONE',  ( -5.622872871577873077, 36.88242187499999858, -13.57481594606304753 ) ) ;
#2070 = CARTESIAN_POINT ( 'NONE',  ( -5.444914386472299306, 35.93984375108392726, 13.14518615778179722 ) ) ;
#2071 = CIRCLE ( 'NONE', #5730, 5.000000000000000000 ) ;
#2072 = CIRCLE ( 'NONE', #4825, 13.57481594606304398 ) ;
#2073 = CARTESIAN_POINT ( 'NONE',  ( 99.99999999999995737, -4.999999999999990230, 3.375000002731184612 ) ) ;
#2074 = CARTESIAN_POINT ( 'NONE',  ( 143.1451861577818079, 35.59257812608393579, -1.609821015232357215E-15 ) ) ;
#2075 = CARTESIAN_POINT ( 'NONE',  ( 55.70494972787295751, 33.31054687608393294, -9.295050272127046043 ) ) ;
#2076 = CARTESIAN_POINT ( 'NONE',  ( 189.5550856135277229, 36.93203125108394147, 13.14518615778179722 ) ) ;
#2077 = ORIENTED_EDGE ( 'NONE', *, *, #19944, .F. ) ;
#2078 = CYLINDRICAL_SURFACE ( 'NONE', #4321, 5.000000000000004441 ) ;
#2079 = CARTESIAN_POINT ( 'NONE',  ( -5.444914386472297529, 36.43593750108392726, -13.14518615778179900 ) ) ;
#2080 = CARTESIAN_POINT ( 'NONE',  ( 136.1177599455525069, 54.65941425415165611, -14.99999999999999645 ) ) ;
#2081 = CARTESIAN_POINT ( 'NONE',  ( 130.0000000000000000, -7.395377635281828788, 13.57481594606302799 ) ) ;
#2082 = CARTESIAN_POINT ( 'NONE',  ( -9.295050272127046043, 33.50898437608393010, -9.295050272127046043 ) ) ;
#2083 = CARTESIAN_POINT ( 'NONE',  ( 95.00472066334981491, 103.1245878333314465, -52.82500000273118701 ) ) ;
#2084 = CARTESIAN_POINT ( 'NONE',  ( 5.444914386472297529, 37.92421875108392726, -13.14518615778179900 ) ) ;
#2085 = CARTESIAN_POINT ( 'NONE',  ( 99.99999999999995737, 5.000000000000018652, 10.75000000000000000 ) ) ;
#2086 = CARTESIAN_POINT ( 'NONE',  ( 97.50000000000000000, 122.6500000021849530, -1.035533905932742416 ) ) ;
#2087 = CARTESIAN_POINT ( 'NONE',  ( 58.09762142622420811, 51.13402819306927682, 15.00000000000063238 ) ) ;
#2088 = CARTESIAN_POINT ( 'NONE',  ( 95.54126587499995082, 1.846868145590750077, 8.375000001365592084 ) ) ;
#2089 = VECTOR ( 'NONE', #21736, 1000.000000000000000 ) ;
#2090 = ORIENTED_EDGE ( 'NONE', *, *, #5433, .T. ) ;
#2091 = FACE_OUTER_BOUND ( 'NONE', #20465, .T. ) ;
#2092 = CARTESIAN_POINT ( 'NONE',  ( 99.99999999999995737, -4.458734124999988779, 12.68750000136559208 ) ) ;
#2093 = CARTESIAN_POINT ( 'NONE',  ( 123.8389378251455639, 51.27996893916988341, 14.99999999999790745 ) ) ;
#2094 = CARTESIAN_POINT ( 'NONE',  ( 5.444914386472302859, 39.21406250108392300, 13.14518615778179189 ) ) ;
#2095 = CARTESIAN_POINT ( 'NONE',  ( 130.0000000000000000, 38.91640625216786731, 13.57481594606304576 ) ) ;
#2096 = CARTESIAN_POINT ( 'NONE',  ( 95.54126587499995082, 81.62500000136560629, -1.846868145590750077 ) ) ;
#2097 = CARTESIAN_POINT ( 'NONE',  ( 78.14518615778179367, 35.54296875108394715, 5.444914386472293977 ) ) ;
#2098 = CARTESIAN_POINT ( 'NONE',  ( 93.46109445667491400, 105.2492070361643215, -50.92500000273119554 ) ) ;
#2099 = CARTESIAN_POINT ( 'NONE',  ( -9.295050272127044266, 39.85898437608393152, 9.295050272127047819 ) ) ;
#2100 = VERTEX_POINT ( 'NONE', #11255 ) ;
#2101 = CARTESIAN_POINT ( 'NONE',  ( -13.57481594606304753, 39.36289062499999858, -5.622872871577872189 ) ) ;
#2102 = CARTESIAN_POINT ( 'NONE',  ( -8.312177448680279460E-16, 37.62656249999999858, -13.57481594606304576 ) ) ;
#2103 = CARTESIAN_POINT ( 'NONE',  ( 92.99999999999998579, 110.0000000000000000, -56.49999999453763877 ) ) ;
#2104 = CARTESIAN_POINT ( 'NONE',  ( 135.6228728715778971, 39.66054687500000142, 13.57481594606304576 ) ) ;
#2105 = VERTEX_POINT ( 'NONE', #22397 ) ;
#2106 = DIRECTION ( 'NONE',  ( -0.000000000000000000, 1.000000000000000000, -0.000000000000000000 ) ) ;
#2107 = ADVANCED_FACE ( 'NONE', ( #4727 ), #7272, .T. ) ;
#2108 = CARTESIAN_POINT ( 'NONE',  ( -13.14518615778179544, 38.37070312608393152, 0.000000000000000000 ) ) ;
#2109 = CARTESIAN_POINT ( 'NONE',  ( -13.57481594606304753, 36.28710937716787299, -5.622872871577873077 ) ) ;
#2110 = CARTESIAN_POINT ( 'NONE',  ( 124.5550856135277087, 35.14609375108393152, 13.14518615778179722 ) ) ;
#2111 = CARTESIAN_POINT ( 'NONE',  ( 55.40115559117954547, 35.44375000216787441, -9.598844408820458085 ) ) ;
#2112 = B_SPLINE_CURVE_WITH_KNOTS ( 'NONE', 3,
 ( #27313, #27033, #24738, #16025, #20471, #7629, #26744, #15884, #14171, #3498, #7479, #16321, #5361, #950, #9477, #9621, #1234, #22889, #26890, #11745, #12026, #7186, #20750, #5219, #12161, #9337, #16174, #14027, #7336, #809, #9897 ),
 .UNSPECIFIED., .F., .F.,
 ( 4, 2, 2, 2, 2, 2, 2, 2, 2, 2, 1, 2, 2, 2, 2, 4 ),
 ( 0.000000000000000000, 0.001656255954913781435, 0.003312511909827562870, 0.004968767864741344305, 0.005796895842198234589, 0.006625023819655125740, 0.008281279774568908042, 0.009937535729482686875, 0.01325004763931025148, 0.01490630359422403031, 0.01656255954913780915, 0.01821881550405159145, 0.01987507145896537028, 0.02318758336879293835, 0.02484383932370672066, 0.02650009527862050296 ),
 .UNSPECIFIED. ) ;
#2113 = CARTESIAN_POINT ( 'NONE',  ( 9.598844408820456309, 36.03906250216787299, -9.598844408820458085 ) ) ;
#2114 = VECTOR ( 'NONE', #17418, 1000.000000000000000 ) ;
#2115 = CARTESIAN_POINT ( 'NONE',  ( 94.99999999999995737, 2.071067811865491048, 6.937499999999999112 ) ) ;
#2116 = VERTEX_POINT ( 'NONE', #21973 ) ;
#2117 = CARTESIAN_POINT ( 'NONE',  ( 208.1451861577817795, 38.61875000108393152, -5.444914386472297529 ) ) ;
#2118 = DIRECTION ( 'NONE',  ( 5.782411586589358625E-17, -0.000000000000000000, 1.000000000000000000 ) ) ;
#2119 = CARTESIAN_POINT ( 'NONE',  ( 102.0710678118653618, 81.31250000000000000, 5.000000000000031086 ) ) ;
#2120 = ORIENTED_EDGE ( 'NONE', *, *, #20253, .T. ) ;
#2121 = DIRECTION ( 'NONE',  ( -1.000000000000000000, 8.275480229788910625E-32, 2.385244779468109755E-16 ) ) ;
#2122 = DIRECTION ( 'NONE',  ( 0.000000000000000000, 1.000000000000000000, 0.000000000000000000 ) ) ;
#2123 = CARTESIAN_POINT ( 'NONE',  ( 94.33688103937535629, 105.8855032339526758, -48.29999999453764303 ) ) ;
#2124 = CARTESIAN_POINT ( 'NONE',  ( -13.57481594606304576, 36.28710937499999289, 5.622872871577880183 ) ) ;
#2125 = CARTESIAN_POINT ( 'NONE',  ( 0.000000000000000000, 23.00000000000000000, -25.00000000000001066 ) ) ;
#2126 = VECTOR ( 'NONE', #11389, 1000.000000000000000 ) ;
#2127 = CARTESIAN_POINT ( 'NONE',  ( -8.049105076161786076E-16, 38.96601562608393721, -13.14518615778179544 ) ) ;
#2128 = CARTESIAN_POINT ( 'NONE',  ( 9.295050272127047819, 40.05742187608392868, 9.295050272127046043 ) ) ;
#2129 = CARTESIAN_POINT ( 'NONE',  ( 185.4011555911795597, 34.74921874999999716, 9.598844408820459861 ) ) ;
#2130 = B_SPLINE_CURVE_WITH_KNOTS ( 'NONE', 3,
 ( #24885, #11465, #4941, #2933, #22891, #20045, #20184, #9482, #9341, #26893, #24741, #11887, #20612, #13887, #1096, #9763, #22613, #7631, #16325, #26749, #25024, #5506, #7191, #3083, #14174 ),
 .UNSPECIFIED., .F., .F.,
 ( 4, 2, 2, 2, 2, 2, 2, 1, 2, 2, 2, 2, 4 ),
 ( 0.000000000000000000, 0.001301161269048799630, 0.002602322538097599260, 0.005204645076195198519, 0.007806967614292798646, 0.01040929015239039704, 0.01171045142143919970, 0.01301161269048800063, 0.01431277395953680330, 0.01561393522858560597, 0.01821625776668320262, 0.01951741903573200529, 0.02081858030478080449 ),
 .UNSPECIFIED. ) ;
#2131 = CARTESIAN_POINT ( 'NONE',  ( 99.99999999999998579, 118.4984768113314146, -45.87500000273119127 ) ) ;
#2132 = CARTESIAN_POINT ( 'NONE',  ( 195.0000000000000000, -7.395377635281828788, -13.57481594606306707 ) ) ;
#2133 = CARTESIAN_POINT ( 'NONE',  ( 70.44491438647230552, 37.13046875108393152, -13.14518615778179900 ) ) ;
#2134 = CARTESIAN_POINT ( 'NONE',  ( 104.4587341249999639, 1.442382525525748735E-14, 1.937500001365591640 ) ) ;
#2135 = DIRECTION ( 'NONE',  ( 5.782411586589357392E-17, -0.000000000000000000, 1.000000000000000000 ) ) ;
#2136 = CARTESIAN_POINT ( 'NONE',  ( 104.4587341249999923, 93.24999999863439371, 1.846868145590726318 ) ) ;
#2137 = AXIS2_PLACEMENT_3D ( 'NONE', #22959, #12369, #3421 ) ;
#2138 = CARTESIAN_POINT ( 'NONE',  ( 102.4999999999999858, 123.7999999999999972, -9.847140817659276890E-15 ) ) ;
#2139 = CARTESIAN_POINT ( 'NONE',  ( -9.598844408820454532, 35.54296874999999289, 9.598844408820459861 ) ) ;
#2140 = CARTESIAN_POINT ( 'NONE',  ( 94.99999999999995737, 1.387778780781445676E-14, 14.56250000136559208 ) ) ;
#2141 = VECTOR ( 'NONE', #25293, 1000.000000000000000 ) ;
#2142 = ORIENTED_EDGE ( 'NONE', *, *, #10358, .T. ) ;
#2143 = CARTESIAN_POINT ( 'NONE',  ( 94.99999999999995737, 85.00000000000000000, -1.387778780781445676E-14 ) ) ;
#2144 = ADVANCED_FACE ( 'NONE', ( #17970 ), #17688, .T. ) ;
#2145 = CARTESIAN_POINT ( 'NONE',  ( 95.54126587499999346, 91.87499999863439371, 1.846868145590722543 ) ) ;
#2146 = ORIENTED_EDGE ( 'NONE', *, *, #10490, .T. ) ;
#2147 = CARTESIAN_POINT ( 'NONE',  ( 107.0000000000000000, 112.2744378736303332, -47.90000000000000568 ) ) ;
#2148 = CARTESIAN_POINT ( 'NONE',  ( 74.29505027212704249, 36.28710937608393294, 9.295050272127046043 ) ) ;
#2149 = ORIENTED_EDGE ( 'NONE', *, *, #10165, .T. ) ;
#2150 = DIRECTION ( 'NONE',  ( 0.000000000000000000, 0.000000000000000000, 1.000000000000000000 ) ) ;
#2151 = CARTESIAN_POINT ( 'NONE',  ( 104.4587341249999781, 1.846868145590750299, 3.250000001365592528 ) ) ;
#2152 = ORIENTED_EDGE ( 'NONE', *, *, #26598, .F. ) ;
#2153 = CARTESIAN_POINT ( 'NONE',  ( -9.295050272127046043, 34.30273437608393294, -9.295050272127046043 ) ) ;
#2154 = CARTESIAN_POINT ( 'NONE',  ( -13.14518615778179189, 38.42031250108393436, 5.444914386472304635 ) ) ;
#2155 = UNCERTAINTY_MEASURE_WITH_UNIT (LENGTH_MEASURE( 1.000000000000000082E-05 ), #19187, 'distance_accuracy_value', 'NONE');
#2156 = CARTESIAN_POINT ( 'NONE',  ( 195.0000000000000000, 37.72578125216787726, -13.57481594606304576 ) ) ;
#2157 =( BOUNDED_CURVE ( )  B_SPLINE_CURVE ( 2, ( #26013, #4216, #6076, #14743, #12873, #4080, #6345, #13012, #10612 ),
 .UNSPECIFIED., .F., .F. ) 
 B_SPLINE_CURVE_WITH_KNOTS ( ( 3, 2, 2, 2, 3 ),
 ( 0.1458333333333336757, 0.1562500000000002776, 0.1666666666666669072, 0.1770833333333335369, 0.1875000000000001388 ),
 .UNSPECIFIED. ) 
 CURVE ( )  GEOMETRIC_REPRESENTATION_ITEM ( )  RATIONAL_B_SPLINE_CURVE ( ( 0.9999999999999975575, 0.9238795325112891810, 1.000000000000000000, 0.9238795325112867385, 1.000000000000000000, 0.9238795325112867385, 1.000000000000000000, 0.9238795325112857393, 1.000000000000001110 ) ) 
 REPRESENTATION_ITEM ( '' )  );
#2158 = CARTESIAN_POINT ( 'NONE',  ( 13.14518615778179722, 35.34453125108392157, 5.444914386472293977 ) ) ;
#2159 = CARTESIAN_POINT ( 'NONE',  ( 191.1360747348882398, 54.10645156200111927, 14.99999999999995026 ) ) ;
#2160 = CARTESIAN_POINT ( 'NONE',  ( 143.1451861577818363, 36.33671875108393579, 5.444914386472293977 ) ) ;
#2161 = CARTESIAN_POINT ( 'NONE',  ( -5.444914386472299306, 37.72578125108395142, 13.14518615778179722 ) ) ;
#2162 = CARTESIAN_POINT ( 'NONE',  ( 116.8548138422182063, 33.36015625108393579, -5.444914386472297529 ) ) ;
#2163 = CARTESIAN_POINT ( 'NONE',  ( 51.42518405393695957, 33.11210937499999574, 5.622872871577880183 ) ) ;
#2164 = FACE_OUTER_BOUND ( 'NONE', #18756, .T. ) ;
#2165 = CARTESIAN_POINT ( 'NONE',  ( 104.4587341249999639, 1.442382525525748735E-14, 1.937500001365591640 ) ) ;
#2166 = CARTESIAN_POINT ( 'NONE',  ( 93.00000000000000000, 112.2744378736303190, -46.10000000000000142 ) ) ;
#2167 = ADVANCED_FACE ( 'NONE', ( #453 ), #4873, .F. ) ;
#2168 = CARTESIAN_POINT ( 'NONE',  ( 99.99999999999995737, -4.458734124999988779, 13.68750000136559208 ) ) ;
#2169 = CARTESIAN_POINT ( 'NONE',  ( 93.46109445667491400, 105.2492070361643215, -50.92500000273119554 ) ) ;
#2170 = CARTESIAN_POINT ( 'NONE',  ( 98.15313185440923860, -4.458734124999987891, 0.8750000013655925279 ) ) ;
#2171 = AXIS2_PLACEMENT_3D ( 'NONE', #12525, #14541, #6274 ) ;
#2172 = CARTESIAN_POINT ( 'NONE',  ( 104.4587341249999639, 80.18750000136559208, -1.442382525525748735E-14 ) ) ;
#2173 = CARTESIAN_POINT ( 'NONE',  ( 104.9952793366501567, 103.1245878333314465, -48.92499999726882010 ) ) ;
#2174 = CARTESIAN_POINT ( 'NONE',  ( -13.14518615778179189, 37.62656250108393863, 5.444914386472304635 ) ) ;
#2175 = CARTESIAN_POINT ( 'NONE',  ( 93.46109445667489979, 105.2492070361643215, -47.67499999726882720 ) ) ;
#2176 = ORIENTED_EDGE ( 'NONE', *, *, #19611, .T. ) ;
#2177 = FACE_OUTER_BOUND ( 'NONE', #4881, .T. ) ;
#2179 = ADVANCED_FACE ( 'NONE', ( #2450 ), #15683, .T. ) ;
#2178 = CARTESIAN_POINT ( 'NONE',  ( 101.4615807364564546, 123.4500000010924765, -1.461580736456474794 ) ) ;
#2180 = CARTESIAN_POINT ( 'NONE',  ( 189.3771271284220745, 36.08867187500000284, -13.57481594606300135 ) ) ;
#2181 = EDGE_CURVE ( 'NONE', #162, #7211, #22258, .T. ) ;
#2182 = CARTESIAN_POINT ( 'NONE',  ( 181.8548138422181921, 40.50390625108394005, -5.444914386472297529 ) ) ;
#2183 = VERTEX_POINT ( 'NONE', #8850 ) ;
#2184 = CARTESIAN_POINT ( 'NONE',  ( 0.000000000000000000, 29.95886589889650509, 0.000000000000000000 ) ) ;
#2185 = EDGE_CURVE ( 'NONE', #540, #11153, #11537, .T. ) ;
#2186 = CYLINDRICAL_SURFACE ( 'NONE', #13412, 4.999999999999999112 ) ;
#2187 = CARTESIAN_POINT ( 'NONE',  ( 104.4587341249999781, 1.846868145590750299, 14.25000000136559208 ) ) ;
#2188 = ORIENTED_EDGE ( 'NONE', *, *, #7577, .F. ) ;
#2189 = CARTESIAN_POINT ( 'NONE',  ( 95.67376207875072680, 115.9545556584642867, -52.30000000000001137 ) ) ;
#2190 = CARTESIAN_POINT ( 'NONE',  ( 13.14518615778179900, 40.10703125108393152, 5.444914386472293977 ) ) ;
#2191 = CARTESIAN_POINT ( 'NONE',  ( 97.93301270000000613, 123.9500000010924765, -9.540979117872439019E-15 ) ) ;
#2192 = EDGE_CURVE ( 'NONE', #923, #14907, #3043, .T. ) ;
#2193 = CARTESIAN_POINT ( 'NONE',  ( 143.1451861577818079, 39.41250000108393436, -5.444914386472297529 ) ) ;
#2194 = DIRECTION ( 'NONE',  ( -0.000000000000000000, -1.000000000000000000, -0.000000000000000000 ) ) ;
#2195 = CARTESIAN_POINT ( 'NONE',  ( 103.5355339059327235, 92.74999999726881583, 3.535533905932724874 ) ) ;
#2196 = CARTESIAN_POINT ( 'NONE',  ( 74.29505027212704249, 40.25585937608393294, 9.295050272127046043 ) ) ;
#2197 = CARTESIAN_POINT ( 'NONE',  ( 99.99999999999998579, 110.0000000000000000, -145.0000000000000284 ) ) ;
#2198 = CARTESIAN_POINT ( 'NONE',  ( 181.8548138422182205, 34.40195312608393152, 0.000000000000000000 ) ) ;
#2199 = VERTEX_POINT ( 'NONE', #7127 ) ;
#2200 =( BOUNDED_CURVE ( )  B_SPLINE_CURVE ( 2, ( #2881, #18127, #19840, #468, #22129, #24400, #9013, #5168, #10985 ),
 .UNSPECIFIED., .F., .T. ) 
 B_SPLINE_CURVE_WITH_KNOTS ( ( 3, 2, 2, 2, 3 ),
 ( 0.02083333333333358892, 0.03125000000000020123, 0.04166666666666681007, 0.05208333333333342585, 0.06250000000000004163 ),
 .UNSPECIFIED. ) 
 CURVE ( )  GEOMETRIC_REPRESENTATION_ITEM ( )  RATIONAL_B_SPLINE_CURVE ( ( 0.9999999999999981126, 0.9238795325112886259, 1.000000000000000000, 0.9238795325112867385, 1.000000000000000000, 0.9238795325112867385, 1.000000000000000000, 0.9238795325112864054, 1.000000000000000222 ) ) 
 REPRESENTATION_ITEM ( '' )  );
#2201 = ORIENTED_EDGE ( 'NONE', *, *, #6469, .F. ) ;
#2202 = CARTESIAN_POINT ( 'NONE',  ( -8.049105076161786076E-16, 40.55351562608393579, -13.14518615778179544 ) ) ;
#2203 = CARTESIAN_POINT ( 'NONE',  ( 96.84719886470459471, -3.152801135295355994, 10.81250000136559208 ) ) ;
#2204 = CARTESIAN_POINT ( 'NONE',  ( 59.55508561352770158, 39.11484375108393863, 13.14518615778179722 ) ) ;
#2205 = EDGE_CURVE ( 'NONE', #8864, #26666, #22169, .T. ) ;
#2206 = CARTESIAN_POINT ( 'NONE',  ( 104.4587341249999781, 82.87500000136560629, 1.846868145590721655 ) ) ;
#2207 = CARTESIAN_POINT ( 'NONE',  ( 195.0000000000000000, 37.57695312608392868, 13.14518615778179544 ) ) ;
#2208 = CARTESIAN_POINT ( 'NONE',  ( 13.14518615778179722, 39.51171875108393294, 5.444914386472293977 ) ) ;
#2209 = CARTESIAN_POINT ( 'NONE',  ( -5.622872871577890841, 39.66054687716787441, 13.57481594606302444 ) ) ;
#2210 = DIRECTION ( 'NONE',  ( -0.000000000000000000, -1.000000000000000000, -0.000000000000000000 ) ) ;
#2211 = DIRECTION ( 'NONE',  ( -0.000000000000000000, 1.000000000000000000, -0.000000000000000000 ) ) ;
#2212 = CARTESIAN_POINT ( 'NONE',  ( 102.4976396683250783, 102.3130555110000159, -55.02499999726882152 ) ) ;
#2213 = AXIS2_PLACEMENT_3D ( 'NONE', #10774, #17198, #4241 ) ;
#2214 = VERTEX_POINT ( 'NONE', #20117 ) ;
#2215 = EDGE_CURVE ( 'NONE', #21433, #24113, #15951, .T. ) ;
#2216 = CARTESIAN_POINT ( 'NONE',  ( -13.57481594606304576, 37.03124999999999289, 0.000000000000000000 ) ) ;
#2217 = CARTESIAN_POINT ( 'NONE',  ( -13.14518615778179189, 35.84062500108394289, 5.444914386472304635 ) ) ;
#2218 = CARTESIAN_POINT ( 'NONE',  ( 94.99999999999995737, 2.071067811865491048, 3.062500002731186388 ) ) ;
#2219 = CARTESIAN_POINT ( 'NONE',  ( 116.8548138422182205, 35.19570312608393436, 0.000000000000000000 ) ) ;
#2220 = CARTESIAN_POINT ( 'NONE',  ( 78.14518615778179367, 34.60039062608392868, -1.609821015232357215E-15 ) ) ;
#2221 = EDGE_CURVE ( 'NONE', #7002, #12839, #26826, .T. ) ;
#2222 = CARTESIAN_POINT ( 'NONE',  ( 185.7049497278729575, 36.68398437608393436, -9.295050272127046043 ) ) ;
#2223 = CARTESIAN_POINT ( 'NONE',  ( 97.83688103937537051, 103.3426043859339103, -46.10000000546238397 ) ) ;
#2224 = SURFACE_SIDE_STYLE ('',( #24019 ) ) ;
#2225 = CARTESIAN_POINT ( 'NONE',  ( 139.1801758136479918, 50.00000000000002132, -15.00000000000000000 ) ) ;
#2226 = CARTESIAN_POINT ( 'NONE',  ( 188.6617095634187251, 36.00000000000002132, 11.53991937534743784 ) ) ;
#2227 = FACE_OUTER_BOUND ( 'NONE', #10725, .T. ) ;
#2228 = CARTESIAN_POINT ( 'NONE',  ( 102.4976396683250925, 117.6869444889999841, -53.72500000273119980 ) ) ;
#2229 = CARTESIAN_POINT ( 'NONE',  ( 13.14518615778179900, 36.93203125108394147, 5.444914386472293977 ) ) ;
#2230 = EDGE_CURVE ( 'NONE', #4960, #27535, #2323, .T. ) ;
#2231 = CARTESIAN_POINT ( 'NONE',  ( -9.598844408820454532, 34.74921874999999716, 9.598844408820459861 ) ) ;
#2232 = FACE_OUTER_BOUND ( 'NONE', #7500, .T. ) ;
#2233 = VECTOR ( 'NONE', #26227, 1000.000000000000000 ) ;
#2234 = CARTESIAN_POINT ( 'NONE',  ( 58.54912065733758197, 50.00000000106957998, 11.97362904075674983 ) ) ;
#2235 = AXIS2_PLACEMENT_3D ( 'NONE', #6523, #264, #15201 ) ;
#2236 = CARTESIAN_POINT ( 'NONE',  ( 95.54126587499995082, -1.846868145590724986, 7.500000001365592084 ) ) ;
#2237 = ORIENTED_EDGE ( 'NONE', *, *, #16828, .F. ) ;
#2238 = CARTESIAN_POINT ( 'NONE',  ( 98.53841926354351699, 122.8500000010924680, -1.461580736456474794 ) ) ;
#2239 = CARTESIAN_POINT ( 'NONE',  ( 101.8468681455906903, 4.458734125000016313, 11.12500000136559386 ) ) ;
#2240 = CARTESIAN_POINT ( 'NONE',  ( 130.3286002765670446, 53.49358765999040344, 14.99999999999996447 ) ) ;
#2241 = CARTESIAN_POINT ( 'NONE',  ( -13.14518615778179189, 39.01562500108393294, 5.444914386472304635 ) ) ;
#2242 = DIRECTION ( 'NONE',  ( 0.000000000000000000, 0.000000000000000000, -1.000000000000000000 ) ) ;
#2243 = CARTESIAN_POINT ( 'NONE',  ( 104.4587341249999781, 81.12500000136559208, 1.846868145590721655 ) ) ;
#2244 = CARTESIAN_POINT ( 'NONE',  ( 70.44491438647230552, 34.94765625108394147, -13.14518615778179900 ) ) ;
#2245 = CARTESIAN_POINT ( 'NONE',  ( 97.50236033167492167, 117.6869444889999841, -51.52500000273119696 ) ) ;
#2246 = CARTESIAN_POINT ( 'NONE',  ( 108.0825317500000153, 110.0000000000000000, -44.37500000273119838 ) ) ;
#2247 = B_SPLINE_CURVE_WITH_KNOTS ( 'NONE', 3,
 ( #26875, #18454, #5344, #2915 ),
 .UNSPECIFIED., .F., .F.,
 ( 4, 4 ),
 ( 0.000000000000000000, 1.000000000000000000 ),
 .UNSPECIFIED. ) ;
#2248 = CYLINDRICAL_SURFACE ( 'NONE', #9842, 13.57481594606304576 ) ;
#2249 = CARTESIAN_POINT ( 'NONE',  ( 104.7293670624999748, 95.71874999795160477, -6.938893903907228378E-15 ) ) ;
#2250 = DIRECTION ( 'NONE',  ( -0.000000000000000000, -1.000000000000000000, -0.000000000000000000 ) ) ;
#2251 = CARTESIAN_POINT ( 'NONE',  ( 139.5988444088204687, 38.91640624999999432, 9.598844408820456309 ) ) ;
#2252 = ADVANCED_FACE ( 'NONE', ( #16108 ), #20826, .T. ) ;
#2253 = ORIENTED_EDGE ( 'NONE', *, *, #27597, .F. ) ;
#2254 = CARTESIAN_POINT ( 'NONE',  ( -8.312177448680279460E-16, 34.55078125216787299, -13.57481594606304576 ) ) ;
#2255 = CARTESIAN_POINT ( 'NONE',  ( -13.14518615778179544, 37.57695312608393579, 0.000000000000000000 ) ) ;
#2256 = CARTESIAN_POINT ( 'NONE',  ( -5.622872871577873077, 37.27929687716787299, 13.57481594606304753 ) ) ;
#2257 = CARTESIAN_POINT ( 'NONE',  ( 116.8548138422182205, 35.79101562608393294, 0.000000000000000000 ) ) ;
#2258 = CARTESIAN_POINT ( 'NONE',  ( 65.00000000000000000, 33.36015625216786873, 13.57481594606304576 ) ) ;
#2259 = VERTEX_POINT ( 'NONE', #9559 ) ;
#2260 = DIRECTION ( 'NONE',  ( 0.000000000000000000, -1.000000000000000000, 0.000000000000000000 ) ) ;
#2261 = STYLED_ITEM ( 'NONE', ( #5076 ), #2892 ) ;
#2262 = CARTESIAN_POINT ( 'NONE',  ( 7.171391395016640580, 31.30502190640808990, -11.52591746582321974 ) ) ;
#2263 = AXIS2_PLACEMENT_3D ( 'NONE', #26535, #15966, #13820 ) ;
#2264 = CARTESIAN_POINT ( 'NONE',  ( 97.92893218813451028, -4.999999999999989342, 6.187499999999999112 ) ) ;
#2265 = CARTESIAN_POINT ( 'NONE',  ( 93.46109445667489979, 105.2492070361643215, -49.67499999726882010 ) ) ;
#2266 = CARTESIAN_POINT ( 'NONE',  ( 208.1451861577817795, 34.65000000108393152, -5.444914386472297529 ) ) ;
#2267 = DIRECTION ( 'NONE',  ( -0.000000000000000000, 1.000000000000000000, -0.000000000000000000 ) ) ;
#2268 = CARTESIAN_POINT ( 'NONE',  ( 104.9999999999999716, 81.50000000000000000, -1.449011120738813565E-14 ) ) ;
#2269 = CARTESIAN_POINT ( 'NONE',  ( 98.23223304703363112, 122.8000000021849587, 1.767766952966351557 ) ) ;
#2270 = CARTESIAN_POINT ( 'NONE',  ( 99.99999999999998579, 123.6000000000000085, 2.499999999999978684 ) ) ;
#2271 = CARTESIAN_POINT ( 'NONE',  ( 200.6228728715778118, 39.26367187716788010, -13.57481594606312036 ) ) ;
#2272 = CARTESIAN_POINT ( 'NONE',  ( -13.57481594606304576, 37.82499999999999574, 0.000000000000000000 ) ) ;
#2273 = CARTESIAN_POINT ( 'NONE',  ( 0.000000000000000000, 40.99999999999999289, -15.57481594606304576 ) ) ;
#2274 = CARTESIAN_POINT ( 'NONE',  ( -9.295050272127044266, 37.67617187608393436, 9.295050272127047819 ) ) ;
#2275 = CARTESIAN_POINT ( 'NONE',  ( 2.414731522848535132E-15, 39.16445312608392726, 13.14518615778179544 ) ) ;
#2276 = CARTESIAN_POINT ( 'NONE',  ( 208.5748159460630120, 33.50898437499999716, -5.622872871577873077 ) ) ;
#2277 = DIRECTION ( 'NONE',  ( 0.000000000000000000, 0.000000000000000000, -1.000000000000000000 ) ) ;
#2278 = DIRECTION ( 'NONE',  ( 0.000000000000000000, 0.000000000000000000, -1.000000000000000000 ) ) ;
#2279 = CARTESIAN_POINT ( 'NONE',  ( 70.44491438647230552, 35.54296875108393294, -13.14518615778179900 ) ) ;
#2280 = DIRECTION ( 'NONE',  ( 0.000000000000000000, 0.000000000000000000, 1.000000000000000000 ) ) ;
#2281 = CARTESIAN_POINT ( 'NONE',  ( 93.00000000000001421, 112.2744378736303332, -44.60000000546238397 ) ) ;
#2282 = CARTESIAN_POINT ( 'NONE',  ( 95.54126587499999346, 91.87499999863439371, 1.846868145590722543 ) ) ;
#2283 = CARTESIAN_POINT ( 'NONE',  ( 99.20899822134843760, 123.0000000000000000, -1.909647267044714436 ) ) ;
#2284 = CARTESIAN_POINT ( 'NONE',  ( 5.622872871577871301, 35.19570312499999432, -13.57481594606304753 ) ) ;
#2285 = CARTESIAN_POINT ( 'NONE',  ( 143.1451861577818079, 37.18007812608393436, -1.609821015232357215E-15 ) ) ;
#2286 = ORIENTED_EDGE ( 'NONE', *, *, #22272, .T. ) ;
#2287 = VERTEX_POINT ( 'NONE', #24953 ) ;
#2288 = CARTESIAN_POINT ( 'NONE',  ( 104.9999999999999574, 84.56250000000002842, -2.071067811865491937 ) ) ;
#2289 = CARTESIAN_POINT ( 'NONE',  ( 97.92893218813451028, 83.93750000273119838, -5.000000000000018652 ) ) ;
#2290 = CARTESIAN_POINT ( 'NONE',  ( 96.84719886470463734, 93.68749999863440792, -3.152801135295366208 ) ) ;
#2291 = CARTESIAN_POINT ( 'NONE',  ( 13.57481594606304931, 34.20351562499999432, 5.622872871577868636 ) ) ;
#2292 = ORIENTED_EDGE ( 'NONE', *, *, #20278, .F. ) ;
#2293 = CARTESIAN_POINT ( 'NONE',  ( 107.0000000000000000, 107.7255621263696668, -52.10000000000001563 ) ) ;
#2294 = CARTESIAN_POINT ( 'NONE',  ( 59.55508561352770158, 34.25312500108393010, -13.14518615778179900 ) ) ;
#2295 = ORIENTED_EDGE ( 'NONE', *, *, #13803, .F. ) ;
#2296 = CARTESIAN_POINT ( 'NONE',  ( 135.6228728715777834, 39.26367187716788010, -13.57481594606312036 ) ) ;
#2297 = CARTESIAN_POINT ( 'NONE',  ( 96.84719886470459471, 3.152801135295383084, 2.562500001365592084 ) ) ;
#2298 = ORIENTED_EDGE ( 'NONE', *, *, #2382, .T. ) ;
#2299 = CARTESIAN_POINT ( 'NONE',  ( 9.295050272127046043, 35.69179687608394147, -9.295050272127046043 ) ) ;
#2300 = CARTESIAN_POINT ( 'NONE',  ( 13.14518615778179900, 39.51171875108392584, 5.444914386472293977 ) ) ;
#2301 = CARTESIAN_POINT ( 'NONE',  ( 185.4011555911795597, 38.02343750216788010, 9.598844408820459861 ) ) ;
#2302 = CARTESIAN_POINT ( 'NONE',  ( 5.444914386472297529, 37.13046875108393152, -13.14518615778179722 ) ) ;
#2303 = LINE ( 'NONE', #26090, #17632 ) ;
#2304 = DIRECTION ( 'NONE',  ( -0.000000000000000000, 1.000000000000000000, -0.000000000000000000 ) ) ;
#2305 = ORIENTED_EDGE ( 'NONE', *, *, #5823, .F. ) ;
#2307 = AXIS2_PLACEMENT_3D ( 'NONE', #10384, #15073, #23791 ) ;
#2306 = CARTESIAN_POINT ( 'NONE',  ( -9.295050272127046043, 39.85898437608393152, -9.295050272127046043 ) ) ;
#2308 = EDGE_CURVE ( 'NONE', #6173, #370, #16868, .T. ) ;
#2309 = CARTESIAN_POINT ( 'NONE',  ( 130.0000000000000000, 35.59257812608393579, -13.14518615778179544 ) ) ;
#2310 = CARTESIAN_POINT ( 'NONE',  ( 74.59884440882045453, 35.93984374999999432, -9.598844408820458085 ) ) ;
#2311 = CARTESIAN_POINT ( 'NONE',  ( 0.000000000000000000, 40.99999999999999289, 0.000000000000000000 ) ) ;
#2312 = CARTESIAN_POINT ( 'NONE',  ( 99.99999999999995737, 4.458734125000016313, 11.43750000136559208 ) ) ;
#2313 = CARTESIAN_POINT ( 'NONE',  ( 84.99999999999998579, 125.0000000000000000, 14.99999999999999112 ) ) ;
#2314 = CARTESIAN_POINT ( 'NONE',  ( 103.1528011352953342, -3.152801135295355106, 12.81250000136559208 ) ) ;
#2315 = LINE ( 'NONE', #15103, #16400 ) ;
#2316 = DIRECTION ( 'NONE',  ( -0.000000000000000000, -1.000000000000000000, -0.000000000000000000 ) ) ;
#2317 = FACE_OUTER_BOUND ( 'NONE', #13417, .T. ) ;
#2318 = CARTESIAN_POINT ( 'NONE',  ( 91.91746824999997045, 112.6261737610028320, -51.72499999726882436 ) ) ;
#2319 = CARTESIAN_POINT ( 'NONE',  ( -13.14518615778179189, 36.83281250108393579, 5.444914386472304635 ) ) ;
#2320 = CARTESIAN_POINT ( 'NONE',  ( 91.91746824999998466, 110.0000000000000000, -47.87499999726882294 ) ) ;
#2321 = ORIENTED_EDGE ( 'NONE', *, *, #2520, .T. ) ;
#2322 = CARTESIAN_POINT ( 'NONE',  ( 98.53841926354351699, 124.0500000010924708, 1.461580736456455920 ) ) ;
#2323 =( BOUNDED_CURVE ( )  B_SPLINE_CURVE ( 2, ( #169, #6703, #15391, #24103, #4581, #13241, #18816, #24677, #16541 ),
 .UNSPECIFIED., .F., .F. ) 
 B_SPLINE_CURVE_WITH_KNOTS ( ( 3, 2, 2, 2, 3 ),
 ( 0.3958333333333331483, 0.4062499999999999445, 0.4166666666666667407, 0.4270833333333335369, 0.4375000000000003331 ),
 .UNSPECIFIED. ) 
 CURVE ( )  GEOMETRIC_REPRESENTATION_ITEM ( )  RATIONAL_B_SPLINE_CURVE ( ( 1.000000000000001110, 0.9238795325112855172, 1.000000000000000000, 0.9238795325112867385, 1.000000000000000000, 0.9238795325112867385, 1.000000000000000000, 0.9238795325112842960, 1.000000000000002442 ) ) 
 REPRESENTATION_ITEM ( '' )  );
#2324 = DIRECTION ( 'NONE',  ( -0.000000000000000000, 1.000000000000000000, -0.000000000000000000 ) ) ;
#2325 = CARTESIAN_POINT ( 'NONE',  ( 219.9999999999999716, 80.00000000000000000, -10.00000000000000178 ) ) ;
#2326 = CARTESIAN_POINT ( 'NONE',  ( 208.1451861577817795, 38.51953125108393294, 5.444914386472293977 ) ) ;
#2327 = ORIENTED_EDGE ( 'NONE', *, *, #10555, .T. ) ;
#2328 = CARTESIAN_POINT ( 'NONE',  ( 74.29505027212704249, 36.48554687608393721, -9.295050272127046043 ) ) ;
#2329 = CARTESIAN_POINT ( 'NONE',  ( 191.2025481310419366, 54.08938259242988522, -15.00000000000000000 ) ) ;
#2330 = VERTEX_POINT ( 'NONE', #888 ) ;
#2331 = CARTESIAN_POINT ( 'NONE',  ( 105.6631189606246295, 114.1144967660473242, -48.80000000000001137 ) ) ;
#2332 = CARTESIAN_POINT ( 'NONE',  ( 2.414731522848535132E-15, 39.95820312608393010, 13.14518615778179544 ) ) ;
#2333 = CARTESIAN_POINT ( 'NONE',  ( 94.99999999999995737, 81.12500000273119838, -1.387778780781445676E-14 ) ) ;
#2334 = CARTESIAN_POINT ( 'NONE',  ( 139.2950502721270425, 40.25585937608393294, -9.295050272127046043 ) ) ;
#2335 = CARTESIAN_POINT ( 'NONE',  ( -8.049105076161786076E-16, 39.75976562608394005, -13.14518615778179544 ) ) ;
#2336 = CARTESIAN_POINT ( 'NONE',  ( 103.5355339059327235, 95.74999999726881583, 3.535533905932724874 ) ) ;
#2337 = CARTESIAN_POINT ( 'NONE',  ( 65.00000000000000000, 38.96601562608393721, -13.14518615778179544 ) ) ;
#2338 = EDGE_CURVE ( 'NONE', #27581, #18466, #22719, .T. ) ;
#2339 = CARTESIAN_POINT ( 'NONE',  ( 0.000000000000000000, 40.99999999999999289, 0.000000000000000000 ) ) ;
#2340 = CARTESIAN_POINT ( 'NONE',  ( 195.0000000000000000, 34.99726562608393721, -13.14518615778179544 ) ) ;
#2341 = EDGE_LOOP ( 'NONE', ( #8716, #25264, #2913, #16596 ) ) ;
#2342 = ADVANCED_FACE ( 'NONE', ( #12099 ), #5329, .T. ) ;
#2343 = ORIENTED_EDGE ( 'NONE', *, *, #5269, .T. ) ;
#2344 = VERTEX_POINT ( 'NONE', #13960 ) ;
#2345 = CARTESIAN_POINT ( 'NONE',  ( -13.14518615778179900, 38.32109375108394289, -5.444914386472297529 ) ) ;
#2346 = APPLICATION_PROTOCOL_DEFINITION ( 'draft international standard', 'automotive_design', 1998, #23898 ) ;
#2347 = CARTESIAN_POINT ( 'NONE',  ( 104.4587341249999639, 1.442382525525748735E-14, 11.18750000136559208 ) ) ;
#2348 = CARTESIAN_POINT ( 'NONE',  ( 101.0355339059327235, 124.4499999999999744, 2.499999999999974687 ) ) ;
#2349 = CARTESIAN_POINT ( 'NONE',  ( 104.4587341249999781, 81.00000000136560629, -1.846868145590750521 ) ) ;
#2350 = CARTESIAN_POINT ( 'NONE',  ( 195.0000000000000000, 39.95820312608393010, 13.14518615778179544 ) ) ;
#2351 = CARTESIAN_POINT ( 'NONE',  ( -9.295050272127044266, 38.46992187608393721, 9.295050272127047819 ) ) ;
#2352 = FACE_OUTER_BOUND ( 'NONE', #19097, .T. ) ;
#2353 = CARTESIAN_POINT ( 'NONE',  ( 65.00000000000000000, -7.395377635281828788, 13.57481594606303688 ) ) ;
#2354 = CARTESIAN_POINT ( 'NONE',  ( 181.8548138422182205, 40.70234375108392300, -5.444914386472297529 ) ) ;
#2355 = CARTESIAN_POINT ( 'NONE',  ( 106.5389055433250860, 114.7507929638356785, -54.42499999726882720 ) ) ;
#2356 = EDGE_CURVE ( 'NONE', #25435, #8206, #11967, .T. ) ;
#2357 = VERTEX_POINT ( 'NONE', #1173 ) ;
#2358 = CARTESIAN_POINT ( 'NONE',  ( -9.598844408820458085, 35.34453124999998863, -9.598844408820458085 ) ) ;
#2359 = CARTESIAN_POINT ( 'NONE',  ( 5.444914386472302859, 36.03906250108394005, 13.14518615778179189 ) ) ;
#2360 = CARTESIAN_POINT ( 'NONE',  ( 97.92893218813451028, 5.000000000000018652, 2.937500002731185944 ) ) ;
#2361 = CARTESIAN_POINT ( 'NONE',  ( 130.0000000000000000, 37.77539062608393294, 13.14518615778179544 ) ) ;
#2362 = CARTESIAN_POINT ( 'NONE',  ( 59.55508561352770158, 34.84843750108393579, -13.14518615778179900 ) ) ;
#2363 = CARTESIAN_POINT ( 'NONE',  ( 181.8548138422181921, 35.93984375108393436, -5.444914386472297529 ) ) ;
#2364 = ORIENTED_EDGE ( 'NONE', *, *, #3092, .F. ) ;
#2365 = FACE_OUTER_BOUND ( 'NONE', #26834, .T. ) ;
#2366 = CARTESIAN_POINT ( 'NONE',  ( -8.049105076161786076E-16, 33.21132812608393436, -13.14518615778179544 ) ) ;
#2367 = CARTESIAN_POINT ( 'NONE',  ( 131.9473259220810064, 51.47162402671692405, -15.00000000000066258 ) ) ;
#2368 = CARTESIAN_POINT ( 'NONE',  ( 99.99999999999998579, 123.6000000000000085, 2.499999999999978684 ) ) ;
#2369 = CARTESIAN_POINT ( 'NONE',  ( 139.5988444088204403, 40.00781250216787299, -9.598844408820458085 ) ) ;
#2370 = CARTESIAN_POINT ( 'NONE',  ( 1.662435489736055892E-15, 36.00000000000000000, 13.57481594606304576 ) ) ;
#2371 =( BOUNDED_CURVE ( )  B_SPLINE_CURVE ( 2, ( #25636, #23648, #27790, #14928, #4123, #8248, #21506, #27653, #12788, #6119, #19361 ),
 .UNSPECIFIED., .F., .F. ) 
 B_SPLINE_CURVE_WITH_KNOTS ( ( 3, 2, 2, 2, 2, 3 ),
 ( 0.3000000000000002109, 0.3200000000000002287, 0.3400000000000003020, 0.3600000000000002642, 0.3800000000000003375, 0.4000000000000003553 ),
 .UNSPECIFIED. ) 
 CURVE ( )  GEOMETRIC_REPRESENTATION_ITEM ( )  RATIONAL_B_SPLINE_CURVE ( ( 0.9999999999999994449, 0.9510565162951540863, 1.000000000000000000, 0.9510565162951535312, 1.000000000000000000, 0.9510565162951535312, 1.000000000000000000, 0.9510565162951535312, 1.000000000000000000, 0.9510565162951527540, 1.000000000000000888 ) ) 
 REPRESENTATION_ITEM ( '' )  );
#2372 = CARTESIAN_POINT ( 'NONE',  ( -9.598844408820458085, 34.55078124999999289, -9.598844408820458085 ) ) ;
#2373 = EDGE_CURVE ( 'NONE', #2719, #1494, #18964, .T. ) ;
#2374 = CARTESIAN_POINT ( 'NONE',  ( 74.18017581364799184, 55.00000000000000000, 14.99999999999997868 ) ) ;
#2375 = CARTESIAN_POINT ( 'NONE',  ( 58.83893782516223325, 51.27996893917264032, 14.99999999999997868 ) ) ;
#2376 = PRESENTATION_STYLE_ASSIGNMENT (( #90 ) ) ;
#2377 = CARTESIAN_POINT ( 'NONE',  ( 95.54126587499996504, 1.387778780781445676E-14, 8.437500001365592084 ) ) ;
#2378 = ORIENTED_EDGE ( 'NONE', *, *, #5307, .F. ) ;
#2379 = CARTESIAN_POINT ( 'NONE',  ( 97.93301269999999192, 123.8000000010924850, 0.8561741729129329626 ) ) ;
#2380 = CARTESIAN_POINT ( 'NONE',  ( 103.1528011352953342, -3.152801135295355106, 13.81250000136559208 ) ) ;
#2381 = CARTESIAN_POINT ( 'NONE',  ( 130.9830651851037260, 49.99999999949027796, 13.54930971656715677 ) ) ;
#2382 = EDGE_CURVE ( 'NONE', #4458, #28041, #4313, .T. ) ;
#2383 = CARTESIAN_POINT ( 'NONE',  ( -5.444914386472299306, 39.90859375108393436, 13.14518615778179722 ) ) ;
#2384 = CARTESIAN_POINT ( 'NONE',  ( 108.0825317500000153, 110.0000000000000000, -54.25000000273119838 ) ) ;
#2385 = CARTESIAN_POINT ( 'NONE',  ( 101.8468681455906903, 81.37500000136563472, -4.458734125000016313 ) ) ;
#2386 = CARTESIAN_POINT ( 'NONE',  ( 78.14518615778179367, 34.84843750108393579, -5.444914386472297529 ) ) ;
#2387 = CARTESIAN_POINT ( 'NONE',  ( 97.50236033167492167, 102.3130555110000159, -48.72500000273119269 ) ) ;
#2388 = CARTESIAN_POINT ( 'NONE',  ( 9.295050272127046043, 37.87460937608393152, -9.295050272127046043 ) ) ;
#2389 = DIRECTION ( 'NONE',  ( 0.000000000000000000, 1.000000000000000000, 0.000000000000000000 ) ) ;
#2390 = CARTESIAN_POINT ( 'NONE',  ( 107.0000000000000000, 110.0000000000000000, -145.0000000000000284 ) ) ;
#2391 = DIRECTION ( 'NONE',  ( 0.000000000000000000, 1.000000000000000000, 0.000000000000000000 ) ) ;
#2392 = CARTESIAN_POINT ( 'NONE',  ( 124.3771271284221314, 36.08867187500000284, -13.57481594606304753 ) ) ;
#2393 = ADVANCED_FACE ( 'NONE', ( #1446 ), #10279, .T. ) ;
#2394 = ORIENTED_EDGE ( 'NONE', *, *, #2626, .F. ) ;
#2395 = CARTESIAN_POINT ( 'NONE',  ( 95.54126587499996504, 1.387778780781445676E-14, 0.4375000013655920839 ) ) ;
#2396 = CARTESIAN_POINT ( 'NONE',  ( -9.295050272127046043, 38.27148437608393294, -9.295050272127046043 ) ) ;
#2397 = CARTESIAN_POINT ( 'NONE',  ( -8.312177448680279460E-16, 38.51953125216787299, -13.57481594606304576 ) ) ;
#2398 = CARTESIAN_POINT ( 'NONE',  ( 143.1451861577818079, 37.72578125108393721, 5.444914386472293977 ) ) ;
#2399 = PRODUCT ( 'BR-008', 'BR-008', '', ( #200 ) ) ;
#2400 = CARTESIAN_POINT ( 'NONE',  ( 78.57481594606304043, 35.09648437716787583, 5.622872871577869525 ) ) ;
#2401 = DIRECTION ( 'NONE',  ( -0.000000000000000000, -1.000000000000000000, -0.000000000000000000 ) ) ;
#2402 = CARTESIAN_POINT ( 'NONE',  ( -9.295050272127046043, 40.45429687608393721, -9.295050272127046043 ) ) ;
#2403 = CARTESIAN_POINT ( 'NONE',  ( 94.99999999999995737, 1.387778780781445676E-14, 1.999999999999998224 ) ) ;
#2404 = CARTESIAN_POINT ( 'NONE',  ( 108.0825317499999869, 107.3738262389971680, -46.97499999726881015 ) ) ;
#2405 = CARTESIAN_POINT ( 'NONE',  ( 189.5550856135277229, 33.26093750108393721, -13.14518615778179900 ) ) ;
#2406 = CARTESIAN_POINT ( 'NONE',  ( 99.99999999999998579, 90.00000000000000000, -6.938893903907228378E-15 ) ) ;
#2407 = CIRCLE ( 'NONE', #6944, 2.499999999999995115 ) ;
#2408 = CARTESIAN_POINT ( 'NONE',  ( 103.5355339059327235, 93.12500000000000000, -3.535533905932738197 ) ) ;
#2410 = VERTEX_POINT ( 'NONE', #24605 ) ;
#2409 = DIRECTION ( 'NONE',  ( -1.000000000000000000, 0.000000000000000000, -3.469446951953613696E-16 ) ) ;
#2411 = SHAPE_REPRESENTATION ( 'BR-008', ( #27691, #870, #3112, #13099, #19023, #6294, #3589, #21786, #9486, #25867, #9925, #10367, #26322, #19496 ), #22696 ) ;
#2412 = DIRECTION ( 'NONE',  ( -0.8660254037844418162, -0.4999999999999947264, -0.000000000000000000 ) ) ;
#2413 = CARTESIAN_POINT ( 'NONE',  ( -13.57481594606304576, 36.23749999999999005, 0.000000000000000000 ) ) ;
#2414 = LINE ( 'NONE', #11497, #21638 ) ;
#2415 = CARTESIAN_POINT ( 'NONE',  ( -9.295050272127044266, 36.88242187608393152, 9.295050272127047819 ) ) ;
#2416 = CARTESIAN_POINT ( 'NONE',  ( -5.444914386472299306, 35.14609375108393152, 13.14518615778179722 ) ) ;
#2417 = CARTESIAN_POINT ( 'NONE',  ( 189.3771271284221314, 35.29492187500000000, -13.57481594606304753 ) ) ;
#2418 = EDGE_CURVE ( 'NONE', #13118, #24171, #10114, .T. ) ;
#2419 = CARTESIAN_POINT ( 'NONE',  ( 99.99999999999998579, 101.5015231886685712, -44.87500000273119838 ) ) ;
#2420 = CARTESIAN_POINT ( 'NONE',  ( 139.5988444088204687, 36.53515624999999289, 9.598844408820456309 ) ) ;
#2421 = CARTESIAN_POINT ( 'NONE',  ( 70.44491438647230552, 33.95546875108393436, -13.14518615778179900 ) ) ;
#2422 = CARTESIAN_POINT ( 'NONE',  ( 104.4587341249999781, -1.846868145590721655, 1.875000001365591862 ) ) ;
#2423 = CARTESIAN_POINT ( 'NONE',  ( 97.64864547061532107, 122.9999999999999858, 0.8612512827582227137 ) ) ;
#2424 = CARTESIAN_POINT ( 'NONE',  ( 94.99999999999995737, 1.387778780781445676E-14, 4.999999999999999112 ) ) ;
#2425 = CARTESIAN_POINT ( 'NONE',  ( 9.598844408820456309, 37.52734375000000000, -9.598844408820458085 ) ) ;
#2426 = CARTESIAN_POINT ( 'NONE',  ( 116.8548138422182063, 39.21406250108392300, 5.444914386472304635 ) ) ;
#2427 = EDGE_LOOP ( 'NONE', ( #15836, #21135, #8076, #4426 ) ) ;
#2428 = CARTESIAN_POINT ( 'NONE',  ( 104.9999999999999716, 82.50000000000000000, -1.449011120738813565E-14 ) ) ;
#2429 = CARTESIAN_POINT ( 'NONE',  ( 99.99999999999995737, 81.87500000273119838, -5.000000000000018652 ) ) ;
#2430 = CARTESIAN_POINT ( 'NONE',  ( 99.99999999999998579, 94.06249999863440792, 4.458734124999981674 ) ) ;
#2431 = CARTESIAN_POINT ( 'NONE',  ( 52.14049004392254005, 36.00000000000001421, -3.245221471867175023 ) ) ;
#2432 = MECHANICAL_DESIGN_GEOMETRIC_PRESENTATION_REPRESENTATION (  '', ( #17879 ), #7891 ) ;
#2433 = CARTESIAN_POINT ( 'NONE',  ( 94.33688103937534208, 114.1144967660473242, -47.20000000000000995 ) ) ;
#2434 = CARTESIAN_POINT ( 'NONE',  ( 51.42518405393695957, 40.99999999999999289, 0.000000000000000000 ) ) ;
#2435 = VERTEX_POINT ( 'NONE', #20752 ) ;
#2436 = DIRECTION ( 'NONE',  ( 0.000000000000000000, 1.000000000000000000, 0.000000000000000000 ) ) ;
#2437 = CARTESIAN_POINT ( 'NONE',  ( 95.54126587499995082, 1.846868145590750077, 2.625000001365592084 ) ) ;
#2438 = VERTEX_POINT ( 'NONE', #9900 ) ;
#2439 = CARTESIAN_POINT ( 'NONE',  ( -5.444914386472297529, 33.45937500108394147, -13.14518615778179722 ) ) ;
#2440 = CARTESIAN_POINT ( 'NONE',  ( 2.414731522848535132E-15, 39.36289062608393152, 13.14518615778179544 ) ) ;
#2441 = CARTESIAN_POINT ( 'NONE',  ( 204.5988444088204403, 36.03906250216787299, -9.598844408820458085 ) ) ;
#2442 = CARTESIAN_POINT ( 'NONE',  ( 9.295050272127046043, 37.08085937608393579, -9.295050272127046043 ) ) ;
#2443 = LINE ( 'NONE', #24236, #2126 ) ;
#2444 = CARTESIAN_POINT ( 'NONE',  ( 214.9999999999999716, 75.00000000000000000, -10.00000000000000000 ) ) ;
#2445 = CARTESIAN_POINT ( 'NONE',  ( -5.444914386472299306, 35.34453125108393579, 13.14518615778179722 ) ) ;
#2446 = CARTESIAN_POINT ( 'NONE',  ( 139.2950502721270425, 34.69960937608393436, -9.295050272127046043 ) ) ;
#2447 = CARTESIAN_POINT ( 'NONE',  ( 78.57481594606305464, 33.45937499999999432, -1.662435489736055892E-15 ) ) ;
#2448 = FACE_OUTER_BOUND ( 'NONE', #24937, .T. ) ;
#2449 = CARTESIAN_POINT ( 'NONE',  ( 99.99999999999995737, -4.458734124999988779, 12.93750000136559208 ) ) ;
#2450 = FACE_OUTER_BOUND ( 'NONE', #14400, .T. ) ;
#2451 = CARTESIAN_POINT ( 'NONE',  ( 101.8468681455907046, -4.458734124999987891, 13.75000000136559208 ) ) ;
#2452 = CARTESIAN_POINT ( 'NONE',  ( 108.0825317500000011, 112.6261737610028320, -54.02500000273118275 ) ) ;
#2453 = CARTESIAN_POINT ( 'NONE',  ( 99.99999999999998579, 124.0000000000000000, -2.499999999999997780 ) ) ;
#2454 = CARTESIAN_POINT ( 'NONE',  ( 97.50236033167490746, 102.3130555110000159, -49.22499999726882436 ) ) ;
#2455 = CARTESIAN_POINT ( 'NONE',  ( 2.414731522848535132E-15, 35.39414062608393863, 13.14518615778179544 ) ) ;
#2456 = CARTESIAN_POINT ( 'NONE',  ( 97.50236033167490746, 117.6869444889999841, -48.27499999726882152 ) ) ;
#2457 = EDGE_LOOP ( 'NONE', ( #17288, #711, #27032 ) ) ;
#2458 = CARTESIAN_POINT ( 'NONE',  ( 104.3262379212492590, 115.9545556584642867, -51.20000000546237118 ) ) ;
#2459 = FACE_OUTER_BOUND ( 'NONE', #14459, .T. ) ;
#2460 = CARTESIAN_POINT ( 'NONE',  ( 0.000000000000000000, 40.99999999999999289, -13.57481594606304576 ) ) ;
#2461 = EDGE_CURVE ( 'NONE', #9259, #27424, #23781, .T. ) ;
#2462 = CARTESIAN_POINT ( 'NONE',  ( 208.1451861577817795, 37.82500000108392868, -5.444914386472297529 ) ) ;
#2463 = ORIENTED_EDGE ( 'NONE', *, *, #27785, .F. ) ;
#2464 = CARTESIAN_POINT ( 'NONE',  ( 104.9999999999999716, -2.071067811865452857, 7.562500002731185944 ) ) ;
#2465 = CARTESIAN_POINT ( 'NONE',  ( 203.7726092461557812, 50.37415326817817629, -14.99999999999999822 ) ) ;
#2466 = CARTESIAN_POINT ( 'NONE',  ( 98.15313185440925281, 4.458734125000016313, 13.50000000136559208 ) ) ;
#2467 = EDGE_LOOP ( 'NONE', ( #15603, #6608, #7902, #4181 ) ) ;
#2468 = CARTESIAN_POINT ( 'NONE',  ( 94.33688103937537051, 114.1144967660473242, -52.20000000000000995 ) ) ;
#2469 = CARTESIAN_POINT ( 'NONE',  ( 13.57481594606304576, 33.55859375216787299, -1.662435489736055892E-15 ) ) ;
#2470 = CARTESIAN_POINT ( 'NONE',  ( 101.0355339059327378, 124.4500000000000028, 2.499999999999977796 ) ) ;
#2471 = CARTESIAN_POINT ( 'NONE',  ( 139.2950502721270425, 40.05742187608392868, 9.295050272127046043 ) ) ;
#2472 = CARTESIAN_POINT ( 'NONE',  ( 0.000000000000000000, 36.00000000000000000, -13.57481594606304576 ) ) ;
#2473 = CARTESIAN_POINT ( 'NONE',  ( 95.00000000000000000, 94.31249999726880162, -2.071067811865479058 ) ) ;
#2474 = CARTESIAN_POINT ( 'NONE',  ( 74.29505027212704249, 38.07304687608393579, -9.295050272127046043 ) ) ;
#2475 = CARTESIAN_POINT ( 'NONE',  ( 13.57481594606304576, 37.42812499999999432, -1.662435489736055892E-15 ) ) ;
#2476 = CARTESIAN_POINT ( 'NONE',  ( 200.4449143864723055, 36.23750000108393721, 13.14518615778179189 ) ) ;
#2477 = CARTESIAN_POINT ( 'NONE',  ( 102.4999999999999858, 123.1500000021849672, -1.035533905932742638 ) ) ;
#2478 = ORIENTED_EDGE ( 'NONE', *, *, #24239, .T. ) ;
#2479 = CARTESIAN_POINT ( 'NONE',  ( -5.444914386472297529, 39.80937500108392868, -13.14518615778179900 ) ) ;
#2480 = APPLICATION_PROTOCOL_DEFINITION ( 'draft international standard', 'automotive_design', 1998, #4974 ) ;
#2481 = CARTESIAN_POINT ( 'NONE',  ( 104.4587341249999639, 1.442382525525748735E-14, 9.187500001365592084 ) ) ;
#2482 =( BOUNDED_CURVE ( )  B_SPLINE_CURVE ( 2, ( #20922, #23059, #27618, #3809, #6224, #16771, #25328, #12469, #10336 ),
 .UNSPECIFIED., .F., .F. ) 
 B_SPLINE_CURVE_WITH_KNOTS ( ( 3, 2, 2, 2, 3 ),
 ( 0.8124999999999998890, 0.8229166666666666297, 0.8333333333333334814, 0.8437500000000003331, 0.8541666666666670737 ),
 .UNSPECIFIED. ) 
 CURVE ( )  GEOMETRIC_REPRESENTATION_ITEM ( )  RATIONAL_B_SPLINE_CURVE ( ( 1.000000000000000888, 0.9238795325112859613, 1.000000000000000000, 0.9238795325112867385, 1.000000000000000000, 0.9238795325112867385, 1.000000000000000000, 0.9238795325112835188, 1.000000000000003331 ) ) 
 REPRESENTATION_ITEM ( '' )  );
#2483 = CARTESIAN_POINT ( 'NONE',  ( 65.00000000000000000, 39.95820312608393010, 13.14518615778179544 ) ) ;
#2484 = CARTESIAN_POINT ( 'NONE',  ( 96.84719886470459471, 79.56250000136559208, 3.152801135295355994 ) ) ;
#2485 = CARTESIAN_POINT ( 'NONE',  ( 185.7049497278729575, 40.45429687608393721, -9.295050272127046043 ) ) ;
#2486 = CARTESIAN_POINT ( 'NONE',  ( -13.14518615778179722, 38.32109375108394289, -5.444914386472297529 ) ) ;
#2487 = PLANE ( 'NONE',  #359 ) ;
#2488 = CARTESIAN_POINT ( 'NONE',  ( 102.0710678118654329, -4.999999999999989342, 12.31249999999999822 ) ) ;
#2489 = CARTESIAN_POINT ( 'NONE',  ( 78.57481594606305464, 39.80937499999999574, -1.662435489736055892E-15 ) ) ;
#2490 = CARTESIAN_POINT ( 'NONE',  ( 91.91746824999997045, 112.6261737610028320, -51.72499999726882436 ) ) ;
#2491 = ORIENTED_EDGE ( 'NONE', *, *, #25266, .F. ) ;
#2492 = ORIENTED_EDGE ( 'NONE', *, *, #12484, .F. ) ;
#2493 = CARTESIAN_POINT ( 'NONE',  ( -5.622872871577873077, 36.08867187500000284, -13.57481594606304753 ) ) ;
#2494 = CARTESIAN_POINT ( 'NONE',  ( -8.049105076161786076E-16, 35.59257812608393579, -13.14518615778179544 ) ) ;
#2495 = ORIENTED_EDGE ( 'NONE', *, *, #12780, .F. ) ;
#2496 = CARTESIAN_POINT ( 'NONE',  ( 120.7049497278729575, 32.11992187608393579, 9.295050272127047819 ) ) ;
#2497 = CARTESIAN_POINT ( 'NONE',  ( 59.55508561352770158, 35.14609375108393152, 13.14518615778179722 ) ) ;
#2498 = CARTESIAN_POINT ( 'NONE',  ( 200.4449143864723055, 36.23750000108393721, 13.14518615778179189 ) ) ;
#2499 = ADVANCED_FACE ( 'NONE', ( #11466 ), #20185, .T. ) ;
#2500 = EDGE_LOOP ( 'NONE', ( #23716, #19526, #11070, #26522 ) ) ;
#2501 = CARTESIAN_POINT ( 'NONE',  ( 87.00000000000000000, 118.0000000000000000, -13.00000000000000711 ) ) ;
#2502 = CARTESIAN_POINT ( 'NONE',  ( 9.295050272127047819, 32.11992187608393579, 9.295050272127046043 ) ) ;
#2503 = CARTESIAN_POINT ( 'NONE',  ( 129.6030005853479850, 51.45716825712189291, -15.00000000000033573 ) ) ;
#2504 = CARTESIAN_POINT ( 'NONE',  ( 99.99999999999998579, 124.7999999999999972, -2.499999999999997780 ) ) ;
#2505 = CARTESIAN_POINT ( 'NONE',  ( 91.91746824999998466, 107.3738262389971680, -53.02500000273119696 ) ) ;
#2506 = CARTESIAN_POINT ( 'NONE',  ( 199.1572863549628210, 35.99999999999999289, -12.92256159328821141 ) ) ;
#2507 = CARTESIAN_POINT ( 'NONE',  ( 102.4999999999999716, 122.3500000021849701, -1.035533905932742638 ) ) ;
#2508 = CARTESIAN_POINT ( 'NONE',  ( -13.57481594606304398, 36.38632812716788578, 5.622872871577880183 ) ) ;
#2509 = AXIS2_PLACEMENT_3D ( 'NONE', #4496, #13154, #21892 ) ;
#2510 = ORIENTED_EDGE ( 'NONE', *, *, #19041, .T. ) ;
#2511 = CARTESIAN_POINT ( 'NONE',  ( 104.4587341249999639, 1.442382525525748735E-14, 7.937500001365592084 ) ) ;
#2512 = EDGE_LOOP ( 'NONE', ( #26472, #17277, #3650, #10533 ) ) ;
#2513 = CARTESIAN_POINT ( 'NONE',  ( 98.53841926354351699, 123.6500000010924794, -1.461580736456474794 ) ) ;
#2514 = CARTESIAN_POINT ( 'NONE',  ( 98.15313185440925281, -4.458734124999987891, 11.62500000136559031 ) ) ;
#2515 = CARTESIAN_POINT ( 'NONE',  ( 124.6345034319466691, 54.48174559708144926, 14.99999999999996803 ) ) ;
#2516 = CARTESIAN_POINT ( 'NONE',  ( 2.414731522848535132E-15, 37.57695312608392868, 13.14518615778179544 ) ) ;
#2517 = DIRECTION ( 'NONE',  ( 0.000000000000000000, 1.000000000000000000, 0.000000000000000000 ) ) ;
#2518 = CARTESIAN_POINT ( 'NONE',  ( 104.4587341249999781, 82.25000000136559208, -1.846868145590750299 ) ) ;
#2519 = CARTESIAN_POINT ( 'NONE',  ( 51.85481384221820633, 35.24531250108393721, 5.444914386472304635 ) ) ;
#2520 = EDGE_CURVE ( 'NONE', #2344, #26363, #3502, .T. ) ;
#2521 = CARTESIAN_POINT ( 'NONE',  ( 108.0825317500000011, 107.3738262389971538, -44.47500000273118559 ) ) ;
#2522 = CARTESIAN_POINT ( 'NONE',  ( 2.414731522848535132E-15, 39.16445312608392726, 13.14518615778179544 ) ) ;
#2523 = CARTESIAN_POINT ( 'NONE',  ( -8.312177448680279460E-16, 39.21406249999999716, -13.57481594606304576 ) ) ;
#2524 = LINE ( 'NONE', #241, #1328 ) ;
#2525 = CARTESIAN_POINT ( 'NONE',  ( 99.99999999999995737, 82.25000000000000000, 4.999999999999990230 ) ) ;
#2526 = CARTESIAN_POINT ( 'NONE',  ( 120.4011555911795455, 37.92421874999999432, 9.598844408820459861 ) ) ;
#2527 = VERTEX_POINT ( 'NONE', #6195 ) ;
#2528 = ORIENTED_EDGE ( 'NONE', *, *, #17246, .T. ) ;
#2529 = CARTESIAN_POINT ( 'NONE',  ( 13.57481594606304753, 33.50898437499999716, -5.622872871577873966 ) ) ;
#2530 = CARTESIAN_POINT ( 'NONE',  ( -13.14518615778179189, 36.03906250108394005, 5.444914386472304635 ) ) ;
#2531 = CARTESIAN_POINT ( 'NONE',  ( -5.622872871577873077, 37.77539062716788010, -13.57481594606304753 ) ) ;
#2532 = CARTESIAN_POINT ( 'NONE',  ( 99.99999999999995737, -4.999999999999990230, 9.375000002731184168 ) ) ;
#2533 = CARTESIAN_POINT ( 'NONE',  ( 120.7049497278729575, 35.69179687608393436, -9.295050272127046043 ) ) ;
#2534 = ADVANCED_FACE ( 'NONE', ( #10595 ), #21164, .F. ) ;
#2535 = CARTESIAN_POINT ( 'NONE',  ( 51.42518405393695957, 33.95546875216787441, 0.000000000000000000 ) ) ;
#2536 = EDGE_CURVE ( 'NONE', #13023, #4040, #19160, .T. ) ;
#2537 = ORIENTED_EDGE ( 'NONE', *, *, #17851, .F. ) ;
#2538 =( BOUNDED_CURVE ( )  B_SPLINE_CURVE ( 2, ( #25619, #18520, #9945, #23352, #12629, #3692, #3969, #25347, #14361 ),
 .UNSPECIFIED., .F., .F. ) 
 B_SPLINE_CURVE_WITH_KNOTS ( ( 3, 2, 2, 2, 3 ),
 ( 0.4999999999999998890, 0.5089285714285712858, 0.5178571428571427937, 0.5267857142857143016, 0.5357142857142856984 ),
 .UNSPECIFIED. ) 
 CURVE ( )  GEOMETRIC_REPRESENTATION_ITEM ( )  RATIONAL_B_SPLINE_CURVE ( ( 1.000000000000000888, 0.9238795325112857393, 1.000000000000000000, 0.9238795325112867385, 1.000000000000000000, 0.9238795325112867385, 1.000000000000000000, 0.9238795325112867385, 1.000000000000000000 ) ) 
 REPRESENTATION_ITEM ( '' )  );
#2539 = AXIS2_PLACEMENT_3D ( 'NONE', #8020, #8434, #3890 ) ;
#2540 = CARTESIAN_POINT ( 'NONE',  ( 13.49550141231711287, 36.00000000000000711, -0.9550757908102345262 ) ) ;
#2541 = CARTESIAN_POINT ( 'NONE',  ( -5.622872871577873077, 33.01289062716787726, -13.57481594606304753 ) ) ;
#2542 = EDGE_CURVE ( 'NONE', #9045, #28041, #7908, .T. ) ;
#2543 = CARTESIAN_POINT ( 'NONE',  ( 99.99999999999998579, 123.7000000021849502, 2.499999999999978684 ) ) ;
#2544 = CARTESIAN_POINT ( 'NONE',  ( 91.91746824999998466, 110.0000000000000000, -49.87499999726882294 ) ) ;
#2545 = CARTESIAN_POINT ( 'NONE',  ( 189.5550856135277229, 34.84843750108393579, -13.14518615778179900 ) ) ;
#2546 = VECTOR ( 'NONE', #16546, 1000.000000000000000 ) ;
#2547 = EDGE_CURVE ( 'NONE', #7547, #15121, #21253, .T. ) ;
#2548 = CARTESIAN_POINT ( 'NONE',  ( 13.57481594606304576, 34.35234375216787583, -1.662435489736055892E-15 ) ) ;
#2549 = DIRECTION ( 'NONE',  ( -1.000000000000000000, 0.000000000000000000, 0.000000000000000000 ) ) ;
#2550 = DIRECTION ( 'NONE',  ( -0.8660254037844380415, 0.5000000000000013323, 0.000000000000000000 ) ) ;
#2551 = CARTESIAN_POINT ( 'NONE',  ( -5.622872871577828668, 32.51679687716787015, 13.57481594606309194 ) ) ;
#2552 = CARTESIAN_POINT ( 'NONE',  ( -9.598844408820458085, 36.13828124999999147, -9.598844408820458085 ) ) ;
#2553 = DIRECTION ( 'NONE',  ( -0.000000000000000000, -1.000000000000000000, -0.000000000000000000 ) ) ;
#2554 = CARTESIAN_POINT ( 'NONE',  ( 13.14518615778179900, 37.22968750108393721, -5.444914386472297529 ) ) ;
#2555 = CARTESIAN_POINT ( 'NONE',  ( 9.295050272127047819, 37.67617187608393436, 9.295050272127046043 ) ) ;
#2556 = CARTESIAN_POINT ( 'NONE',  ( 185.4011555911795313, 33.75703124999999005, -9.598844408820458085 ) ) ;
#2557 = CARTESIAN_POINT ( 'NONE',  ( 91.91746824999998466, 107.3738262389971680, -47.27500000273118985 ) ) ;
#2558 = CARTESIAN_POINT ( 'NONE',  ( 107.0000000000000142, 110.0000000000000000, -45.50000000546238255 ) ) ;
#2559 = CARTESIAN_POINT ( 'NONE',  ( 65.00000000000000000, 35.19570312608392726, 13.14518615778179544 ) ) ;
#2560 = CARTESIAN_POINT ( 'NONE',  ( 104.4587341249999781, -1.846868145590721655, 3.875000001365591640 ) ) ;
#2561 = CARTESIAN_POINT ( 'NONE',  ( 97.80124048048590168, 123.0000000000000142, -1.224358067407148587 ) ) ;
#2562 = LINE ( 'NONE', #15654, #15728 ) ;
#2563 = CARTESIAN_POINT ( 'NONE',  ( -5.622872871577873077, 36.08867187500000284, -13.57481594606304753 ) ) ;
#2564 = CARTESIAN_POINT ( 'NONE',  ( 139.2950502721270425, 38.86679687608393863, -9.295050272127046043 ) ) ;
#2565 = EDGE_CURVE ( 'NONE', #15436, #20385, #18866, .T. ) ;
#2566 = EDGE_LOOP ( 'NONE', ( #21580, #13791, #18482, #26653 ) ) ;
#2567 = CARTESIAN_POINT ( 'NONE',  ( 104.9999999999999716, 84.50000000000000000, -1.449011120738813565E-14 ) ) ;
#2568 = CARTESIAN_POINT ( 'NONE',  ( 13.57481594606304931, 34.99726562500000426, 5.622872871577868636 ) ) ;
#2569 = CARTESIAN_POINT ( 'NONE',  ( 96.46446609406721961, 84.00000000273119838, -3.535533905932755072 ) ) ;
#2570 = AXIS2_PLACEMENT_3D ( 'NONE', #21626, #19619, #4236 ) ;
#2571 = CARTESIAN_POINT ( 'NONE',  ( 101.8468681455907330, 94.49999999863442213, -4.458734124999994997 ) ) ;
#2572 = CARTESIAN_POINT ( 'NONE',  ( 60.02711226049118665, 36.00000000000001421, -12.48139679469878871 ) ) ;
#2573 = EDGE_CURVE ( 'NONE', #3340, #28009, #14451, .T. ) ;
#2574 = CARTESIAN_POINT ( 'NONE',  ( 99.99999999999997158, 117.3602355696678501, -51.50000000000001421 ) ) ;
#2575 = CARTESIAN_POINT ( 'NONE',  ( 78.14518615778179367, 33.21132812608393436, -1.609821015232357215E-15 ) ) ;
#2576 = ORIENTED_EDGE ( 'NONE', *, *, #6335, .F. ) ;
#2577 =( BOUNDED_CURVE ( )  B_SPLINE_CURVE ( 2, ( #13774, #22212, #20358, #26925, #7084, #3255, #11781 ),
 .UNSPECIFIED., .F., .T. ) 
 B_SPLINE_CURVE_WITH_KNOTS ( ( 3, 2, 2, 3 ),
 ( 0.4166666666666666297, 0.4583333333333332593, 0.5000000000000000000, 0.5416666676520737189 ),
 .UNSPECIFIED. ) 
 CURVE ( )  GEOMETRIC_REPRESENTATION_ITEM ( )  RATIONAL_B_SPLINE_CURVE ( ( 1.000000000000000000, 0.9238795325112866275, 1.000000000000000000, 0.9238795325112867385, 1.000000000000000000, 0.9238795325112867385, 1.000000000000000000 ) ) 
 REPRESENTATION_ITEM ( '' )  );
#2578 = CYLINDRICAL_SURFACE ( 'NONE', #19038, 5.000000000000004441 ) ;
#2579 = ADVANCED_FACE ( 'NONE', ( #27726 ), #25713, .F. ) ;
#2580 = CARTESIAN_POINT ( 'NONE',  ( 99.99999999999995737, 5.000000000000018652, 13.75000000000000000 ) ) ;
#2581 = VERTEX_POINT ( 'NONE', #10035 ) ;
#2582 = CARTESIAN_POINT ( 'NONE',  ( 2.414731522848535132E-15, 40.15664062608393436, 13.14518615778179544 ) ) ;
#2583 = CARTESIAN_POINT ( 'NONE',  ( 185.4011555911795597, 33.26093750216787726, 9.598844408820459861 ) ) ;
#2584 = VECTOR ( 'NONE', #16967, 1000.000000000000000 ) ;
#2585 = CARTESIAN_POINT ( 'NONE',  ( 5.444914386472297529, 35.54296875108393294, -13.14518615778179722 ) ) ;
#2586 = CARTESIAN_POINT ( 'NONE',  ( 55.81982418635200816, 55.00000000000000000, -14.99999999999999822 ) ) ;
#2587 = CARTESIAN_POINT ( 'NONE',  ( 204.5988444088204403, 38.42031250216787441, -9.598844408820458085 ) ) ;
#2588 = CARTESIAN_POINT ( 'NONE',  ( 5.444914386472302859, 36.23750000108393721, 13.14518615778179189 ) ) ;
#2589 = CARTESIAN_POINT ( 'NONE',  ( 143.1451861577818079, 36.23750000108393010, -5.444914386472297529 ) ) ;
#2590 = CARTESIAN_POINT ( 'NONE',  ( 55.40115559117954547, 35.54296874999999289, 9.598844408820459861 ) ) ;
#2591 = AXIS2_PLACEMENT_3D ( 'NONE', #24762, #11485, #17780 ) ;
#2592 = CARTESIAN_POINT ( 'NONE',  ( 104.9999999999999858, 92.00000000000000000, -6.938893903907228378E-15 ) ) ;
#2593 = CARTESIAN_POINT ( 'NONE',  ( 95.54126587499996504, 1.387778780781445676E-14, 12.68750000136559208 ) ) ;
#2594 = CARTESIAN_POINT ( 'NONE',  ( 195.0000000000000000, -7.395377635281828788, -2.255140518769849538E-14 ) ) ;
#2595 = CARTESIAN_POINT ( 'NONE',  ( 99.99999999999995737, 4.458734125000016313, 12.18750000136559208 ) ) ;
#2596 = CARTESIAN_POINT ( 'NONE',  ( 108.0825317500000011, 107.3738262389971538, -46.22500000273118559 ) ) ;
#2597 = CARTESIAN_POINT ( 'NONE',  ( 99.99999999999998579, 123.6000000000000085, 2.499999999999978684 ) ) ;
#2598 = DIRECTION ( 'NONE',  ( 0.000000000000000000, -1.000000000000000000, 0.000000000000000000 ) ) ;
#2599 = CARTESIAN_POINT ( 'NONE',  ( 104.9952793366501567, 116.8754121666685393, -48.32499999726882578 ) ) ;
#2600 = CARTESIAN_POINT ( 'NONE',  ( 9.295050272127047819, 36.28710937608393294, 9.295050272127046043 ) ) ;
#2601 = CARTESIAN_POINT ( 'NONE',  ( 95.67376207875069838, 104.0454443415356991, -48.19999999453764161 ) ) ;
#2602 = ORIENTED_EDGE ( 'NONE', *, *, #1788, .F. ) ;
#2603 = DIRECTION ( 'NONE',  ( -0.000000000000000000, 1.000000000000000000, -0.000000000000000000 ) ) ;
#2604 = CARTESIAN_POINT ( 'NONE',  ( 99.99999999999998579, 122.7500000010924879, -2.066987299999998751 ) ) ;
#2605 = DIRECTION ( 'NONE',  ( -0.8660254037844418162, 0.4999999999999947264, 0.000000000000000000 ) ) ;
#2606 = CARTESIAN_POINT ( 'NONE',  ( 181.8548138422181921, 37.32890625108393579, -5.444914386472297529 ) ) ;
#2607 = ORIENTED_EDGE ( 'NONE', *, *, #18989, .F. ) ;
#2608 = CARTESIAN_POINT ( 'NONE',  ( 195.8421075954646255, 53.50112910130381749, -15.00000000000000178 ) ) ;
#2609 = CARTESIAN_POINT ( 'NONE',  ( 99.99999999999995737, 4.458734125000016313, 11.43750000136559208 ) ) ;
#2610 = ORIENTED_EDGE ( 'NONE', *, *, #10957, .F. ) ;
#2611 = CARTESIAN_POINT ( 'NONE',  ( 93.00000000000001421, 112.2744378736303332, -46.10000000000000142 ) ) ;
#2612 = CARTESIAN_POINT ( 'NONE',  ( -8.049105076161786076E-16, 40.35507812608393152, -13.14518615778179544 ) ) ;
#2613 = CARTESIAN_POINT ( 'NONE',  ( 101.7677669529663547, 123.8999999999999915, -1.767766952966370209 ) ) ;
#2614 = CARTESIAN_POINT ( 'NONE',  ( 124.3771271284221314, 32.51679687716787726, 13.57481594606304753 ) ) ;
#2615 = CARTESIAN_POINT ( 'NONE',  ( -9.295050272127046043, 39.85898437608393152, -9.295050272127046043 ) ) ;
#2616 =( BOUNDED_CURVE ( )  B_SPLINE_CURVE ( 2, ( #27650, #12227, #1577, #16390, #1165, #1024, #16532, #27101, #1438 ),
 .UNSPECIFIED., .F., .T. ) 
 B_SPLINE_CURVE_WITH_KNOTS ( ( 3, 2, 2, 2, 3 ),
 ( 0.2500000000000004441, 0.2916666666666670182, 0.3333333333333334814, 0.3750000000000000555, 0.4166666666666666297 ),
 .UNSPECIFIED. ) 
 CURVE ( )  GEOMETRIC_REPRESENTATION_ITEM ( )  RATIONAL_B_SPLINE_CURVE ( ( 0.9999999999999992228, 0.9238795325112875156, 1.000000000000000000, 0.9238795325112867385, 1.000000000000000000, 0.9238795325112867385, 1.000000000000000000, 0.9238795325112868495, 0.9999999999999998890 ) ) 
 REPRESENTATION_ITEM ( '' )  );
#2617 = CARTESIAN_POINT ( 'NONE',  ( 96.46446609406726225, 93.24999999726881583, -3.535533905932738197 ) ) ;
#2618 = CARTESIAN_POINT ( 'NONE',  ( 59.55508561352770158, 37.72578125108395142, 13.14518615778179722 ) ) ;
#2619 = CARTESIAN_POINT ( 'NONE',  ( 68.86392526511711765, 54.10645156200380512, -15.00000000000000000 ) ) ;
#2620 = CARTESIAN_POINT ( 'NONE',  ( 200.6228728715778686, 40.75195312500000711, -13.57481594606304753 ) ) ;
#2621 = VERTEX_POINT ( 'NONE', #25441 ) ;
#2622 = CARTESIAN_POINT ( 'NONE',  ( 74.59884440882045453, 38.32109374999999574, -9.598844408820458085 ) ) ;
#2623 = ORIENTED_EDGE ( 'NONE', *, *, #44, .T. ) ;
#2624 = ORIENTED_EDGE ( 'NONE', *, *, #15897, .T. ) ;
#2625 = CARTESIAN_POINT ( 'NONE',  ( -13.14518615778179544, 35.19570312608393436, 0.000000000000000000 ) ) ;
#2626 = EDGE_CURVE ( 'NONE', #499, #9571, #1691, .T. ) ;
#2627 = CARTESIAN_POINT ( 'NONE',  ( 104.4587341249999781, 1.846868145590750521, 12.25000000136559208 ) ) ;
#2628 = CARTESIAN_POINT ( 'NONE',  ( 55.70494972787295751, 38.86679687608393863, -9.295050272127046043 ) ) ;
#2629 = DIRECTION ( 'NONE',  ( 0.000000000000000000, 1.000000000000000000, -1.156482317317871478E-16 ) ) ;
#2630 = CARTESIAN_POINT ( 'NONE',  ( 204.2950502721270425, 37.67617187608393436, 9.295050272127046043 ) ) ;
#2631 = EDGE_LOOP ( 'NONE', ( #21780, #2090, #21677 ) ) ;
#2632 = CARTESIAN_POINT ( 'NONE',  ( 5.444914386472297529, 38.91640625108393436, -13.14518615778179722 ) ) ;
#2633 = CARTESIAN_POINT ( 'NONE',  ( 104.4587341249999923, 91.49999999863440792, 1.846868145590726318 ) ) ;
#2634 = CARTESIAN_POINT ( 'NONE',  ( 200.4449143864723055, 38.12265625108393863, -13.14518615778179722 ) ) ;
#2635 = CARTESIAN_POINT ( 'NONE',  ( 99.99999999999997158, 101.5015231886685854, -55.12499999726880873 ) ) ;
#2636 = ORIENTED_EDGE ( 'NONE', *, *, #16630, .F. ) ;
#2637 = CARTESIAN_POINT ( 'NONE',  ( 13.57481594606304931, 37.37851562499999858, 5.622872871577869525 ) ) ;
#2638 = CARTESIAN_POINT ( 'NONE',  ( 13.14518615778179900, 36.93203125108394147, 5.444914386472293977 ) ) ;
#2639 = EDGE_LOOP ( 'NONE', ( #2576, #13038, #22128 ) ) ;
#2640 = CARTESIAN_POINT ( 'NONE',  ( 120.7049497278729575, 32.71523437608393436, -9.295050272127046043 ) ) ;
#2641 = CARTESIAN_POINT ( 'NONE',  ( 78.14518615778179367, 33.06250000108393294, -5.444914386472297529 ) ) ;
#2642 = CARTESIAN_POINT ( 'NONE',  ( 195.0000000000000000, 36.98164062608393721, 13.14518615778179544 ) ) ;
#2643 = ORIENTED_EDGE ( 'NONE', *, *, #479, .T. ) ;
#2644 = CARTESIAN_POINT ( 'NONE',  ( 97.93301270000000613, 123.7000000010924765, -0.8561741729129506151 ) ) ;
#2645 = CARTESIAN_POINT ( 'NONE',  ( 9.295050272127047819, 33.70742187608393436, 9.295050272127046043 ) ) ;
#2646 = CARTESIAN_POINT ( 'NONE',  ( 99.99999999999998579, 123.7000000021849502, 2.499999999999978684 ) ) ;
#2647 = CARTESIAN_POINT ( 'NONE',  ( 120.4011555911795455, 39.41250000216787441, -9.598844408820458085 ) ) ;
#2648 = CARTESIAN_POINT ( 'NONE',  ( 97.50236033167492167, 102.3130555110000159, -52.72500000273119980 ) ) ;
#2649 = LINE ( 'NONE', #4930, #20620 ) ;
#2650 = LINE ( 'NONE', #24876, #1888 ) ;
#2651 = CARTESIAN_POINT ( 'NONE',  ( 71.87350824357694989, 51.14166184781134206, 15.00000000000195222 ) ) ;
#2652 = PRODUCT_DEFINITION ( 'UNKNOWN', '', #23155, #1521 ) ;
#2653 = EDGE_CURVE ( 'NONE', #8637, #10079, #11194, .T. ) ;
#2654 = EDGE_LOOP ( 'NONE', ( #25934, #10017, #11980, #12718 ) ) ;
#2655 = CARTESIAN_POINT ( 'NONE',  ( 104.4587341249999781, -1.846868145590721655, 3.875000001365592084 ) ) ;
#2656 = ORIENTED_EDGE ( 'NONE', *, *, #84, .F. ) ;
#2657 = CARTESIAN_POINT ( 'NONE',  ( 101.4615807364564546, 124.2500000010924879, -1.461580736456474794 ) ) ;
#2658 = CARTESIAN_POINT ( 'NONE',  ( 104.4587341249999639, 1.442382525525748735E-14, 6.937500001365592972 ) ) ;
#2659 = CARTESIAN_POINT ( 'NONE',  ( 51.42518405393695957, 37.87460937716787868, -5.622872871577872189 ) ) ;
#2660 = VECTOR ( 'NONE', #560, 1000.000000000000000 ) ;
#2661 = CARTESIAN_POINT ( 'NONE',  ( 9.295050272127047819, 36.88242187608393152, 9.295050272127046043 ) ) ;
#2662 = CARTESIAN_POINT ( 'NONE',  ( -13.57481594606304576, 38.71796875216787726, 0.000000000000000000 ) ) ;
#2663 = CARTESIAN_POINT ( 'NONE',  ( 101.8468681455906903, 81.00000000136560629, 4.458734124999987891 ) ) ;
#2664 = CARTESIAN_POINT ( 'NONE',  ( 51.85481384221819923, 35.93984375108393436, -5.444914386472297529 ) ) ;
#2665 = CARTESIAN_POINT ( 'NONE',  ( 102.4976396683250925, 117.6869444889999841, -45.72500000273119269 ) ) ;
#2666 = CARTESIAN_POINT ( 'NONE',  ( -13.14518615778179189, 38.22187500108393721, 5.444914386472304635 ) ) ;
#2667 = CARTESIAN_POINT ( 'NONE',  ( -13.57481594606304576, 37.87460937499999147, 5.622872871577880183 ) ) ;
#2668 = CARTESIAN_POINT ( 'NONE',  ( 6.119843627700378264, 51.28708186914656153, 14.99999999999999645 ) ) ;
#2669 = CARTESIAN_POINT ( 'NONE',  ( 104.9999999999999716, 1.449011120738813565E-14, 7.500000000000000000 ) ) ;
#2670 = CARTESIAN_POINT ( 'NONE',  ( 130.0000000000000000, 38.42031249999999432, -13.57481594606304576 ) ) ;
#2671 = ORIENTED_EDGE ( 'NONE', *, *, #23773, .T. ) ;
#2672 = ORIENTED_EDGE ( 'NONE', *, *, #14123, .F. ) ;
#2673 = DIRECTION ( 'NONE',  ( 0.000000000000000000, 0.000000000000000000, -1.000000000000000000 ) ) ;
#2674 = CARTESIAN_POINT ( 'NONE',  ( 13.14518615778179900, 37.22968750108393721, -5.444914386472297529 ) ) ;
#2675 = CARTESIAN_POINT ( 'NONE',  ( 9.598844408820456309, 38.42031250216787441, -9.598844408820458085 ) ) ;
#2676 = CARTESIAN_POINT ( 'NONE',  ( 97.92893218813451028, -4.999999999999989342, 11.31250000273118594 ) ) ;
#2677 = CARTESIAN_POINT ( 'NONE',  ( 116.8548138422182205, 34.99726562608393721, 0.000000000000000000 ) ) ;
#2678 = CARTESIAN_POINT ( 'NONE',  ( 78.57481594606304043, 33.50898437716787015, 5.622872871577869525 ) ) ;
#2679 = CARTESIAN_POINT ( 'NONE',  ( -13.57481594606304753, 31.52460937716787370, -5.622872871577873077 ) ) ;
#2680 = CIRCLE ( 'NONE', #16323, 11.57481594606304398 ) ;
#2681 = VECTOR ( 'NONE', #18208, 1000.000000000000000 ) ;
#2682 = CARTESIAN_POINT ( 'NONE',  ( 104.9999999999999574, -2.071067811865462627, 2.437499999999998668 ) ) ;
#2683 = CARTESIAN_POINT ( 'NONE',  ( 0.000000000000000000, 20.53589838486225361, 0.000000000000000000 ) ) ;
#2684 = FACE_OUTER_BOUND ( 'NONE', #18957, .T. ) ;
#2685 = AXIS2_PLACEMENT_3D ( 'NONE', #17965, #26674, #7121 ) ;
#2686 = CARTESIAN_POINT ( 'NONE',  ( 208.1451861577818079, 33.01289062608393010, -1.609821015232357215E-15 ) ) ;
#2687 = DIRECTION ( 'NONE',  ( -0.000000000000000000, 1.000000000000000000, -0.000000000000000000 ) ) ;
#2688 = CARTESIAN_POINT ( 'NONE',  ( 99.99999999999998579, 124.3500000010924822, -2.066987299999998751 ) ) ;
#2689 = CARTESIAN_POINT ( 'NONE',  ( 130.0000000000000000, 39.31328125216787583, -13.57481594606304576 ) ) ;
#2690 = DIRECTION ( 'NONE',  ( -0.000000000000000000, -0.000000000000000000, -1.000000000000000000 ) ) ;
#2691 = CARTESIAN_POINT ( 'NONE',  ( 96.46446609406721961, 3.535533905932755072, 12.87500000000000000 ) ) ;
#2692 = CARTESIAN_POINT ( 'NONE',  ( 9.598844408820456309, 37.52734375000000000, -9.598844408820458085 ) ) ;
#2693 = CARTESIAN_POINT ( 'NONE',  ( 3.089260913797906571, 36.00000000000000000, -13.21136010216355672 ) ) ;
#2694 = CARTESIAN_POINT ( 'NONE',  ( 5.444914386472302859, 33.06250000108393294, 13.14518615778179189 ) ) ;
#2695 = CARTESIAN_POINT ( 'NONE',  ( -8.049105076161786076E-16, 35.59257812608393579, -13.14518615778179544 ) ) ;
#2696 = ADVANCED_FACE ( 'NONE', ( #12164, #25295 ), #20892, .F. ) ;
#2697 = CARTESIAN_POINT ( 'NONE',  ( 200.6228728715778686, 34.89804687499999147, 13.57481594606304576 ) ) ;
#2698 = CARTESIAN_POINT ( 'NONE',  ( -9.598844408820454532, 36.43593750216787441, 9.598844408820459861 ) ) ;
#2699 = CARTESIAN_POINT ( 'NONE',  ( 99.99999999999995737, -4.999999999999990230, 4.375000002731185056 ) ) ;
#2700 = CARTESIAN_POINT ( 'NONE',  ( 143.5748159460630688, 36.68398437500000142, -5.622872871577873966 ) ) ;
#2701 = CARTESIAN_POINT ( 'NONE',  ( 70.44491438647230552, 36.33671875108394289, -13.14518615778179900 ) ) ;
#2702 = EDGE_CURVE ( 'NONE', #4367, #24513, #21664, .T. ) ;
#2703 = CARTESIAN_POINT ( 'NONE',  ( 95.54126587499996504, 1.846868145590750077, 3.375000001365592972 ) ) ;
#2704 = CARTESIAN_POINT ( 'NONE',  ( 99.99999999999998579, 137.0000000000000000, -12.50000000000002132 ) ) ;
#2705 = ORIENTED_EDGE ( 'NONE', *, *, #2887, .F. ) ;
#2706 = DIRECTION ( 'NONE',  ( -0.000000000000000000, 1.000000000000000000, -0.000000000000000000 ) ) ;
#2707 = CARTESIAN_POINT ( 'NONE',  ( -13.57481594606304576, 36.23749999999999005, 0.000000000000000000 ) ) ;
#2708 = CARTESIAN_POINT ( 'NONE',  ( 143.1451861577818079, 37.92421875108392726, 5.444914386472293977 ) ) ;
#2709 = ORIENTED_EDGE ( 'NONE', *, *, #23068, .F. ) ;
#2710 = CARTESIAN_POINT ( 'NONE',  ( 94.33688103937537051, 114.1144967660473242, -50.20000000000000995 ) ) ;
#2711 = CARTESIAN_POINT ( 'NONE',  ( 100.4037632238151048, 123.0000000000000426, 2.336451931449787356 ) ) ;
#2712 = CARTESIAN_POINT ( 'NONE',  ( 103.5355339059327093, 82.75000000273119838, -3.535533905932755072 ) ) ;
#2713 = CARTESIAN_POINT ( 'NONE',  ( 96.46446609406726225, 92.37500000000000000, -3.535533905932738197 ) ) ;
#2714 = VECTOR ( 'NONE', #22615, 1000.000000000000000 ) ;
#2715 = CARTESIAN_POINT ( 'NONE',  ( 60.54052658636183537, 35.99999999999998579, -12.68347323196786292 ) ) ;
#2716 = EDGE_CURVE ( 'NONE', #17777, #16548, #13009, .T. ) ;
#2717 = CARTESIAN_POINT ( 'NONE',  ( 107.0000000000000000, 107.7255621263696668, -50.10000000000001563 ) ) ;
#2718 = CARTESIAN_POINT ( 'NONE',  ( 51.85481384221819923, 32.76484375108393010, -5.444914386472297529 ) ) ;
#2719 = VERTEX_POINT ( 'NONE', #7023 ) ;
#2720 = CARTESIAN_POINT ( 'NONE',  ( 95.00000000000000000, 95.31249999726880162, -2.071067811865479058 ) ) ;
#2721 = CARTESIAN_POINT ( 'NONE',  ( 94.99999999999995737, 2.071067811865491048, 13.93749999999999822 ) ) ;
#2722 = ORIENTED_EDGE ( 'NONE', *, *, #23773, .F. ) ;
#2723 = CARTESIAN_POINT ( 'NONE',  ( -9.295050272127044266, 36.88242187608393152, 9.295050272127047819 ) ) ;
#2724 = CARTESIAN_POINT ( 'NONE',  ( 181.4251840539369596, 33.16171875216787868, 0.000000000000000000 ) ) ;
#2725 = CARTESIAN_POINT ( 'NONE',  ( 13.14518615778179544, 34.60039062608392868, -1.609821015232357215E-15 ) ) ;
#2726 = ADVANCED_FACE ( 'NONE', ( #2770 ), #22578, .T. ) ;
#2727 = CARTESIAN_POINT ( 'NONE',  ( 204.5988444088204403, 40.00781250216787299, -9.598844408820458085 ) ) ;
#2728 = CARTESIAN_POINT ( 'NONE',  ( 9.295050272127047819, 34.69960937608393436, 9.295050272127046043 ) ) ;
#2729 = CARTESIAN_POINT ( 'NONE',  ( 143.1451861577818079, 32.96328125108393436, 5.444914386472293977 ) ) ;
#2730 = CARTESIAN_POINT ( 'NONE',  ( 74.59884440882045453, 34.94765624999999432, 9.598844408820456309 ) ) ;
#2731 = DIRECTION ( 'NONE',  ( -0.000000000000000000, 1.000000000000000000, -0.000000000000000000 ) ) ;
#2732 = CARTESIAN_POINT ( 'NONE',  ( 96.84719886470459471, 3.152801135295383084, 11.56250000136559208 ) ) ;
#2733 = DIRECTION ( 'NONE',  ( -0.000000000000000000, -0.000000000000000000, -1.000000000000000000 ) ) ;
#2734 = CARTESIAN_POINT ( 'NONE',  ( 98.15313185440925281, -4.458734124999987891, 0.6250000013655921949 ) ) ;
#2735 = CARTESIAN_POINT ( 'NONE',  ( 97.83688103937538472, 116.6573956140660897, -52.90000000546237402 ) ) ;
#2736 = DIRECTION ( 'NONE',  ( 0.000000000000000000, 0.000000000000000000, 1.000000000000000000 ) ) ;
#2737 = CYLINDRICAL_SURFACE ( 'NONE', #5278, 5.000000000000004441 ) ;
#2738 = CARTESIAN_POINT ( 'NONE',  ( 97.50236033167490746, 102.3130555110000159, -47.22499999726881725 ) ) ;
#2739 = CARTESIAN_POINT ( 'NONE',  ( -8.049105076161786076E-16, 36.58476562608393579, -13.14518615778179544 ) ) ;
#2740 = EDGE_CURVE ( 'NONE', #21141, #21949, #922, .T. ) ;
#2741 = CIRCLE ( 'NONE', #3651, 9.000000000000007105 ) ;
#2742 = ORIENTED_EDGE ( 'NONE', *, *, #930, .F. ) ;
#2743 = SURFACE_STYLE_FILL_AREA ( #7568 ) ;
#2744 =( BOUNDED_CURVE ( )  B_SPLINE_CURVE ( 2, ( #4644, #19740, #13302 ),
 .UNSPECIFIED., .F., .F. ) 
 B_SPLINE_CURVE_WITH_KNOTS ( ( 3, 3 ),
 ( 0.5208333333333332593, 0.5249747582430959181 ),
 .UNSPECIFIED. ) 
 CURVE ( )  GEOMETRIC_REPRESENTATION_ITEM ( )  RATIONAL_B_SPLINE_CURVE ( ( 1.000000000000000888, 0.9697362687807495885, 0.9635368518655813563 ) ) 
 REPRESENTATION_ITEM ( '' )  );
#2745 = CARTESIAN_POINT ( 'NONE',  ( 94.99999999999995737, 1.387778780781445676E-14, 4.125000002731185056 ) ) ;
#2746 = CARTESIAN_POINT ( 'NONE',  ( 99.99999999999995737, -4.999999999999990230, 1.249999999999999334 ) ) ;
#2747 = CARTESIAN_POINT ( 'NONE',  ( 208.1451861577817795, 34.55078125108393294, 5.444914386472293977 ) ) ;
#2748 = ORIENTED_EDGE ( 'NONE', *, *, #26047, .F. ) ;
#2749 = CARTESIAN_POINT ( 'NONE',  ( 191.9606029491974084, 53.88964894337311762, -15.00000000000000000 ) ) ;
#2750 = CARTESIAN_POINT ( 'NONE',  ( 96.84719886470459471, -3.152801135295355994, 11.81250000136559208 ) ) ;
#2751 = AXIS2_PLACEMENT_3D ( 'NONE', #27587, #14727, #10734 ) ;
#2752 = EDGE_LOOP ( 'NONE', ( #12074, #21349, #19696, #18924 ) ) ;
#2753 = CARTESIAN_POINT ( 'NONE',  ( 108.0825317500000153, 110.0000000000000000, -54.37500000273119838 ) ) ;
#2754 = CARTESIAN_POINT ( 'NONE',  ( 13.14518615778179900, 37.72578125108393721, 5.444914386472293977 ) ) ;
#2755 = CARTESIAN_POINT ( 'NONE',  ( 102.4999999999999716, 123.8500000000000085, -1.035533905932742638 ) ) ;
#2756 = CARTESIAN_POINT ( 'NONE',  ( 120.4011555911795455, 31.67343750216787512, 9.598844408820459861 ) ) ;
#2757 = CARTESIAN_POINT ( 'NONE',  ( 107.0000000000000142, 110.0000000000000000, -43.50000000546237544 ) ) ;
#2758 = CARTESIAN_POINT ( 'NONE',  ( -13.14518615778179189, 35.04687500108393294, 5.444914386472304635 ) ) ;
#2759 = CIRCLE ( 'NONE', #9135, 11.57481594606304398 ) ;
#2760 = CARTESIAN_POINT ( 'NONE',  ( 99.99999999999998579, 93.62499999726881583, 4.999999999999984013 ) ) ;
#2761 = CARTESIAN_POINT ( 'NONE',  ( 59.55508561352770158, 38.51953125108393294, 13.14518615778179722 ) ) ;
#2762 = CARTESIAN_POINT ( 'NONE',  ( 58.58713332374817639, 50.00000000108478559, -11.99502265407751267 ) ) ;
#2763 = CARTESIAN_POINT ( 'NONE',  ( 108.0825317500000011, 112.6261737610028320, -54.27500000273118985 ) ) ;
#2764 = CARTESIAN_POINT ( 'NONE',  ( 185.7049497278729575, 32.11992187608393579, 9.295050272127047819 ) ) ;
#2765 = CARTESIAN_POINT ( 'NONE',  ( 72.75412397599441761, 36.00000000000002842, 10.77549638133779553 ) ) ;
#2766 = CARTESIAN_POINT ( 'NONE',  ( -9.295050272127046043, 35.89023437608393152, -9.295050272127046043 ) ) ;
#2767 = CARTESIAN_POINT ( 'NONE',  ( 103.1528011352953342, -3.152801135295355106, 7.062500001365592972 ) ) ;
#2768 = CARTESIAN_POINT ( 'NONE',  ( 65.00000000000000000, 36.38632812608393152, -13.14518615778179544 ) ) ;
#2769 = FACE_OUTER_BOUND ( 'NONE', #17556, .T. ) ;
#2770 = FACE_OUTER_BOUND ( 'NONE', #10578, .T. ) ;
#2771 = ORIENTED_EDGE ( 'NONE', *, *, #3331, .T. ) ;
#2772 = CARTESIAN_POINT ( 'NONE',  ( -5.444914386472299306, 38.51953125108393294, 13.14518615778179722 ) ) ;
#2773 = CARTESIAN_POINT ( 'NONE',  ( -8.312177448680279460E-16, 36.03906250000000000, -13.57481594606304576 ) ) ;
#2774 = CARTESIAN_POINT ( 'NONE',  ( 208.1451861577818079, 37.92421875108393436, 5.444914386472293977 ) ) ;
#2775 = CARTESIAN_POINT ( 'NONE',  ( 99.99999999999997158, 118.4984768113314004, -50.37499999726881583 ) ) ;
#2776 = ORIENTED_EDGE ( 'NONE', *, *, #18913, .T. ) ;
#2777 = CARTESIAN_POINT ( 'NONE',  ( -9.598844408820458085, 32.16953124999999147, -9.598844408820458085 ) ) ;
#2778 = CARTESIAN_POINT ( 'NONE',  ( -9.295050272127046043, 34.89804687608393152, -9.295050272127046043 ) ) ;
#2779 = ORIENTED_EDGE ( 'NONE', *, *, #19455, .T. ) ;
#2780 = CARTESIAN_POINT ( 'NONE',  ( 143.1451861577818079, 34.74921875108395142, 5.444914386472293977 ) ) ;
#2781 = CARTESIAN_POINT ( 'NONE',  ( 51.85481384221820633, 40.75195312608393294, 0.000000000000000000 ) ) ;
#2782 = CARTESIAN_POINT ( 'NONE',  ( 200.4449143864723055, 35.44375000108393436, 13.14518615778179189 ) ) ;
#2783 =( BOUNDED_CURVE ( )  B_SPLINE_CURVE ( 2, ( #14333, #8593, #5668, #19428, #23848, #1396, #12048, #18634, #1670 ),
 .UNSPECIFIED., .F., .F. ) 
 B_SPLINE_CURVE_WITH_KNOTS ( ( 3, 2, 2, 2, 3 ),
 ( 0.7291666666666668517, 0.7395833333333334814, 0.7500000000000001110, 0.7604166666666667407, 0.7708333333333333703 ),
 .UNSPECIFIED. ) 
 CURVE ( )  GEOMETRIC_REPRESENTATION_ITEM ( )  RATIONAL_B_SPLINE_CURVE ( ( 0.9999999999999983347, 0.9238795325112884038, 1.000000000000000000, 0.9238795325112867385, 1.000000000000000000, 0.9238795325112867385, 1.000000000000000000, 0.9238795325112867385, 1.000000000000000000 ) ) 
 REPRESENTATION_ITEM ( '' )  );
#2784 = ORIENTED_EDGE ( 'NONE', *, *, #12107, .T. ) ;
#2785 = CARTESIAN_POINT ( 'NONE',  ( 97.93301270000000613, 123.7500000010924879, -9.540979117872439019E-15 ) ) ;
#2786 = CARTESIAN_POINT ( 'NONE',  ( 104.9999999999999858, -2.071067811865442643, 1.562500002731185722 ) ) ;
#2787 = AXIS2_PLACEMENT_3D ( 'NONE', #5811, #14482, #23199 ) ;
#2788 = CARTESIAN_POINT ( 'NONE',  ( 91.91746824999998466, 107.3738262389971680, -49.02500000273119696 ) ) ;
#2789 = CARTESIAN_POINT ( 'NONE',  ( 99.99999999999998579, 128.0000000000000000, -5.204170427930421283E-15 ) ) ;
#2790 = CARTESIAN_POINT ( 'NONE',  ( 2.493653234604083739E-15, 36.43593749999999432, 13.57481594606304576 ) ) ;
#2791 = CARTESIAN_POINT ( 'NONE',  ( 68.04460945692940754, 53.89089363584395898, 14.99999999999997868 ) ) ;
#2792 = CARTESIAN_POINT ( 'NONE',  ( 96.84719886470459471, 3.152801135295383084, 6.312500001365592084 ) ) ;
#2793 = VERTEX_POINT ( 'NONE', #18442 ) ;
#2794 = CARTESIAN_POINT ( 'NONE',  ( 101.4615807364564546, 122.6500000010924794, -1.461580736456474794 ) ) ;
#2795 = CARTESIAN_POINT ( 'NONE',  ( 95.54126587499995082, 1.846868145590750077, 8.375000001365592084 ) ) ;
#2796 = CYLINDRICAL_SURFACE ( 'NONE', #14411, 25.00000000000001066 ) ;
#2797 = CARTESIAN_POINT ( 'NONE',  ( 5.444914386472302859, 34.45156250108393436, 13.14518615778179189 ) ) ;
#2798 = CARTESIAN_POINT ( 'NONE',  ( 103.5355338419364699, 95.00000000000001421, -3.535533969929001596 ) ) ;
#2799 = CARTESIAN_POINT ( 'NONE',  ( 65.00000000000000000, 37.32890625216786873, 13.57481594606304576 ) ) ;
#2800 = CARTESIAN_POINT ( 'NONE',  ( 101.8468681455907330, 94.12499999863439371, 4.458734124999979898 ) ) ;
#2801 = CARTESIAN_POINT ( 'NONE',  ( 181.4251840539369596, 37.87460937499999147, 5.622872871577880183 ) ) ;
#2802 = CARTESIAN_POINT ( 'NONE',  ( -5.444914386472297529, 37.22968750108394431, -13.14518615778179722 ) ) ;
#2803 = LINE ( 'NONE', #528, #6630 ) ;
#2804 = DIRECTION ( 'NONE',  ( -0.8490667072653959035, 1.618318251311064231E-06, -0.5282856486891157610 ) ) ;
#2805 = DIRECTION ( 'NONE',  ( 0.000000000000000000, 0.000000000000000000, 1.000000000000000000 ) ) ;
#2806 = CARTESIAN_POINT ( 'NONE',  ( 120.4011555911795455, 36.13828124999999147, -9.598844408820458085 ) ) ;
#2807 = ORIENTED_EDGE ( 'NONE', *, *, #10525, .T. ) ;
#2808 = CARTESIAN_POINT ( 'NONE',  ( 5.622872871577924592, 33.31054687499999289, 13.57481594606299957 ) ) ;
#2809 = CARTESIAN_POINT ( 'NONE',  ( -5.444914386472299306, 32.16953125108393152, 13.14518615778179722 ) ) ;
#2810 = CARTESIAN_POINT ( 'NONE',  ( 9.598844408820456309, 35.24531250216787726, -9.598844408820458085 ) ) ;
#2811 = CARTESIAN_POINT ( 'NONE',  ( 104.9999999999999716, 1.449011120738813565E-14, 10.62500000273118594 ) ) ;
#2812 = CARTESIAN_POINT ( 'NONE',  ( 143.1451861577818079, 33.06250000108393294, -5.444914386472297529 ) ) ;
#2813 = CARTESIAN_POINT ( 'NONE',  ( 55.70494972787295751, 39.85898437608393152, 9.295050272127047819 ) ) ;
#2814 = EDGE_CURVE ( 'NONE', #3701, #16509, #21793, .T. ) ;
#2815 = CARTESIAN_POINT ( 'NONE',  ( 104.9999999999999716, 80.43750000000002842, 2.071067811865462627 ) ) ;
#2816 = CARTESIAN_POINT ( 'NONE',  ( -8.312177448680279460E-16, 32.96328125216787441, -13.57481594606304576 ) ) ;
#2817 = CARTESIAN_POINT ( 'NONE',  ( 94.99999999999995737, -2.071067811865466624, 2.062499999999998668 ) ) ;
#2818 = DIRECTION ( 'NONE',  ( 0.000000000000000000, 0.000000000000000000, 1.000000000000000000 ) ) ;
#2819 = CARTESIAN_POINT ( 'NONE',  ( -8.312177448680279460E-16, 38.51953125216787299, -13.57481594606304576 ) ) ;
#2820 = CARTESIAN_POINT ( 'NONE',  ( 195.0000000000000000, 34.79882812608393294, -13.14518615778179544 ) ) ;
#2821 = CARTESIAN_POINT ( 'NONE',  ( 0.000000000000000000, 40.99999999999999289, 0.000000000000000000 ) ) ;
#2822 = CARTESIAN_POINT ( 'NONE',  ( 107.0000000000000000, 110.0000000000000000, -52.00000000000001421 ) ) ;
#2823 =( NAMED_UNIT ( * ) SI_UNIT ( $, .STERADIAN. ) SOLID_ANGLE_UNIT ( ) );
#2825 = ORIENTED_EDGE ( 'NONE', *, *, #3764, .F. ) ;
#2824 = CARTESIAN_POINT ( 'NONE',  ( 204.5988444088204403, 39.11484374999999858, -9.598844408820458085 ) ) ;
#2826 = CARTESIAN_POINT ( 'NONE',  ( -5.622872871577782483, 35.29492187499999289, -13.57481594606313990 ) ) ;
#2827 = CARTESIAN_POINT ( 'NONE',  ( 99.99999999999995737, 85.00000000000000000, 2.999999999999990674 ) ) ;
#2828 = CARTESIAN_POINT ( 'NONE',  ( -13.57481594606304576, 34.69960937499999432, 5.622872871577880183 ) ) ;
#2829 = DIRECTION ( 'NONE',  ( -1.040834085586084848E-15, 1.000000000000000000, 0.000000000000000000 ) ) ;
#2830 = CARTESIAN_POINT ( 'NONE',  ( 13.14518615778179900, 34.05468750108394005, -5.444914386472297529 ) ) ;
#2831 = CARTESIAN_POINT ( 'NONE',  ( 9.295050272127046043, 34.69960937608393436, -9.295050272127046043 ) ) ;
#2832 = CARTESIAN_POINT ( 'NONE',  ( 185.4011555911795597, 32.36796874999999574, 9.598844408820459861 ) ) ;
#2833 = CARTESIAN_POINT ( 'NONE',  ( -13.57481594606304753, 35.49335937716787015, -5.622872871577873077 ) ) ;
#2834 = CARTESIAN_POINT ( 'NONE',  ( -5.622872871577839327, 38.07304687716787583, 13.57481594606308128 ) ) ;
#2835 = CARTESIAN_POINT ( 'NONE',  ( 98.15313185440925281, 84.25000000136559208, -4.458734125000016313 ) ) ;
#2836 = CARTESIAN_POINT ( 'NONE',  ( 51.85481384221820633, 35.04687500108393294, 5.444914386472304635 ) ) ;
#2837 = FACE_BOUND ( 'NONE', #27498, .T. ) ;
#2838 = CARTESIAN_POINT ( 'NONE',  ( 102.3057342235964882, 122.9999999999999858, -0.9766400096817489107 ) ) ;
#2839 = CARTESIAN_POINT ( 'NONE',  ( 101.4615807364564546, 124.2500000010924879, -1.461580736456474794 ) ) ;
#2840 = CARTESIAN_POINT ( 'NONE',  ( 13.57481594606304931, 33.40976562499999858, 5.622872871577869525 ) ) ;
#2841 = CARTESIAN_POINT ( 'NONE',  ( 130.0000000000000000, 38.56914062608393579, 13.14518615778179544 ) ) ;
#2842 = VERTEX_POINT ( 'NONE', #26571 ) ;
#2843 = CARTESIAN_POINT ( 'NONE',  ( 94.99999999999995737, 82.00000000000000000, -1.387778780781445676E-14 ) ) ;
#2844 = CARTESIAN_POINT ( 'NONE',  ( 78.57481594606305464, 38.32109375216786873, -1.662435489736055892E-15 ) ) ;
#2845 = CARTESIAN_POINT ( 'NONE',  ( 97.92893218813451028, 79.93750000273119838, -5.000000000000018652 ) ) ;
#2846 = CARTESIAN_POINT ( 'NONE',  ( 103.5355339059327235, 91.12500000000000000, -3.535533905932738197 ) ) ;
#2847 = CARTESIAN_POINT ( 'NONE',  ( 9.598844408820459861, 34.15390624999999858, 9.598844408820456309 ) ) ;
#2848 = CARTESIAN_POINT ( 'NONE',  ( 99.99999999999997158, 102.6397644303321215, -54.50000000000000711 ) ) ;
#2849 = CARTESIAN_POINT ( 'NONE',  ( 51.42518405393695957, 40.25585937499999289, 5.622872871577880183 ) ) ;
#2850 = EDGE_LOOP ( 'NONE', ( #21299, #23566, #9122, #16662 ) ) ;
#2851 = CARTESIAN_POINT ( 'NONE',  ( 9.598844408820456309, 32.86406250216787583, -9.598844408820458085 ) ) ;
#2852 = AXIS2_PLACEMENT_3D ( 'NONE', #23754, #6637, #24035 ) ;
#2853 = CARTESIAN_POINT ( 'NONE',  ( 94.99999999999995737, 2.071067811865491048, 14.93750000000000000 ) ) ;
#2854 = EDGE_CURVE ( 'NONE', #19811, #10089, #8507, .T. ) ;
#2855 = ORIENTED_EDGE ( 'NONE', *, *, #27287, .F. ) ;
#2856 = CARTESIAN_POINT ( 'NONE',  ( 13.14518615778179900, 37.22968750108393721, -5.444914386472297529 ) ) ;
#2857 = CARTESIAN_POINT ( 'NONE',  ( 200.6228728715778686, 34.50117187716788436, -13.57481594606304753 ) ) ;
#2858 = CARTESIAN_POINT ( 'NONE',  ( -5.444914386472299306, 33.55859375108393294, 13.14518615778179722 ) ) ;
#2859 = CARTESIAN_POINT ( 'NONE',  ( -8.312177448680279460E-16, 32.07031249999999289, -13.57481594606304576 ) ) ;
#2860 = CARTESIAN_POINT ( 'NONE',  ( 107.5412658750000077, 110.0000000000000000, -43.81250000409678336 ) ) ;
#2861 = CARTESIAN_POINT ( 'NONE',  ( -13.14518615778179900, 35.14609375108393152, -5.444914386472297529 ) ) ;
#2862 = CARTESIAN_POINT ( 'NONE',  ( 124.5550856135277087, 32.46718750108393436, -13.14518615778179900 ) ) ;
#2863 = CARTESIAN_POINT ( 'NONE',  ( 96.84719886470463734, 90.93749999863440792, 3.152801135295351997 ) ) ;
#2864 = DIRECTION ( 'NONE',  ( -0.000000000000000000, 1.000000000000000000, -0.000000000000000000 ) ) ;
#2865 = CARTESIAN_POINT ( 'NONE',  ( 104.4587341249999639, 1.442382525525748735E-14, 8.187500001365592084 ) ) ;
#2866 = CARTESIAN_POINT ( 'NONE',  ( 208.2454503467689904, 36.00000000000000711, 2.307131236160025800 ) ) ;
#2867 = CARTESIAN_POINT ( 'NONE',  ( 103.1528011352953342, -3.152801135295355106, 9.812500001365593860 ) ) ;
#2868 = CARTESIAN_POINT ( 'NONE',  ( 107.0000000000000142, 112.2744378736303332, -53.40000000546237402 ) ) ;
#2869 = CYLINDRICAL_SURFACE ( 'NONE', #20474, 13.57481594606304398 ) ;
#2870 = CARTESIAN_POINT ( 'NONE',  ( 99.99999999999995737, 78.00000000000000000, -1.387778780781445676E-14 ) ) ;
#2871 = CARTESIAN_POINT ( 'NONE',  ( 107.0000000000000142, 110.0000000000000000, -49.50000000546238255 ) ) ;
#2872 = CARTESIAN_POINT ( 'NONE',  ( -13.14518615778179189, 33.65781250108393152, 5.444914386472304635 ) ) ;
#2873 = COLOUR_RGB ( '', 0.09019608, 0.27058824, 0.51372549) ;
#2874 = ORIENTED_EDGE ( 'NONE', *, *, #16651, .F. ) ;
#2875 = CARTESIAN_POINT ( 'NONE',  ( 99.99999999999998579, 95.12499999726881583, -4.999999999999997335 ) ) ;
#2876 = CARTESIAN_POINT ( 'NONE',  ( 195.0000000000000000, 52.00000000000000711, -11.57481594606306707 ) ) ;
#2877 = DIRECTION ( 'NONE',  ( -0.000000000000000000, -1.000000000000000000, -0.000000000000000000 ) ) ;
#2878 = CARTESIAN_POINT ( 'NONE',  ( 185.7049497278729575, 34.89804687608393152, -9.295050272127046043 ) ) ;
#2879 = VERTEX_POINT ( 'NONE', #4910 ) ;
#2880 = EDGE_CURVE ( 'NONE', #5815, #6644, #16145, .T. ) ;
#2881 = CARTESIAN_POINT ( 'NONE',  ( -8.312177448680279460E-16, 40.10703125216787157, -13.57481594606304576 ) ) ;
#2882 = CARTESIAN_POINT ( 'NONE',  ( 101.8468681455906903, -4.458734124999987891, 11.00000000136559208 ) ) ;
#2883 = ORIENTED_EDGE ( 'NONE', *, *, #3607, .T. ) ;
#2884 = CARTESIAN_POINT ( 'NONE',  ( 108.0825317500000011, 112.6261737610028320, -52.27500000273118985 ) ) ;
#2885 = CARTESIAN_POINT ( 'NONE',  ( 9.295050272127047819, 36.88242187608393152, 9.295050272127046043 ) ) ;
#2886 = CARTESIAN_POINT ( 'NONE',  ( 99.99999999999998579, 124.7999999999999972, -2.499999999999997780 ) ) ;
#2887 = EDGE_CURVE ( 'NONE', #2527, #9281, #14118, .T. ) ;
#2888 = B_SPLINE_CURVE_WITH_KNOTS ( 'NONE', 3,
 ( #12183, #9645, #11770, #22776, #11911, #1117, #978, #25178, #12045, #5666, #23050, #3524, #25877, #19319, #2226, #3940, #17314, #8624, #19178, #6214, #14607, #23741, #25592, #10325, #8342 ),
 .UNSPECIFIED., .F., .F.,
 ( 4, 2, 2, 2, 2, 2, 2, 1, 2, 2, 2, 2, 4 ),
 ( 0.000000000000000000, 0.001301161269048876174, 0.002602322538097752349, 0.005204645076195502963, 0.007806967614293254878, 0.01040929015239100593, 0.01171045142143988319, 0.01301161269048875871, 0.01431277395953763597, 0.01561393522858651149, 0.01821625776668426427, 0.01951741903573314327, 0.02081858030478202226 ),
 .UNSPECIFIED. ) ;
#2889 = CARTESIAN_POINT ( 'NONE',  ( 116.8548138422182063, 37.42812500108393436, 5.444914386472304635 ) ) ;
#2890 = CARTESIAN_POINT ( 'NONE',  ( 5.444914386472297529, 36.53515625108394715, -13.14518615778179722 ) ) ;
#2891 = CARTESIAN_POINT ( 'NONE',  ( 13.14518615778179900, 34.55078125108393294, 5.444914386472293977 ) ) ;
#2892 = ADVANCED_BREP_SHAPE_REPRESENTATION ( '', ( #7448, #26844 ), #12238 ) ;
#2893 = CARTESIAN_POINT ( 'NONE',  ( 104.4587341249999923, 93.49999999863442213, 1.846868145590726318 ) ) ;
#2894 = CARTESIAN_POINT ( 'NONE',  ( 69.57159163252556766, 51.44262710532576932, -14.99999999999933742 ) ) ;
#2895 = CARTESIAN_POINT ( 'NONE',  ( 97.50236033167492167, 117.6869444889999841, -53.77500000273119696 ) ) ;
#2896 = CARTESIAN_POINT ( 'NONE',  ( 181.4251840539369596, 40.15664062500000142, -5.622872871577873077 ) ) ;
#2897 = EDGE_CURVE ( 'NONE', #2435, #24292, #1999, .T. ) ;
#2898 = CARTESIAN_POINT ( 'NONE',  ( 0.000000000000000000, 1.000000000000000000, 23.26794919243112858 ) ) ;
#2899 = CARTESIAN_POINT ( 'NONE',  ( -13.14518615778179900, 36.73359375108393010, -5.444914386472297529 ) ) ;
#2900 = CARTESIAN_POINT ( 'NONE',  ( 103.1528011352953342, -3.152801135295355106, 9.062500001365592084 ) ) ;
#2901 =( BOUNDED_CURVE ( )  B_SPLINE_CURVE ( 2, ( #8242, #12224, #14780, #6114, #18535, #27239, #5573 ),
 .UNSPECIFIED., .F., .F. ) 
 B_SPLINE_CURVE_WITH_KNOTS ( ( 3, 2, 2, 3 ),
 ( 0.4520580917964582834, 0.4583333333333333148, 0.4687500000000000555, 0.4791666666666667962 ),
 .UNSPECIFIED. ) 
 CURVE ( )  GEOMETRIC_REPRESENTATION_ITEM ( )  RATIONAL_B_SPLINE_CURVE ( ( 0.9635368512068458458, 0.9541432653384140927, 1.000000000000000000, 0.9238795325112867385, 1.000000000000000000, 0.9238795325112859613, 1.000000000000000888 ) ) 
 REPRESENTATION_ITEM ( '' )  );
#2902 = CARTESIAN_POINT ( 'NONE',  ( 55.70494972787295751, 37.27929687608393294, -9.295050272127046043 ) ) ;
#2903 = DIRECTION ( 'NONE',  ( -5.782411586589357392E-17, -1.156482317317871478E-16, -1.000000000000000000 ) ) ;
#2904 = CARTESIAN_POINT ( 'NONE',  ( 96.46446609406721961, -3.535533905932727539, 14.12499999999999822 ) ) ;
#2905 = CARTESIAN_POINT ( 'NONE',  ( 5.444914386472302859, 35.44375000108393436, 13.14518615778179189 ) ) ;
#2906 = CARTESIAN_POINT ( 'NONE',  ( 99.14382582708707048, 123.6000000010924680, -2.066987299999999195 ) ) ;
#2907 = CARTESIAN_POINT ( 'NONE',  ( 101.8468681455907330, 91.37499999863442213, 4.458734124999980786 ) ) ;
#2908 = CARTESIAN_POINT ( 'NONE',  ( 195.0000000000000000, 37.77539062608393294, 13.14518615778179544 ) ) ;
#2909 = CARTESIAN_POINT ( 'NONE',  ( 108.0825317499999869, 107.3738262389971538, -50.97499999726881015 ) ) ;
#2910 = VERTEX_POINT ( 'NONE', #3855 ) ;
#2911 = CARTESIAN_POINT ( 'NONE',  ( -5.622872871577873077, 34.79882812499998579, 13.57481594606304753 ) ) ;
#2912 = CARTESIAN_POINT ( 'NONE',  ( -13.14518615778179544, 34.20351562608393436, 0.000000000000000000 ) ) ;
#2913 = ORIENTED_EDGE ( 'NONE', *, *, #11909, .T. ) ;
#2914 = CARTESIAN_POINT ( 'NONE',  ( 116.8548138422182063, 32.76484375108393010, -5.444914386472297529 ) ) ;
#2915 = CARTESIAN_POINT ( 'NONE',  ( 7.171390501253594785, 31.30502191632583830, -11.52591802191987114 ) ) ;
#2916 = CARTESIAN_POINT ( 'NONE',  ( 204.2950502721270425, 33.90585937608393863, 9.295050272127046043 ) ) ;
#2917 = EDGE_LOOP ( 'NONE', ( #4462, #19296, #4936, #14694 ) ) ;
#2918 = CARTESIAN_POINT ( 'NONE',  ( 103.5355339059327093, 3.535533905932755072, 10.75000000273118594 ) ) ;
#2919 = CARTESIAN_POINT ( 'NONE',  ( 7.636241067997081799, 54.91786508990981019, -14.99999999999999822 ) ) ;
#2920 = CARTESIAN_POINT ( 'NONE',  ( 101.0355339059327093, 124.0500000021849445, -2.500000000000002665 ) ) ;
#2921 = EDGE_CURVE ( 'NONE', #20854, #7547, #13184, .T. ) ;
#2922 = CARTESIAN_POINT ( 'NONE',  ( 130.0000000000000000, 36.93203125216787441, -13.57481594606304576 ) ) ;
#2923 = CARTESIAN_POINT ( 'NONE',  ( 108.0825317500000153, 110.0000000000000000, -46.12500000273119838 ) ) ;
#2924 = CARTESIAN_POINT ( 'NONE',  ( -13.57481594606304753, 34.69960937716787441, -5.622872871577872189 ) ) ;
#2925 = CARTESIAN_POINT ( 'NONE',  ( 65.98306518510102592, 49.99999999949029217, 13.54930971656748717 ) ) ;
#2926 = VERTEX_POINT ( 'NONE', #12931 ) ;
#2927 = CARTESIAN_POINT ( 'NONE',  ( 96.84719886470459471, -3.152801135295355994, 6.562500001365592084 ) ) ;
#2928 = VERTEX_POINT ( 'NONE', #28203 ) ;
#2929 = CARTESIAN_POINT ( 'NONE',  ( 99.99999999999995737, 5.000000000000018652, 12.87500000273118594 ) ) ;
#2930 = CARTESIAN_POINT ( 'NONE',  ( 96.84719886470459471, 3.152801135295383084, 7.312500001365592084 ) ) ;
#2931 = CARTESIAN_POINT ( 'NONE',  ( 135.3237909639547070, 54.47170356488064868, 14.99999999999996447 ) ) ;
#2932 = CARTESIAN_POINT ( 'NONE',  ( -8.049105076161786076E-16, 37.18007812608393436, -13.14518615778179544 ) ) ;
#2933 = CARTESIAN_POINT ( 'NONE',  ( -12.83975123685818964, 35.99999999999999289, 2.850296047819762535 ) ) ;
#2934 = CARTESIAN_POINT ( 'NONE',  ( 51.85481384221820633, 32.81445312608393294, 0.000000000000000000 ) ) ;
#2935 = CARTESIAN_POINT ( 'NONE',  ( 102.4976396683250925, 102.3130555110000159, -44.52500000273119696 ) ) ;
#2936 = CARTESIAN_POINT ( 'NONE',  ( 5.444914386472297529, 37.13046875108393152, -13.14518615778179722 ) ) ;
#2937 = VECTOR ( 'NONE', #3164, 1000.000000000000000 ) ;
#2938 = DIRECTION ( 'NONE',  ( 0.000000000000000000, -1.000000000000000000, 0.000000000000000000 ) ) ;
#2939 = CARTESIAN_POINT ( 'NONE',  ( 0.4460412567804681316, 49.99999999978076204, 13.57776691409236314 ) ) ;
#2940 = CARTESIAN_POINT ( 'NONE',  ( 97.92893218813452449, 91.18749999726880162, -4.999999999999997335 ) ) ;
#2941 = CARTESIAN_POINT ( 'NONE',  ( 130.0000000000000000, 33.65781249999999147, -13.57481594606304576 ) ) ;
#2942 = EDGE_LOOP ( 'NONE', ( #20773, #11386, #17741, #16971 ) ) ;
#2943 = CARTESIAN_POINT ( 'NONE',  ( 5.622872871577870413, 33.60820312499999574, -13.57481594606304753 ) ) ;
#2944 =( BOUNDED_CURVE ( )  B_SPLINE_CURVE ( 2, ( #19603, #28164, #8631, #26018, #26158, #23883, #15311, #24026, #21900 ),
 .UNSPECIFIED., .F., .F. ) 
 B_SPLINE_CURVE_WITH_KNOTS ( ( 3, 2, 2, 2, 3 ),
 ( 0.8500000000000007550, 0.8750000000000008882, 0.9000000000000009104, 0.9250000000000009326, 0.9500000000000009548 ),
 .UNSPECIFIED. ) 
 CURVE ( )  GEOMETRIC_REPRESENTATION_ITEM ( )  RATIONAL_B_SPLINE_CURVE ( ( 0.9999999999999976685, 0.9238795325112890700, 1.000000000000000000, 0.9238795325112867385, 1.000000000000000000, 0.9238795325112867385, 1.000000000000000000, 0.9238795325112837409, 1.000000000000003109 ) ) 
 REPRESENTATION_ITEM ( '' )  );
#2945 = CARTESIAN_POINT ( 'NONE',  ( -5.444914386472299306, 34.55078125108393294, 13.14518615778179722 ) ) ;
#2946 = CARTESIAN_POINT ( 'NONE',  ( -9.598844408820458085, 33.06250000216787299, -9.598844408820458085 ) ) ;
#2947 = CARTESIAN_POINT ( 'NONE',  ( 104.9999999999999574, -2.071067811865462627, 10.56250000273118594 ) ) ;
#2948 = CARTESIAN_POINT ( 'NONE',  ( 130.0000000000000000, 34.79882812608393294, -13.14518615778179544 ) ) ;
#2949 = CARTESIAN_POINT ( 'NONE',  ( 72.17139139501665568, 31.30502190640808990, -11.52591746582321974 ) ) ;
#2950 = CARTESIAN_POINT ( 'NONE',  ( 65.00000000000000000, 36.93203125216787441, -13.57481594606304576 ) ) ;
#2951 = CARTESIAN_POINT ( 'NONE',  ( 9.295050272127047819, 37.67617187608393436, 9.295050272127046043 ) ) ;
#2952 = DIRECTION ( 'NONE',  ( 0.000000000000000000, 0.000000000000000000, 1.000000000000000000 ) ) ;
#2953 = CARTESIAN_POINT ( 'NONE',  ( 102.0710678118654329, 5.000000000000018652, 2.687499999999999112 ) ) ;
#2954 = CARTESIAN_POINT ( 'NONE',  ( 97.50236033167490746, 102.3130555110000159, -53.47499999726882436 ) ) ;
#2955 = CARTESIAN_POINT ( 'NONE',  ( -5.622872871577873077, 40.15664062716787441, -13.57481594606304753 ) ) ;
#2956 = DIRECTION ( 'NONE',  ( 0.000000000000000000, 0.000000000000000000, -1.000000000000000000 ) ) ;
#2957 = CARTESIAN_POINT ( 'NONE',  ( 101.0355339059327378, 124.7569999999781629, -2.499999999999997780 ) ) ;
#2958 = CARTESIAN_POINT ( 'NONE',  ( 100.8561741729129295, 124.0000000010925021, 2.066987299999979211 ) ) ;
#2959 = CARTESIAN_POINT ( 'NONE',  ( 195.0000000000000000, 40.00781250000000000, -13.57481594606304576 ) ) ;
#2960 = CARTESIAN_POINT ( 'NONE',  ( 103.5355339059327093, -3.535533905932726206, 10.50000000273118594 ) ) ;
#2961 = CARTESIAN_POINT ( 'NONE',  ( 97.92893218813451028, 5.000000000000018652, 12.81250000000000000 ) ) ;
#2962 = CARTESIAN_POINT ( 'NONE',  ( 13.57481594606304753, 32.71523437500000142, -5.622872871577873077 ) ) ;
#2963 = CARTESIAN_POINT ( 'NONE',  ( 7.171390501253594785, 31.30502191632583830, -11.52591802191987114 ) ) ;
#2964 = CARTESIAN_POINT ( 'NONE',  ( 9.295050272127046043, 34.89804687608393863, -9.295050272127046043 ) ) ;
#2965 = CARTESIAN_POINT ( 'NONE',  ( -13.14518615778179900, 36.53515625108392584, -5.444914386472297529 ) ) ;
#2966 = CARTESIAN_POINT ( 'NONE',  ( -9.295050272127044266, 34.30273437608393294, 9.295050272127047819 ) ) ;
#2967 = CARTESIAN_POINT ( 'NONE',  ( 9.598844408820459861, 37.42812500216787441, 9.598844408820456309 ) ) ;
#2968 = CARTESIAN_POINT ( 'NONE',  ( 103.5355339059327093, -3.535533905932726206, 4.500000002731185944 ) ) ;
#2969 = CARTESIAN_POINT ( 'NONE',  ( 103.1528011352953342, 82.06250000136559208, -3.152801135295383084 ) ) ;
#2970 = CARTESIAN_POINT ( 'NONE',  ( 74.29505027212704249, 33.70742187608393436, 9.295050272127046043 ) ) ;
#2971 = EDGE_CURVE ( 'NONE', #1428, #24121, #25364, .T. ) ;
#2972 = PLANE ( 'NONE',  #9401 ) ;
#2973 = CARTESIAN_POINT ( 'NONE',  ( -8.312177448680279460E-16, 40.00781250000000000, -13.57481594606304576 ) ) ;
#2974 = ORIENTED_EDGE ( 'NONE', *, *, #1675, .F. ) ;
#2975 = CARTESIAN_POINT ( 'NONE',  ( 5.622872871577946796, 37.27929687499999289, 13.57481594606297115 ) ) ;
#2976 = CARTESIAN_POINT ( 'NONE',  ( -13.57481594606304753, 32.21914062500000142, -5.622872871577873077 ) ) ;
#2977 = CARTESIAN_POINT ( 'NONE',  ( 139.2950502721270425, 33.31054687608394005, -9.295050272127046043 ) ) ;
#2978 = ORIENTED_EDGE ( 'NONE', *, *, #14429, .F. ) ;
#2979 = CARTESIAN_POINT ( 'NONE',  ( 103.5355339059327093, 82.37500000000000000, 3.535533905932726206 ) ) ;
#2980 = AXIS2_PLACEMENT_3D ( 'NONE', #8296, #4034, #16985 ) ;
#2981 = CARTESIAN_POINT ( 'NONE',  ( 96.46446609406726225, 94.62500000000000000, 3.535533905932723986 ) ) ;
#2982 = CARTESIAN_POINT ( 'NONE',  ( 96.46446609406721961, 79.25000000273118417, 3.535533905932727539 ) ) ;
#2983 =( BOUNDED_CURVE ( )  B_SPLINE_CURVE ( 2, ( #3871, #4436, #12949 ),
 .UNSPECIFIED., .F., .F. ) 
 B_SPLINE_CURVE_WITH_KNOTS ( ( 3, 3 ),
 ( 0.9375000000000000000, 0.9448586960708869054 ),
 .UNSPECIFIED. ) 
 CURVE ( )  GEOMETRIC_REPRESENTATION_ITEM ( )  RATIONAL_B_SPLINE_CURVE ( ( 1.000000000000000000, 0.9462258510377660192, 0.9684275648627984623 ) ) 
 REPRESENTATION_ITEM ( '' )  );
#2984 = CARTESIAN_POINT ( 'NONE',  ( 96.46446609406726225, 90.62500000000000000, 3.535533905932723986 ) ) ;
#2985 = DIRECTION ( 'NONE',  ( 0.000000000000000000, 4.625929269271485914E-16, 1.000000000000000000 ) ) ;
#2986 = CARTESIAN_POINT ( 'NONE',  ( 95.00472066334982912, 103.1245878333314323, -49.32499999726881157 ) ) ;
#2987 = CARTESIAN_POINT ( 'NONE',  ( 51.42518405393695957, 40.20624999999999005, 0.000000000000000000 ) ) ;
#2988 = CARTESIAN_POINT ( 'NONE',  ( 13.57481594606304931, 39.85898437716787157, 5.622872871577869525 ) ) ;
#2989 =( GEOMETRIC_REPRESENTATION_CONTEXT ( 3 ) GLOBAL_UNCERTAINTY_ASSIGNED_CONTEXT ( ( #26087 ) ) GLOBAL_UNIT_ASSIGNED_CONTEXT ( ( #4325, #16347, #22916 ) ) REPRESENTATION_CONTEXT ( 'NONE', 'WORKASPACE' ) );
#2990 = CIRCLE ( 'NONE', #6612, 11.57481594606304398 ) ;
#2991 = EDGE_LOOP ( 'NONE', ( #24693, #11613, #10535, #26856, #19842, #22309, #27827, #24422, #25104, #11015 ) ) ;
#2992 = DIRECTION ( 'NONE',  ( 0.000000000000000000, -1.000000000000000000, 0.000000000000000000 ) ) ;
#2993 = CARTESIAN_POINT ( 'NONE',  ( 102.0710678118654329, 5.000000000000018652, 14.68749999999999822 ) ) ;
#2994 = ORIENTED_EDGE ( 'NONE', *, *, #17554, .F. ) ;
#2995 = CARTESIAN_POINT ( 'NONE',  ( 5.444914386472302859, 37.03125000108393294, 13.14518615778179189 ) ) ;
#2996 = CARTESIAN_POINT ( 'NONE',  ( 208.5748159460630120, 35.19570312716788152, -5.622872871577873077 ) ) ;
#2997 = EDGE_LOOP ( 'NONE', ( #217, #7719, #21919, #9314 ) ) ;
#2998 = CARTESIAN_POINT ( 'NONE',  ( -5.444914386472297529, 34.05468750108393294, -13.14518615778179722 ) ) ;
#2999 = CARTESIAN_POINT ( 'NONE',  ( -13.57481594606304576, 32.26874999999999716, 0.000000000000000000 ) ) ;
#3000 = LINE ( 'NONE', #13673, #21644 ) ;
#3001 = CARTESIAN_POINT ( 'NONE',  ( 13.14518615778179900, 36.33671875108394289, 5.444914386472293977 ) ) ;
#3002 = CARTESIAN_POINT ( 'NONE',  ( 139.2950502721270425, 33.11210937608393579, -9.295050272127046043 ) ) ;
#3003 = CARTESIAN_POINT ( 'NONE',  ( 72.17139121699895554, 31.99955315621561525, -11.52591757658528948 ) ) ;
#3004 = CYLINDRICAL_SURFACE ( 'NONE', #25512, 13.57481594606304576 ) ;
#3005 = DIRECTION ( 'NONE',  ( 0.000000000000000000, 0.000000000000000000, 1.000000000000000000 ) ) ;
#3006 = CARTESIAN_POINT ( 'NONE',  ( 117.1602487631418086, 35.99999999999998579, 2.850296047819834033 ) ) ;
#3007 = CARTESIAN_POINT ( 'NONE',  ( 103.1528011352953342, 3.152801135295383084, 5.312500001365592972 ) ) ;
#3008 = CARTESIAN_POINT ( 'NONE',  ( 0.000000000000000000, 30.99999999999999645, 0.000000000000000000 ) ) ;
#3009 = ADVANCED_FACE ( 'NONE', ( #10247 ), #18956, .F. ) ;
#3010 = CARTESIAN_POINT ( 'NONE',  ( 98.15313185440923860, 4.458734125000016313, 8.250000001365592084 ) ) ;
#3011 = CARTESIAN_POINT ( 'NONE',  ( 97.50236033167492167, 102.3130555110000159, -46.72500000273119269 ) ) ;
#3012 = CARTESIAN_POINT ( 'NONE',  ( 100.0000000000000000, 110.0000000000000000, -55.00000000000000711 ) ) ;
#3013 = VECTOR ( 'NONE', #11470, 1000.000000000000000 ) ;
#3014 = DIRECTION ( 'NONE',  ( 1.000000000000000000, 0.000000000000000000, 0.000000000000000000 ) ) ;
#3015 = CARTESIAN_POINT ( 'NONE',  ( 108.0825317500000011, 110.0000000000000000, -52.62499999726882294 ) ) ;
#3016 = CARTESIAN_POINT ( 'NONE',  ( -8.049105076161786076E-16, 33.40976562608393863, -13.14518615778179544 ) ) ;
#3017 = ORIENTED_EDGE ( 'NONE', *, *, #12292, .T. ) ;
#3018 = DIRECTION ( 'NONE',  ( -1.000000000000000000, 0.000000000000000000, 0.000000000000000000 ) ) ;
#3019 = CARTESIAN_POINT ( 'NONE',  ( 13.57481594606304753, 39.95820312716787726, -5.622872871577873966 ) ) ;
#3020 = CARTESIAN_POINT ( 'NONE',  ( 98.23223304703363112, 123.4000000021849530, -1.767766952966370209 ) ) ;
#3021 = CARTESIAN_POINT ( 'NONE',  ( 181.8548138422181921, 35.84062500108394289, 5.444914386472304635 ) ) ;
#3022 = VERTEX_POINT ( 'NONE', #19237 ) ;
#3023 = AXIS2_PLACEMENT_3D ( 'NONE', #19045, #7939, #21194 ) ;
#3024 = CARTESIAN_POINT ( 'NONE',  ( 188.1264917564332109, 51.14166184781122837, -15.00000000000000000 ) ) ;
#3025 = CARTESIAN_POINT ( 'NONE',  ( 99.99999999999995737, 4.458734125000016313, 9.437500001365593860 ) ) ;
#3026 = ORIENTED_EDGE ( 'NONE', *, *, #8370, .T. ) ;
#3027 = CARTESIAN_POINT ( 'NONE',  ( 95.00472066334982912, 116.8754121666685393, -53.67500000273118843 ) ) ;
#3028 = CARTESIAN_POINT ( 'NONE',  ( 5.444914386472302859, 36.03906250108394005, 13.14518615778179189 ) ) ;
#3029 = VECTOR ( 'NONE', #12708, 1000.000000000000000 ) ;
#3030 = CARTESIAN_POINT ( 'NONE',  ( 99.99999999999998579, 123.2000000000000028, -2.499999999999997780 ) ) ;
#3031 = CARTESIAN_POINT ( 'NONE',  ( 130.0000000000000000, -7.395377635281828788, -1.503427012513233026E-14 ) ) ;
#3032 = CARTESIAN_POINT ( 'NONE',  ( 124.5550856135277087, 39.11484375108394573, 13.14518615778179722 ) ) ;
#3033 = CARTESIAN_POINT ( 'NONE',  ( -8.049105076161786076E-16, 36.58476562608393579, -13.14518615778179544 ) ) ;
#3034 = CARTESIAN_POINT ( 'NONE',  ( -8.049105076161786076E-16, 35.59257812608393579, -13.14518615778179544 ) ) ;
#3035 = EDGE_CURVE ( 'NONE', #2357, #22244, #23661, .T. ) ;
#3036 = CARTESIAN_POINT ( 'NONE',  ( 96.84719886470463734, 92.18749999863440792, 3.152801135295351997 ) ) ;
#3037 = CARTESIAN_POINT ( 'NONE',  ( 64.12347373463796885, 51.45968077935077645, -15.00000000000135536 ) ) ;
#3038 = CARTESIAN_POINT ( 'NONE',  ( 102.4976396683250925, 102.3130555110000159, -50.77500000273119696 ) ) ;
#3039 = VERTEX_POINT ( 'NONE', #10804 ) ;
#3040 = CARTESIAN_POINT ( 'NONE',  ( 78.24545034676866351, 35.99999999999998579, 2.307131236161231058 ) ) ;
#3041 = CARTESIAN_POINT ( 'NONE',  ( 2.414731522848535132E-15, 36.98164062608393721, 13.14518615778179544 ) ) ;
#3042 = CARTESIAN_POINT ( 'NONE',  ( 99.99999999999995737, -4.458734124999988779, 8.937500001365592084 ) ) ;
#3043 = CIRCLE ( 'NONE', #20812, 4.999999999999989342 ) ;
#3044 = ADVANCED_FACE ( 'NONE', ( #6266 ), #5235, .T. ) ;
#3045 = CARTESIAN_POINT ( 'NONE',  ( 78.14518615778180788, 37.72578125108393010, 5.444914386472293977 ) ) ;
#3046 = CARTESIAN_POINT ( 'NONE',  ( 101.7677669529663547, 124.5000000000000000, 1.767766952966350891 ) ) ;
#3047 = CARTESIAN_POINT ( 'NONE',  ( 208.1451861577818079, 36.23750000108393010, -5.444914386472297529 ) ) ;
#3048 = EDGE_CURVE ( 'NONE', #22877, #5951, #10459, .T. ) ;
#3049 = CARTESIAN_POINT ( 'NONE',  ( 9.295050272127047819, 34.69960937608393436, 9.295050272127046043 ) ) ;
#3050 = VERTEX_POINT ( 'NONE', #19166 ) ;
#3051 = CARTESIAN_POINT ( 'NONE',  ( 97.93301269999999192, 123.0000000010925163, 0.8561741729129329626 ) ) ;
#3052 = CARTESIAN_POINT ( 'NONE',  ( 13.57481594606304931, 34.20351562499999432, 5.622872871577868636 ) ) ;
#3053 = CARTESIAN_POINT ( 'NONE',  ( 181.8548138422182205, 39.21406250108392300, 5.444914386472304635 ) ) ;
#3054 = CARTESIAN_POINT ( 'NONE',  ( 91.91746824999997045, 112.6261737610028320, -47.97499999726881725 ) ) ;
#3055 = ADVANCED_FACE ( 'NONE', ( #23175 ), #17026, .F. ) ;
#3056 = EDGE_LOOP ( 'NONE', ( #5747, #12969, #24221, #139 ) ) ;
#3057 = CARTESIAN_POINT ( 'NONE',  ( -9.598844408820454532, 33.16171874999999858, 9.598844408820459861 ) ) ;
#3058 = CARTESIAN_POINT ( 'NONE',  ( -13.14518615778179544, 32.61601562608393579, 0.000000000000000000 ) ) ;
#3059 = ORIENTED_EDGE ( 'NONE', *, *, #11234, .F. ) ;
#3060 = CARTESIAN_POINT ( 'NONE',  ( 139.2950502721270425, 32.31835937608393294, 9.295050272127046043 ) ) ;
#3061 = CARTESIAN_POINT ( 'NONE',  ( 99.99999999999995737, -4.999999999999990230, 0.3750000027311853890 ) ) ;
#3062 = ORIENTED_EDGE ( 'NONE', *, *, #25549, .T. ) ;
#3063 = EDGE_CURVE ( 'NONE', #10173, #13216, #16120, .T. ) ;
#3064 = CARTESIAN_POINT ( 'NONE',  ( 208.1451861577817795, 34.84843750108393579, -5.444914386472297529 ) ) ;
#3065 = EDGE_LOOP ( 'NONE', ( #7385, #8947, #22450, #3017 ) ) ;
#3066 = CARTESIAN_POINT ( 'NONE',  ( 99.99999999999998579, 123.5500000010924850, -2.066987299999998751 ) ) ;
#3067 = FACE_OUTER_BOUND ( 'NONE', #7175, .T. ) ;
#3068 = CARTESIAN_POINT ( 'NONE',  ( 101.7677669529663547, 123.8000000021849587, 1.767766952966350891 ) ) ;
#3069 = CARTESIAN_POINT ( 'NONE',  ( 116.4251840539369454, 36.28710937716787299, -5.622872871577873077 ) ) ;
#3070 = CARTESIAN_POINT ( 'NONE',  ( 91.91746824999998466, 112.6261737610028320, -49.22500000273119269 ) ) ;
#3071 =( BOUNDED_CURVE ( )  B_SPLINE_CURVE ( 2, ( #13512, #24360, #11230, #8436, #13656, #2568, #22371, #15660, #20094 ),
 .UNSPECIFIED., .F., .F. ) 
 B_SPLINE_CURVE_WITH_KNOTS ( ( 3, 2, 2, 2, 3 ),
 ( 0.6041666666666668517, 0.6145833333333334814, 0.6250000000000001110, 0.6354166666666667407, 0.6458333333333333703 ),
 .UNSPECIFIED. ) 
 CURVE ( )  GEOMETRIC_REPRESENTATION_ITEM ( )  RATIONAL_B_SPLINE_CURVE ( ( 0.9999999999999983347, 0.9238795325112884038, 1.000000000000000000, 0.9238795325112867385, 1.000000000000000000, 0.9238795325112867385, 1.000000000000000000, 0.9238795325112867385, 1.000000000000000000 ) ) 
 REPRESENTATION_ITEM ( '' )  );
#3072 = CARTESIAN_POINT ( 'NONE',  ( 3.100818213308542287E-15, 78.00000000000000000, 12.99999999999999645 ) ) ;
#3073 = CARTESIAN_POINT ( 'NONE',  ( -8.312177448680279460E-16, 32.16953125216787157, -13.57481594606304576 ) ) ;
#3074 = CARTESIAN_POINT ( 'NONE',  ( 189.5550856135277229, 39.80937500108392868, -13.14518615778179900 ) ) ;
#3075 = EDGE_CURVE ( 'NONE', #6277, #13578, #23004, .T. ) ;
#3076 = ORIENTED_EDGE ( 'NONE', *, *, #1856, .F. ) ;
#3077 = PRESENTATION_STYLE_ASSIGNMENT (( #806 ) ) ;
#3078 = CARTESIAN_POINT ( 'NONE',  ( 95.54126587499996504, 1.387778780781445676E-14, 6.437500001365592084 ) ) ;
#3079 = ORIENTED_EDGE ( 'NONE', *, *, #10203, .T. ) ;
#3080 = DIRECTION ( 'NONE',  ( -6.123233995736778362E-17, -0.8660254037844380415, -0.5000000000000009992 ) ) ;
#3081 = CARTESIAN_POINT ( 'NONE',  ( 96.84719886470459471, 3.152801135295383084, 9.312500001365593860 ) ) ;
#3082 = CARTESIAN_POINT ( 'NONE',  ( 139.5988444088204403, 38.42031250216787441, -9.598844408820458085 ) ) ;
#3083 = CARTESIAN_POINT ( 'NONE',  ( 0.7050241099689084079, 36.00000000000001421, 13.13343125082108820 ) ) ;
#3084 = CARTESIAN_POINT ( 'NONE',  ( 70.44491438647230552, 33.06250000108393294, 13.14518615778179189 ) ) ;
#3085 = SURFACE_STYLE_USAGE ( .BOTH. , #10036 ) ;
#3086 = EDGE_CURVE ( 'NONE', #19447, #4040, #3515, .T. ) ;
#3087 = VECTOR ( 'NONE', #22411, 1000.000000000000000 ) ;
#3088 = DIRECTION ( 'NONE',  ( 0.000000000000000000, 0.000000000000000000, 1.000000000000000000 ) ) ;
#3089 = CARTESIAN_POINT ( 'NONE',  ( -8.402315781222888802, 54.99999999485619639, 14.99999999999999822 ) ) ;
#3090 = CARTESIAN_POINT ( 'NONE',  ( 59.37712712842223794, 40.85117187499999147, -13.57481594606315412 ) ) ;
#3091 = CARTESIAN_POINT ( 'NONE',  ( 116.4251840539369596, 33.06249999999999289, 0.000000000000000000 ) ) ;
#3092 = EDGE_CURVE ( 'NONE', #27029, #27310, #25419, .T. ) ;
#3093 = ORIENTED_EDGE ( 'NONE', *, *, #13327, .F. ) ;
#3094 = FACE_BOUND ( 'NONE', #27669, .T. ) ;
#3095 = CARTESIAN_POINT ( 'NONE',  ( -5.444914386472297529, 33.45937500108394147, -13.14518615778179900 ) ) ;
#3096 = CARTESIAN_POINT ( 'NONE',  ( -5.622872871577873077, 34.60039062716786873, -13.57481594606304753 ) ) ;
#3097 = CARTESIAN_POINT ( 'NONE',  ( 96.46446609406721961, -3.535533905932727539, 10.25000000273118594 ) ) ;
#3098 = CARTESIAN_POINT ( 'NONE',  ( 143.1451861577818079, 33.80664062608393294, -1.609821015232357215E-15 ) ) ;
#3099 = PRODUCT_DEFINITION_SHAPE ( 'NONE', 'NONE',  #28204 ) ;
#3100 = CARTESIAN_POINT ( 'NONE',  ( 65.00000000000000000, 31.77265625216787370, 13.57481594606304576 ) ) ;
#3101 = CARTESIAN_POINT ( 'NONE',  ( 94.99999999999995737, 2.071067811865491493, 14.93749999999999822 ) ) ;
#3102 = CARTESIAN_POINT ( 'NONE',  ( -9.295050272127044266, 37.47773437608393010, 9.295050272127047819 ) ) ;
#3103 = CARTESIAN_POINT ( 'NONE',  ( -8.049105076161786076E-16, 33.40976562608393863, -13.14518615778179544 ) ) ;
#3104 = CARTESIAN_POINT ( 'NONE',  ( 93.00000000000002842, 112.2744378736303474, -48.10000000000000142 ) ) ;
#3105 = CARTESIAN_POINT ( 'NONE',  ( 2.493653234604083739E-15, 38.91640625216786731, 13.57481594606304576 ) ) ;
#3106 = CARTESIAN_POINT ( 'NONE',  ( 198.7556382656599396, 31.58960998161716560, -13.14518615778179900 ) ) ;
#3107 = CARTESIAN_POINT ( 'NONE',  ( -8.312177448680279460E-16, 31.37578125216787583, -13.57481594606304576 ) ) ;
#3108 = CARTESIAN_POINT ( 'NONE',  ( 97.83688103937537051, 103.3426043859339103, -52.60000000000001563 ) ) ;
#3109 = CARTESIAN_POINT ( 'NONE',  ( 99.99999999999998579, 123.1500000010924794, 2.066987299999980099 ) ) ;
#3110 = CARTESIAN_POINT ( 'NONE',  ( 127.9130013513679103, 36.00000000000000711, -13.31420566034935327 ) ) ;
#3111 = CARTESIAN_POINT ( 'NONE',  ( 94.99999999999995737, 1.387778780781445676E-14, 10.12500000273118594 ) ) ;
#3112 = AXIS2_PLACEMENT_3D ( 'NONE', #22004, #26823, #8883 ) ;
#3113 = CARTESIAN_POINT ( 'NONE',  ( 94.99999999999995737, 2.071067811865491493, 12.93750000000000000 ) ) ;
#3114 = CARTESIAN_POINT ( 'NONE',  ( 13.57481594606304576, 35.04687499999999289, -1.662435489736055892E-15 ) ) ;
#3115 = CARTESIAN_POINT ( 'NONE',  ( 1.662435489736055892E-15, 40.99999999999999289, 13.57481594606304576 ) ) ;
#3116 = CARTESIAN_POINT ( 'NONE',  ( -13.14518615778179900, 32.76484375108393010, -5.444914386472297529 ) ) ;
#3117 = CARTESIAN_POINT ( 'NONE',  ( -5.444914386472299306, 33.55859375108393294, 13.14518615778179722 ) ) ;
#3118 = CARTESIAN_POINT ( 'NONE',  ( 189.3771271284221314, 32.41757812499999858, 13.57481594606304753 ) ) ;
#3119 = EDGE_CURVE ( 'NONE', #23148, #6493, #15165, .T. ) ;
#3120 = CARTESIAN_POINT ( 'NONE',  ( -13.57481594606304753, 36.28710937716787299, -5.622872871577873077 ) ) ;
#3121 = CARTESIAN_POINT ( 'NONE',  ( -8.312177448680279460E-16, 37.72578125216787726, -13.57481594606304576 ) ) ;
#3122 = CARTESIAN_POINT ( 'NONE',  ( 95.54126587499996504, 83.43750000136560629, -1.387778780781445676E-14 ) ) ;
#3123 = CARTESIAN_POINT ( 'NONE',  ( 55.70494972787295751, 31.92148437608393508, 9.295050272127047819 ) ) ;
#3124 =( BOUNDED_CURVE ( )  B_SPLINE_CURVE ( 2, ( #18841, #23130, #10129, #27549, #21834, #19263, #4441, #8848, #27963 ),
 .UNSPECIFIED., .F., .F. ) 
 B_SPLINE_CURVE_WITH_KNOTS ( ( 3, 2, 2, 2, 3 ),
 ( 0.06250000000000004163, 0.07291666666666665741, 0.08333333333333325932, 0.09374999999999987510, 0.1041666666666664909 ),
 .UNSPECIFIED. ) 
 CURVE ( )  GEOMETRIC_REPRESENTATION_ITEM ( )  RATIONAL_B_SPLINE_CURVE ( ( 0.9999999999999996669, 0.9238795325112870716, 1.000000000000000000, 0.9238795325112867385, 1.000000000000000000, 0.9238795325112867385, 1.000000000000000000, 0.9238795325112880708, 0.9999999999999986677 ) ) 
 REPRESENTATION_ITEM ( '' )  );
#3125 = CARTESIAN_POINT ( 'NONE',  ( 95.27063293749995410, 1.387778780781445676E-14, 14.84375000068279604 ) ) ;
#3126 = CARTESIAN_POINT ( 'NONE',  ( 101.5628473693180069, 123.0000000000000000, 1.972588198814292593 ) ) ;
#3127 = ORIENTED_EDGE ( 'NONE', *, *, #27642, .F. ) ;
#3128 = CARTESIAN_POINT ( 'NONE',  ( 120.4011555911795455, 38.02343750216788010, 9.598844408820459861 ) ) ;
#3129 = CARTESIAN_POINT ( 'NONE',  ( -9.598844408820454532, 33.95546874999999432, 9.598844408820459861 ) ) ;
#3130 = CARTESIAN_POINT ( 'NONE',  ( 108.0825317500000011, 110.0000000000000000, -54.87499999726882294 ) ) ;
#3131 = CARTESIAN_POINT ( 'NONE',  ( 143.1451861577818079, 33.26093750108393721, -5.444914386472297529 ) ) ;
#3132 = VERTEX_POINT ( 'NONE', #15259 ) ;
#3133 = CARTESIAN_POINT ( 'NONE',  ( 103.1528011352953342, 84.06250000136560629, -3.152801135295383084 ) ) ;
#3134 = CARTESIAN_POINT ( 'NONE',  ( 99.99999999999998579, 94.25000000000000000, -4.999999999999997335 ) ) ;
#3135 = CARTESIAN_POINT ( 'NONE',  ( 55.40115559117954547, 38.81718750216787583, 9.598844408820459861 ) ) ;
#3136 = VECTOR ( 'NONE', #19620, 999.9999999999998863 ) ;
#3137 = CIRCLE ( 'NONE', #13520, 0.5000000000000086597 ) ;
#3138 = CARTESIAN_POINT ( 'NONE',  ( 95.00472066334982912, 103.1245878333314323, -47.32499999726881157 ) ) ;
#3139 = CARTESIAN_POINT ( 'NONE',  ( 185.7049497278729575, 39.06523437608392868, -9.295050272127046043 ) ) ;
#3140 = AXIS2_PLACEMENT_3D ( 'NONE', #24486, #843, #9516 ) ;
#3141 = FACE_OUTER_BOUND ( 'NONE', #14026, .T. ) ;
#3142 = VERTEX_POINT ( 'NONE', #19836 ) ;
#3143 = CARTESIAN_POINT ( 'NONE',  ( 183.3096217544866420, 35.99999999999998579, -6.307928093363108779 ) ) ;
#3144 = CARTESIAN_POINT ( 'NONE',  ( 94.99999999999995737, 1.387778780781445676E-14, 12.00000000000000000 ) ) ;
#3145 = ORIENTED_EDGE ( 'NONE', *, *, #25061, .T. ) ;
#3146 = CARTESIAN_POINT ( 'NONE',  ( -5.444914386472299306, 36.13828125108393863, 13.14518615778179722 ) ) ;
#3147 = APPLICATION_CONTEXT ( 'automotive_design' ) ;
#3148 = CARTESIAN_POINT ( 'NONE',  ( 204.2950502721270425, 39.46210937608393010, -9.295050272127046043 ) ) ;
#3149 = CARTESIAN_POINT ( 'NONE',  ( -8.049105076161786076E-16, 32.41757812608393863, -13.14518615778179544 ) ) ;
#3150 = CARTESIAN_POINT ( 'NONE',  ( 97.92893218813451028, 5.000000000000018652, 0.9375000027311859441 ) ) ;
#3151 = CARTESIAN_POINT ( 'NONE',  ( 130.0000000000000000, 32.41757812608393863, -13.14518615778179544 ) ) ;
#3152 = CARTESIAN_POINT ( 'NONE',  ( 104.4587341249999923, 92.24999999863439371, 1.846868145590726318 ) ) ;
#3153 = CARTESIAN_POINT ( 'NONE',  ( 102.0669872999999797, 122.7500000010924737, -9.794112055954760458E-15 ) ) ;
#3154 = CARTESIAN_POINT ( 'NONE',  ( 5.622872871578008080, 36.08867187716787583, -13.57481594606290898 ) ) ;
#3155 = CARTESIAN_POINT ( 'NONE',  ( 104.4587341249999639, 1.442382525525748735E-14, 6.187500001365592084 ) ) ;
#3156 = CARTESIAN_POINT ( 'NONE',  ( -9.598844408820458085, 37.82500000216787583, -9.598844408820458085 ) ) ;
#3157 = CARTESIAN_POINT ( 'NONE',  ( 95.54126587499996504, 1.846868145590750077, 11.37500000136559208 ) ) ;
#3158 = CARTESIAN_POINT ( 'NONE',  ( 102.4976396683250925, 102.3130555110000159, -48.52500000273119696 ) ) ;
#3159 = CARTESIAN_POINT ( 'NONE',  ( 104.4587341249999781, 90.56249999863440792, -6.938893903907228378E-15 ) ) ;
#3160 = CARTESIAN_POINT ( 'NONE',  ( 104.9999999999999716, 83.56250000273119838, 2.071067811865462627 ) ) ;
#3161 = CARTESIAN_POINT ( 'NONE',  ( 106.5389055433250860, 105.2492070361643215, -54.82499999726882578 ) ) ;
#3162 = CARTESIAN_POINT ( 'NONE',  ( -5.444914386472297529, 33.45937500108394147, -13.14518615778179900 ) ) ;
#3163 = ORIENTED_EDGE ( 'NONE', *, *, #26053, .F. ) ;
#3164 = DIRECTION ( 'NONE',  ( -0.000000000000000000, -0.000000000000000000, -1.000000000000000000 ) ) ;
#3165 = CARTESIAN_POINT ( 'NONE',  ( 98.23223304703363112, 123.6000000021849416, 1.767766952966351557 ) ) ;
#3166 = CARTESIAN_POINT ( 'NONE',  ( 208.1451861577818079, 36.98164062608393010, -1.609821015232357215E-15 ) ) ;
#3167 = ORIENTED_EDGE ( 'NONE', *, *, #13236, .F. ) ;
#3168 = CARTESIAN_POINT ( 'NONE',  ( 104.9999999999999716, 1.449011120738813565E-14, 34.79898987322334136 ) ) ;
#3169 = CARTESIAN_POINT ( 'NONE',  ( 104.4587341249999639, 1.442382525525748735E-14, 11.18750000136559208 ) ) ;
#3170 = EDGE_CURVE ( 'NONE', #4566, #13199, #10297, .T. ) ;
#3171 = VERTEX_POINT ( 'NONE', #13110 ) ;
#3172 = CARTESIAN_POINT ( 'NONE',  ( 99.99999999999998579, 101.5015231886685854, -46.87500000273119838 ) ) ;
#3173 = CARTESIAN_POINT ( 'NONE',  ( 2.414731522848535132E-15, 37.57695312608392868, 13.14518615778179544 ) ) ;
#3174 = VECTOR ( 'NONE', #19468, 1000.000000000000000 ) ;
#3175 = CARTESIAN_POINT ( 'NONE',  ( 99.99999999999998579, 90.00000000000000000, -6.938893903907228378E-15 ) ) ;
#3176 = DIRECTION ( 'NONE',  ( -0.000000000000000000, 1.000000000000000000, -0.000000000000000000 ) ) ;
#3177 = AXIS2_PLACEMENT_3D ( 'NONE', #16031, #18612, #7910 ) ;
#3178 = CARTESIAN_POINT ( 'NONE',  ( 116.8548138422182063, 38.22187500108393010, 5.444914386472304635 ) ) ;
#3179 = CARTESIAN_POINT ( 'NONE',  ( -5.444914386472297529, 38.22187500108393721, -13.14518615778179722 ) ) ;
#3180 = CARTESIAN_POINT ( 'NONE',  ( 9.295050272127046043, 36.28710937608393294, -9.295050272127046043 ) ) ;
#3181 = CARTESIAN_POINT ( 'NONE',  ( 104.4587341249999781, 91.56249999863440792, -6.938893903907228378E-15 ) ) ;
#3182 = PLANE ( 'NONE',  #8234 ) ;
#3183 = CARTESIAN_POINT ( 'NONE',  ( 91.91746824999998466, 107.3738262389971680, -51.27500000273119696 ) ) ;
#3184 = DIRECTION ( 'NONE',  ( 0.000000000000000000, -1.000000000000000000, -0.000000000000000000 ) ) ;
#3185 = CARTESIAN_POINT ( 'NONE',  ( -5.444914386472299306, 35.34453125108393579, 13.14518615778179722 ) ) ;
#3186 = CARTESIAN_POINT ( 'NONE',  ( 99.99999999999995737, -4.458734124999988779, 5.937500001365592084 ) ) ;
#3187 = CARTESIAN_POINT ( 'NONE',  ( 51.85481384221820633, 36.58476562608393579, 0.000000000000000000 ) ) ;
#3188 = CARTESIAN_POINT ( 'NONE',  ( -20.00000000000000355, 55.00000000000000000, -14.99999999999999822 ) ) ;
#3189 = CARTESIAN_POINT ( 'NONE',  ( 189.5550856135277229, 36.73359375108393010, 13.14518615778179722 ) ) ;
#3190 = CARTESIAN_POINT ( 'NONE',  ( 13.14518615778179722, 35.54296875108394715, 5.444914386472293977 ) ) ;
#3191 = CARTESIAN_POINT ( 'NONE',  ( 102.4999999999999716, 122.3500000021849701, -1.035533905932742638 ) ) ;
#3192 = CARTESIAN_POINT ( 'NONE',  ( 95.54126587499999346, 90.99999999863439371, -1.846868145590737864 ) ) ;
#3193 = CARTESIAN_POINT ( 'NONE',  ( 208.1451861577818079, 37.97382812608393721, -1.609821015232357215E-15 ) ) ;
#3194 = CARTESIAN_POINT ( 'NONE',  ( 104.9952793366501709, 116.8754121666685393, -52.57499999726881867 ) ) ;
#3195 = AXIS2_PLACEMENT_3D ( 'NONE', #5511, #7486, #9902 ) ;
#3196 = CARTESIAN_POINT ( 'NONE',  ( 5.622872871577878406, 34.10429687499999574, 13.57481594606304576 ) ) ;
#3197 = CARTESIAN_POINT ( 'NONE',  ( -5.444914386472297529, 34.84843750108393579, -13.14518615778179900 ) ) ;
#3198 = ORIENTED_EDGE ( 'NONE', *, *, #22826, .F. ) ;
#3199 = CARTESIAN_POINT ( 'NONE',  ( 208.5748159460630688, 37.47773437716787015, 5.622872871577868636 ) ) ;
#3200 = CARTESIAN_POINT ( 'NONE',  ( 51.85481384221820633, 39.90859375108393436, -5.444914386472297529 ) ) ;
#3201 = CARTESIAN_POINT ( 'NONE',  ( 102.0669873000000081, 122.8000000010924708, -0.8561741729129508371 ) ) ;
#3202 = CARTESIAN_POINT ( 'NONE',  ( 200.4449143864723055, 34.15390625108393863, -13.14518615778179900 ) ) ;
#3203 = ORIENTED_EDGE ( 'NONE', *, *, #23415, .F. ) ;
#3204 = CARTESIAN_POINT ( 'NONE',  ( 102.0710678118654329, -4.999999999999989342, 13.31250000000000000 ) ) ;
#3205 = CARTESIAN_POINT ( 'NONE',  ( 96.46446609406726225, 91.49999999726880162, 3.535533905932723986 ) ) ;
#3206 = CARTESIAN_POINT ( 'NONE',  ( 195.3247243111960643, 53.49346745874645137, 14.99999999999994849 ) ) ;
#3207 = ADVANCED_FACE ( 'NONE', ( #323 ), #17413, .F. ) ;
#3208 = CARTESIAN_POINT ( 'NONE',  ( 135.6228728715778686, 37.67617187716787441, -13.57481594606304753 ) ) ;
#3209 = ADVANCED_FACE ( 'NONE', ( #19413 ), #19987, .F. ) ;
#3210 = DIRECTION ( 'NONE',  ( 0.000000000000000000, 0.000000000000000000, 1.000000000000000000 ) ) ;
#3211 = CARTESIAN_POINT ( 'NONE',  ( -13.57481594606304576, 34.74921875216787726, 0.000000000000000000 ) ) ;
#3212 = CARTESIAN_POINT ( 'NONE',  ( 7.095735352922348582, 31.91687086491026193, -11.40432286404674933 ) ) ;
#3213 = ORIENTED_EDGE ( 'NONE', *, *, #2418, .T. ) ;
#3214 = CIRCLE ( 'NONE', #2307, 5.000000000000000888 ) ;
#3215 =( NAMED_UNIT ( * ) SI_UNIT ( $, .STERADIAN. ) SOLID_ANGLE_UNIT ( ) );
#3216 = CARTESIAN_POINT ( 'NONE',  ( 99.99999999999995737, -4.458734124999988779, 3.687500001365591640 ) ) ;
#3217 = EDGE_LOOP ( 'NONE', ( #4056, #18192, #15839, #9906 ) ) ;
#3218 = CARTESIAN_POINT ( 'NONE',  ( 99.99999999999995737, 4.458734125000016313, 5.187500001365592972 ) ) ;
#3219 = CARTESIAN_POINT ( 'NONE',  ( 12.07727640983550188, 36.00000000000000000, -6.197985357349471869 ) ) ;
#3220 = ADVANCED_FACE ( 'NONE', ( #28116 ), #21564, .F. ) ;
#3221 = CARTESIAN_POINT ( 'NONE',  ( 104.9999999999999858, 94.87499999726881583, -6.938893903907228378E-15 ) ) ;
#3222 = CARTESIAN_POINT ( 'NONE',  ( 51.85481384221820633, 33.60820312608393579, 0.000000000000000000 ) ) ;
#3223 = CARTESIAN_POINT ( 'NONE',  ( 99.99999999999998579, 92.12499999726880162, -4.999999999999997335 ) ) ;
#3224 = CARTESIAN_POINT ( 'NONE',  ( 91.91746824999998466, 112.6261737610028320, -45.22500000273119980 ) ) ;
#3225 = CARTESIAN_POINT ( 'NONE',  ( 99.99999999999998579, 123.2000000000000028, -2.499999999999997780 ) ) ;
#3226 = CARTESIAN_POINT ( 'NONE',  ( 5.622872871577825116, 35.29492187716787299, -13.57481594606309372 ) ) ;
#3227 = CARTESIAN_POINT ( 'NONE',  ( 1.505492181556994380, 53.60078691996478284, 14.99999999999999645 ) ) ;
#3228 = CARTESIAN_POINT ( 'NONE',  ( -15.00000000000000355, 55.00000000000000000, -9.999999999999998224 ) ) ;
#3229 = CARTESIAN_POINT ( 'NONE',  ( 130.0000000000000000, 32.86406249999999574, -13.57481594606304576 ) ) ;
#3230 = ORIENTED_EDGE ( 'NONE', *, *, #9027, .T. ) ;
#3231 = CARTESIAN_POINT ( 'NONE',  ( 104.9999999999999716, 84.43750000000000000, 2.071067811865462627 ) ) ;
#3232 = CARTESIAN_POINT ( 'NONE',  ( -13.14518615778179900, 35.14609375108393152, -5.444914386472297529 ) ) ;
#3233 = CARTESIAN_POINT ( 'NONE',  ( 5.622872871577878406, 32.61601562716786873, 13.57481594606304576 ) ) ;
#3234 =( BOUNDED_CURVE ( )  B_SPLINE_CURVE ( 2, ( #3121, #18074, #22220, #20512, #994, #18365, #24919, #1135, #5403 ),
 .UNSPECIFIED., .F., .F. ) 
 B_SPLINE_CURVE_WITH_KNOTS ( ( 3, 2, 2, 2, 3 ),
 ( 0.2708333333333330928, 0.2812499999999998890, 0.2916666666666666852, 0.3020833333333334259, 0.3125000000000002220 ),
 .UNSPECIFIED. ) 
 CURVE ( )  GEOMETRIC_REPRESENTATION_ITEM ( )  RATIONAL_B_SPLINE_CURVE ( ( 1.000000000000001554, 0.9238795325112850731, 1.000000000000000000, 0.9238795325112867385, 1.000000000000000000, 0.9238795325112867385, 1.000000000000000000, 0.9238795325112850731, 1.000000000000001554 ) ) 
 REPRESENTATION_ITEM ( '' )  );
#3235 = CARTESIAN_POINT ( 'NONE',  ( 99.99999999999995737, 5.000000000000018652, 5.875000002731185056 ) ) ;
#3236 = CARTESIAN_POINT ( 'NONE',  ( 130.0000000000000000, 32.02070312608393010, 13.14518615778179544 ) ) ;
#3237 = CARTESIAN_POINT ( 'NONE',  ( 51.85481384221820633, 38.96601562608393721, 0.000000000000000000 ) ) ;
#3238 = VECTOR ( 'NONE', #7754, 1000.000000000000000 ) ;
#3239 = CARTESIAN_POINT ( 'NONE',  ( 102.0669872999999797, 122.7500000010924737, -9.794112055954760458E-15 ) ) ;
#3240 = CARTESIAN_POINT ( 'NONE',  ( 9.295050272127047819, 38.46992187608393010, 9.295050272127046043 ) ) ;
#3241 = ADVANCED_FACE ( 'NONE', ( #15115 ), #2025, .F. ) ;
#3242 = ADVANCED_FACE ( 'NONE', ( #15548 ), #6718, .F. ) ;
#3243 = CARTESIAN_POINT ( 'NONE',  ( -9.295050272127044266, 33.70742187608393436, 9.295050272127047819 ) ) ;
#3244 = CARTESIAN_POINT ( 'NONE',  ( 94.33688103937537051, 114.1144967660473242, -48.20000000000000995 ) ) ;
#3245 = LINE ( 'NONE', #19033, #4898 ) ;
#3246 = VECTOR ( 'NONE', #5356, 1000.000000000000000 ) ;
#3247 = CARTESIAN_POINT ( 'NONE',  ( -8.312177448680279460E-16, 39.31328125216787583, -13.57481594606304576 ) ) ;
#3248 = CARTESIAN_POINT ( 'NONE',  ( 104.9999999999999716, 82.68750000273119838, -2.071067811865491937 ) ) ;
#3249 = DIRECTION ( 'NONE',  ( 0.8660254037844407060, 0.4999999999999963363, 0.000000000000000000 ) ) ;
#3250 = CARTESIAN_POINT ( 'NONE',  ( 99.99999999999998579, 138.0000000000000000, -5.204170427930421283E-15 ) ) ;
#3251 = EDGE_CURVE ( 'NONE', #23528, #10223, #4739, .T. ) ;
#3252 = FILL_AREA_STYLE ('',( #15779 ) ) ;
#3253 = CARTESIAN_POINT ( 'NONE',  ( 105.6631189606246153, 114.1144967660473242, -51.29999999453763593 ) ) ;
#3254 = CARTESIAN_POINT ( 'NONE',  ( 97.83688103937537051, 103.3426043859339103, -47.60000000000000142 ) ) ;
#3255 = CARTESIAN_POINT ( 'NONE',  ( 102.4999999999999858, 123.0500000021849587, 1.035533905932722876 ) ) ;
#3256 = CARTESIAN_POINT ( 'NONE',  ( -13.57481594606304576, 33.11210937499999574, 5.622872871577880183 ) ) ;
#3257 = CARTESIAN_POINT ( 'NONE',  ( -7.394032042335738630, 36.00000000000004263, -11.20317769887113180 ) ) ;
#3258 = CARTESIAN_POINT ( 'NONE',  ( -13.14518615778179189, 33.65781250108393152, 5.444914386472304635 ) ) ;
#3259 = CARTESIAN_POINT ( 'NONE',  ( -13.14518615778179544, 31.82226562608393650, 0.000000000000000000 ) ) ;
#3260 = EDGE_CURVE ( 'NONE', #17753, #21288, #13398, .T. ) ;
#3261 = CARTESIAN_POINT ( 'NONE',  ( -13.57481594606304576, 35.54296875216788010, 0.000000000000000000 ) ) ;
#3262 = CARTESIAN_POINT ( 'NONE',  ( 2.493653234604083739E-15, 38.12265625216787157, 13.57481594606304576 ) ) ;
#3263 = CARTESIAN_POINT ( 'NONE',  ( 104.4587341249999639, 82.93750000136560629, -1.442382525525748735E-14 ) ) ;
#3264 = CARTESIAN_POINT ( 'NONE',  ( 70.44491438647230552, 33.16171875108393152, -13.14518615778179900 ) ) ;
#3265 = LINE ( 'NONE', #9245, #8019 ) ;
#3266 = CARTESIAN_POINT ( 'NONE',  ( 0.000000000000000000, 10.00000000000000000, 0.000000000000000000 ) ) ;
#3267 = CARTESIAN_POINT ( 'NONE',  ( 9.598844408820459861, 37.32890624999999574, 9.598844408820456309 ) ) ;
#3268 = CARTESIAN_POINT ( 'NONE',  ( -9.598844408820458085, 34.55078124999999289, -9.598844408820458085 ) ) ;
#3269 = CARTESIAN_POINT ( 'NONE',  ( 91.91746824999998466, 110.0000000000000000, -53.87499999726882294 ) ) ;
#3270 = CARTESIAN_POINT ( 'NONE',  ( 124.5550856135277087, 34.25312500108393010, -13.14518615778179900 ) ) ;
#3271 = ORIENTED_EDGE ( 'NONE', *, *, #20663, .F. ) ;
#3272 = CARTESIAN_POINT ( 'NONE',  ( 107.0000000000000142, 110.0000000000000000, -51.00000000000000711 ) ) ;
#3273 = CARTESIAN_POINT ( 'NONE',  ( 208.5748159460630688, 36.68398437716787441, 5.622872871577868636 ) ) ;
#3274 = CARTESIAN_POINT ( 'NONE',  ( 94.99999999999995737, 80.06250000273118417, -2.071067811865491048 ) ) ;
#3275 = CARTESIAN_POINT ( 'NONE',  ( 96.46446609406726225, 91.37500000000000000, -3.535533905932738197 ) ) ;
#3276 = CARTESIAN_POINT ( 'NONE',  ( 87.00000000000000000, 102.0000000000000142, -15.00000000000000711 ) ) ;
#3277 = CARTESIAN_POINT ( 'NONE',  ( 107.0000000000000000, 110.0000000000000000, -54.00000000000001421 ) ) ;
#3278 = CARTESIAN_POINT ( 'NONE',  ( 181.8548138422182205, 31.82226562608393650, 0.000000000000000000 ) ) ;
#3279 = CARTESIAN_POINT ( 'NONE',  ( -13.57481594606304576, 39.51171875216787299, 0.000000000000000000 ) ) ;
#3280 = VERTEX_POINT ( 'NONE', #10981 ) ;
#3281 = CARTESIAN_POINT ( 'NONE',  ( 96.46446609406721961, -3.535533905932727539, 9.125000000000000000 ) ) ;
#3282 = ORIENTED_EDGE ( 'NONE', *, *, #451, .F. ) ;
#3283 = CARTESIAN_POINT ( 'NONE',  ( 2.414731522848535132E-15, 32.21914062608393436, 13.14518615778179544 ) ) ;
#3284 = CARTESIAN_POINT ( 'NONE',  ( 181.8548138422181921, 40.50390625108394005, -5.444914386472297529 ) ) ;
#3285 = CARTESIAN_POINT ( 'NONE',  ( 2.493653234604083739E-15, 36.53515625216787299, 13.57481594606304576 ) ) ;
#3286 = EDGE_CURVE ( 'NONE', #144, #21487, #180, .T. ) ;
#3287 = CARTESIAN_POINT ( 'NONE',  ( 102.0710678118654329, 5.000000000000018652, 11.81250000273118772 ) ) ;
#3288 = CARTESIAN_POINT ( 'NONE',  ( 195.0000000000000000, 38.12265625216787157, 13.57481594606304576 ) ) ;
#3289 = CARTESIAN_POINT ( 'NONE',  ( 2.414731522848535132E-15, 32.21914062608393436, 13.14518615778179544 ) ) ;
#3290 =( BOUNDED_CURVE ( )  B_SPLINE_CURVE ( 2, ( #3682, #23478, #5684, #3393, #8358, #12346, #25607, #3958, #14350 ),
 .UNSPECIFIED., .F., .F. ) 
 B_SPLINE_CURVE_WITH_KNOTS ( ( 3, 2, 2, 2, 3 ),
 ( 0.8571428571428570953, 0.8660714285714286031, 0.8750000000000000000, 0.8839285714285712858, 0.8928571428571427937 ),
 .UNSPECIFIED. ) 
 CURVE ( )  GEOMETRIC_REPRESENTATION_ITEM ( )  RATIONAL_B_SPLINE_CURVE ( ( 1.000000000000000000, 0.9238795325112867385, 1.000000000000000000, 0.9238795325112867385, 1.000000000000000000, 0.9238795325112867385, 1.000000000000000000, 0.9238795325112877377, 0.9999999999999990008 ) ) 
 REPRESENTATION_ITEM ( '' )  );
#3291 = CARTESIAN_POINT ( 'NONE',  ( 94.99999999999995737, 1.387778780781445676E-14, 12.12500000273118594 ) ) ;
#3292 = CARTESIAN_POINT ( 'NONE',  ( 59.37712712842213136, 32.91367187499999858, -13.57481594606304753 ) ) ;
#3293 = CARTESIAN_POINT ( 'NONE',  ( 97.50000000000000000, 124.2000000000000028, -9.540979117872439019E-15 ) ) ;
#3294 = DIRECTION ( 'NONE',  ( 0.000000000000000000, 0.000000000000000000, 1.000000000000000000 ) ) ;
#3295 = CARTESIAN_POINT ( 'NONE',  ( 70.62287287157795390, 36.58476562716786873, 13.57481594606297115 ) ) ;
#3296 = CARTESIAN_POINT ( 'NONE',  ( 98.15313185440925281, -4.458734124999987891, 6.875000001365592972 ) ) ;
#3297 = CARTESIAN_POINT ( 'NONE',  ( 102.1631189606246295, 116.6573956140660897, -53.10000000546238397 ) ) ;
#3298 = CARTESIAN_POINT ( 'NONE',  ( 96.84719886470459471, -3.152801135295355994, 8.562500001365592084 ) ) ;
#3299 = CARTESIAN_POINT ( 'NONE',  ( 104.3262379212492590, 104.0454443415356991, -47.80000000546237970 ) ) ;
#3300 = CARTESIAN_POINT ( 'NONE',  ( 95.54126587499999346, 92.12499999863437949, 1.846868145590722543 ) ) ;
#3301 = CARTESIAN_POINT ( 'NONE',  ( 94.99999999999995737, 1.387778780781445676E-14, 9.000000000000000000 ) ) ;
#3302 = CARTESIAN_POINT ( 'NONE',  ( 91.91746824999998466, 110.0000000000000000, -53.62499999726882294 ) ) ;
#3303 = CARTESIAN_POINT ( 'NONE',  ( -9.295050272127046043, 32.71523437608393436, -9.295050272127046043 ) ) ;
#3304 = ORIENTED_EDGE ( 'NONE', *, *, #1152, .T. ) ;
#3305 = CARTESIAN_POINT ( 'NONE',  ( 124.3771271284221740, 37.18007812499999432, 13.57481594606311504 ) ) ;
#3306 = LINE ( 'NONE', #7423, #15196 ) ;
#3307 = AXIS2_PLACEMENT_3D ( 'NONE', #21369, #2118, #28196 ) ;
#3308 = CARTESIAN_POINT ( 'NONE',  ( 208.1451861577817795, 33.06250000108393294, -5.444914386472297529 ) ) ;
#3309 = ORIENTED_EDGE ( 'NONE', *, *, #27913, .T. ) ;
#3310 = CARTESIAN_POINT ( 'NONE',  ( 186.7985538123501215, 50.69246985422704910, -14.99999999999999822 ) ) ;
#3311 = CARTESIAN_POINT ( 'NONE',  ( 101.8468681455906903, -4.458734124999987891, 6.000000001365591196 ) ) ;
#3312 = ORIENTED_EDGE ( 'NONE', *, *, #1027, .T. ) ;
#3313 = CARTESIAN_POINT ( 'NONE',  ( 104.9952793366501851, 103.1245878333314323, -44.67500000273118843 ) ) ;
#3314 = CARTESIAN_POINT ( 'NONE',  ( -8.049105076161786076E-16, 36.38632812608393152, -13.14518615778179544 ) ) ;
#3315 = CARTESIAN_POINT ( 'NONE',  ( 181.4251840539369596, 40.25585937716787299, -5.622872871577873077 ) ) ;
#3316 = DIRECTION ( 'NONE',  ( 5.782411586589357392E-17, -0.000000000000000000, 1.000000000000000000 ) ) ;
#3317 = CARTESIAN_POINT ( 'NONE',  ( 143.1451861577818079, 37.03125000108393294, -5.444914386472297529 ) ) ;
#3318 = CARTESIAN_POINT ( 'NONE',  ( -13.14518615778179544, 39.16445312608393436, 0.000000000000000000 ) ) ;
#3319 = CARTESIAN_POINT ( 'NONE',  ( -8.049105076161786076E-16, 40.55351562608393579, -13.14518615778179544 ) ) ;
#3320 = CARTESIAN_POINT ( 'NONE',  ( 99.99999999999998579, 93.81249999863440792, -4.458734124999994997 ) ) ;
#3321 = DIRECTION ( 'NONE',  ( -0.000000000000000000, 1.000000000000000000, -0.000000000000000000 ) ) ;
#3322 = CARTESIAN_POINT ( 'NONE',  ( 104.3262379212492448, 104.0454443415356991, -50.30000000000001137 ) ) ;
#3323 = CARTESIAN_POINT ( 'NONE',  ( -9.295050272127044266, 32.11992187608393579, 9.295050272127047819 ) ) ;
#3324 = CARTESIAN_POINT ( 'NONE',  ( 103.1528011352953342, -3.152801135295355106, 6.062500001365592084 ) ) ;
#3325 = CARTESIAN_POINT ( 'NONE',  ( -8.312177448680279460E-16, 33.65781249999999147, -13.57481594606304576 ) ) ;
#3326 = CARTESIAN_POINT ( 'NONE',  ( 195.0000000000000000, 36.00000000000000000, -2.255140518769849538E-14 ) ) ;
#3327 = CARTESIAN_POINT ( 'NONE',  ( 0.000000000000000000, -7.395377635281828788, 0.000000000000000000 ) ) ;
#3328 = CARTESIAN_POINT ( 'NONE',  ( 204.2950502721270425, 36.08867187608392868, 9.295050272127046043 ) ) ;
#3329 = VERTEX_POINT ( 'NONE', #11266 ) ;
#3330 = CARTESIAN_POINT ( 'NONE',  ( -13.14518615778179189, 35.24531250108393721, 5.444914386472304635 ) ) ;
#3331 = EDGE_CURVE ( 'NONE', #16904, #8652, #25972, .T. ) ;
#3332 = CARTESIAN_POINT ( 'NONE',  ( 102.0669872999999939, 123.3000000010924850, 0.8561741729129311862 ) ) ;
#3333 = CARTESIAN_POINT ( 'NONE',  ( 99.99999999999998579, 93.31249999863440792, 4.458734124999981674 ) ) ;
#3334 = CARTESIAN_POINT ( 'NONE',  ( 182.3184072029388005, 36.04503594658365984, 5.908507747192915716 ) ) ;
#3335 = CARTESIAN_POINT ( 'NONE',  ( 104.9952793366501709, 116.8754121666685393, -46.57499999726881157 ) ) ;
#3336 = CYLINDRICAL_SURFACE ( 'NONE', #25938, 9.000000000000007105 ) ;
#3337 = VERTEX_POINT ( 'NONE', #15403 ) ;
#3338 = DIRECTION ( 'NONE',  ( -0.000000000000000000, 1.000000000000000000, -0.000000000000000000 ) ) ;
#3339 = CARTESIAN_POINT ( 'NONE',  ( 65.00000000000000000, 31.62382812608393579, -13.14518615778179544 ) ) ;
#3340 = VERTEX_POINT ( 'NONE', #24117 ) ;
#3341 = CARTESIAN_POINT ( 'NONE',  ( 9.598844408820459861, 32.66562500216787157, 9.598844408820456309 ) ) ;
#3342 = CIRCLE ( 'NONE', #13770, 12.50000000000001599 ) ;
#3343 = CARTESIAN_POINT ( 'NONE',  ( 204.2950502721270425, 33.11210937608393579, 9.295050272127046043 ) ) ;
#3344 = ORIENTED_EDGE ( 'NONE', *, *, #18362, .T. ) ;
#3345 = DIRECTION ( 'NONE',  ( 0.000000000000000000, 0.000000000000000000, 1.000000000000000000 ) ) ;
#3346 = CARTESIAN_POINT ( 'NONE',  ( 8.268597328390889345, 50.00000000054355098, -10.78867689284122733 ) ) ;
#3347 = CARTESIAN_POINT ( 'NONE',  ( 94.99999999999995737, 1.387778780781445676E-14, 5.125000002731184168 ) ) ;
#3348 = CARTESIAN_POINT ( 'NONE',  ( 124.3771271284221314, 36.98164062716787015, -13.57481594606304753 ) ) ;
#3349 = CARTESIAN_POINT ( 'NONE',  ( 99.99999999999998579, 90.25000000000000000, -4.999999999999997335 ) ) ;
#3350 = CARTESIAN_POINT ( 'NONE',  ( 13.57481594606304931, 31.92148437716787157, 5.622872871577868636 ) ) ;
#3351 = CARTESIAN_POINT ( 'NONE',  ( 208.1451861577817795, 37.22968750108393721, -5.444914386472297529 ) ) ;
#3352 = ORIENTED_EDGE ( 'NONE', *, *, #971, .F. ) ;
#3353 = CARTESIAN_POINT ( 'NONE',  ( 96.84719886470459471, 3.152801135295383084, 13.56250000136559386 ) ) ;
#3354 = CYLINDRICAL_SURFACE ( 'NONE', #28022, 0.5000000000000086597 ) ;
#3355 = CARTESIAN_POINT ( 'NONE',  ( 136.0859442160083859, 54.65299103241780898, 14.99999999999996092 ) ) ;
#3356 = DIRECTION ( 'NONE',  ( 0.000000000000000000, 1.000000000000000000, 0.000000000000000000 ) ) ;
#3357 = CARTESIAN_POINT ( 'NONE',  ( 65.00000000000000000, 31.82226562608393650, -13.14518615778179544 ) ) ;
#3358 = VECTOR ( 'NONE', #22604, 1000.000000000000000 ) ;
#3359 = CARTESIAN_POINT ( 'NONE',  ( 13.14518615778179900, 40.30546875108393579, 5.444914386472293977 ) ) ;
#3360 = CARTESIAN_POINT ( 'NONE',  ( -5.622872871577890841, 39.66054687716787441, 13.57481594606302444 ) ) ;
#3361 = DIRECTION ( 'NONE',  ( 0.000000000000000000, 0.000000000000000000, 1.000000000000000000 ) ) ;
#3362 = CARTESIAN_POINT ( 'NONE',  ( 143.5748159460630404, 34.30273437500000000, -5.622872871577873077 ) ) ;
#3363 = ORIENTED_EDGE ( 'NONE', *, *, #15545, .T. ) ;
#3364 = VERTEX_POINT ( 'NONE', #4315 ) ;
#3365 = CARTESIAN_POINT ( 'NONE',  ( 219.9999999999999716, 55.00000000000000000, 14.99999999999994316 ) ) ;
#3366 = CARTESIAN_POINT ( 'NONE',  ( -13.14518615778179544, 35.19570312608393436, 0.000000000000000000 ) ) ;
#3367 = CARTESIAN_POINT ( 'NONE',  ( -8.312177448680279460E-16, 34.55078125216787299, -13.57481594606304576 ) ) ;
#3368 = CARTESIAN_POINT ( 'NONE',  ( 102.0710678118654329, 5.000000000000018652, 3.812500002731184612 ) ) ;
#3369 = CARTESIAN_POINT ( 'NONE',  ( 143.1451861577818079, 39.61093750108393863, -5.444914386472297529 ) ) ;
#3370 = CARTESIAN_POINT ( 'NONE',  ( 51.85481384221819923, 40.50390625108394005, -5.444914386472297529 ) ) ;
#3371 = VERTEX_POINT ( 'NONE', #25829 ) ;
#3372 = CARTESIAN_POINT ( 'NONE',  ( 0.000000000000000000, 36.00000000000000000, 0.000000000000000000 ) ) ;
#3373 = CARTESIAN_POINT ( 'NONE',  ( -5.444914386472297529, 37.22968750108393721, -13.14518615778179900 ) ) ;
#3374 = CARTESIAN_POINT ( 'NONE',  ( 5.444914386472297529, 33.36015625108393579, -13.14518615778179722 ) ) ;
#3375 = CARTESIAN_POINT ( 'NONE',  ( 99.99999999999998579, 117.3602355696678643, -48.49999999999999289 ) ) ;
#3376 = CARTESIAN_POINT ( 'NONE',  ( 99.99999999999997158, 118.4984768113314146, -52.37499999726881583 ) ) ;
#3377 = ORIENTED_EDGE ( 'NONE', *, *, #20172, .T. ) ;
#3378 = CARTESIAN_POINT ( 'NONE',  ( 201.9444237971526661, 31.55306878032414986, -11.16113333171310451 ) ) ;
#3379 = DIRECTION ( 'NONE',  ( 0.000000000000000000, 0.000000000000000000, 1.000000000000000000 ) ) ;
#3380 = CARTESIAN_POINT ( 'NONE',  ( 101.7677669529663547, 123.0999999999999943, -1.767766952966370209 ) ) ;
#3381 = CARTESIAN_POINT ( 'NONE',  ( 99.99999999999998579, 124.5500000010924708, -2.066987299999998751 ) ) ;
#3382 = CARTESIAN_POINT ( 'NONE',  ( 125.5405265863609969, 36.00000000000002842, -12.68347323196757337 ) ) ;
#3383 = EDGE_CURVE ( 'NONE', #21141, #9074, #11023, .T. ) ;
#3384 = CARTESIAN_POINT ( 'NONE',  ( 130.0000000000000000, 40.10703125216787157, -13.57481594606304576 ) ) ;
#3385 = CARTESIAN_POINT ( 'NONE',  ( 103.1528011352953342, 3.152801135295383084, 14.06250000136559208 ) ) ;
#3386 = CARTESIAN_POINT ( 'NONE',  ( 9.598844408820459861, 33.36015624999999574, 9.598844408820456309 ) ) ;
#3387 = EDGE_LOOP ( 'NONE', ( #12731, #6830, #16012, #16694 ) ) ;
#3388 = CARTESIAN_POINT ( 'NONE',  ( -13.57481594606304398, 33.11210937499999574, 5.622872871577880183 ) ) ;
#3389 = CARTESIAN_POINT ( 'NONE',  ( 9.295050272127046043, 32.51679687608393721, -9.295050272127046043 ) ) ;
#3390 = CARTESIAN_POINT ( 'NONE',  ( 9.295050272127047819, 32.91367187608393152, 9.295050272127046043 ) ) ;
#3391 = CARTESIAN_POINT ( 'NONE',  ( 5.444914386472297529, 34.74921875108393721, -13.14518615778179722 ) ) ;
#3392 = CARTESIAN_POINT ( 'NONE',  ( -13.57481594606304576, 33.21132812716787441, 5.622872871577880183 ) ) ;
#3393 = CARTESIAN_POINT ( 'NONE',  ( 97.92893218813451028, 5.000000000000018652, 2.812499999999999112 ) ) ;
#3394 = CARTESIAN_POINT ( 'NONE',  ( 104.4587341249999781, 82.87500000136560629, 1.846868145590721655 ) ) ;
#3395 = CARTESIAN_POINT ( 'NONE',  ( 59.55508561352770158, 33.55859375108393294, 13.14518615778179722 ) ) ;
#3396 = CYLINDRICAL_SURFACE ( 'NONE', #21703, 5.000000000000004441 ) ;
#3397 = CARTESIAN_POINT ( 'NONE',  ( 5.622872871577825116, 35.29492187716787299, -13.57481594606309372 ) ) ;
#3398 =( BOUNDED_CURVE ( )  B_SPLINE_CURVE ( 2, ( #1880, #4286, #2010, #153, #19386, #27952, #10959, #12676, #15232 ),
 .UNSPECIFIED., .F., .F. ) 
 B_SPLINE_CURVE_WITH_KNOTS ( ( 3, 2, 2, 2, 3 ),
 ( 0.3500000000000003109, 0.3750000000000003331, 0.4000000000000003553, 0.4250000000000003775, 0.4500000000000003997 ),
 .UNSPECIFIED. ) 
 CURVE ( )  GEOMETRIC_REPRESENTATION_ITEM ( )  RATIONAL_B_SPLINE_CURVE ( ( 0.9999999999999990008, 0.9238795325112877377, 1.000000000000000000, 0.9238795325112867385, 1.000000000000000000, 0.9238795325112867385, 1.000000000000000000, 0.9238795325112855172, 1.000000000000001110 ) ) 
 REPRESENTATION_ITEM ( '' )  );
#3399 = EDGE_CURVE ( 'NONE', #8723, #14157, #38, .T. ) ;
#3400 = CARTESIAN_POINT ( 'NONE',  ( 100.8561741729129153, 123.5000000010924737, -2.066987299999999195 ) ) ;
#3401 = CARTESIAN_POINT ( 'NONE',  ( -9.598844408820454532, 32.36796874999999574, 9.598844408820459861 ) ) ;
#3402 = CARTESIAN_POINT ( 'NONE',  ( 102.4976396683250783, 102.3130555110000159, -53.27499999726882862 ) ) ;
#3403 = CARTESIAN_POINT ( 'NONE',  ( 130.0000000000000000, 33.80664062608393294, 13.14518615778179544 ) ) ;
#3404 = EDGE_LOOP ( 'NONE', ( #14988, #8739, #722, #24690 ) ) ;
#3405 = ADVANCED_FACE ( 'NONE', ( #898 ), #20265, .T. ) ;
#3406 = CARTESIAN_POINT ( 'NONE',  ( 204.5988444088204687, 36.63437500216787157, 9.598844408820456309 ) ) ;
#3407 = CARTESIAN_POINT ( 'NONE',  ( 98.15313185440925281, 81.62500000136560629, 4.458734124999987891 ) ) ;
#3408 = CARTESIAN_POINT ( 'NONE',  ( 116.8548138422182205, 39.75976562608393294, 0.000000000000000000 ) ) ;
#3409 = CARTESIAN_POINT ( 'NONE',  ( 74.59884440882045453, 39.21406250216787015, -9.598844408820458085 ) ) ;
#3410 = EDGE_CURVE ( 'NONE', #2056, #3788, #24873, .T. ) ;
#3411 = AXIS2_PLACEMENT_3D ( 'NONE', #10151, #18732, #5632 ) ;
#3412 = CARTESIAN_POINT ( 'NONE',  ( 106.5389055433250860, 114.7507929638356785, -46.42499999726882720 ) ) ;
#3413 = CARTESIAN_POINT ( 'NONE',  ( 200.4449143864723055, 39.41250000108393436, 13.14518615778179189 ) ) ;
#3414 = CARTESIAN_POINT ( 'NONE',  ( 5.622872871577878406, 38.96601562716787015, 13.57481594606304576 ) ) ;
#3415 = ORIENTED_EDGE ( 'NONE', *, *, #18830, .F. ) ;
#3416 = CARTESIAN_POINT ( 'NONE',  ( 104.9999999999999716, 1.449011120738813565E-14, 9.500000000000000000 ) ) ;
#3417 = ADVANCED_FACE ( 'NONE', ( #5165 ), #22698, .F. ) ;
#3418 = ORIENTED_EDGE ( 'NONE', *, *, #13399, .F. ) ;
#3419 = CARTESIAN_POINT ( 'NONE',  ( -13.14518615778179189, 33.65781250108393152, 5.444914386472304635 ) ) ;
#3420 = CARTESIAN_POINT ( 'NONE',  ( 195.0000000000000000, 40.35507812608393152, -13.14518615778179544 ) ) ;
#3421 = DIRECTION ( 'NONE',  ( 0.000000000000000000, 0.000000000000000000, 1.000000000000000000 ) ) ;
#3422 = CARTESIAN_POINT ( 'NONE',  ( 104.9999999999999574, -2.071067811865462627, 12.56250000273118772 ) ) ;
#3423 = CARTESIAN_POINT ( 'NONE',  ( 139.2950502721270425, 40.05742187608392868, 9.295050272127046043 ) ) ;
#3424 = CARTESIAN_POINT ( 'NONE',  ( -9.295050272127046043, 33.50898437608393010, -9.295050272127046043 ) ) ;
#3425 = CARTESIAN_POINT ( 'NONE',  ( 6.944423797152706079, 31.55306878032414986, -11.16113333171310451 ) ) ;
#3426 = CARTESIAN_POINT ( 'NONE',  ( 99.99999999999998579, 91.06249999863440792, 4.458734124999981674 ) ) ;
#3427 = CARTESIAN_POINT ( 'NONE',  ( 97.50000000000000000, 124.2500000000000000, 1.035533905932725096 ) ) ;
#3428 = CARTESIAN_POINT ( 'NONE',  ( 195.0000000000000000, 33.01289062608393721, 13.14518615778179544 ) ) ;
#3429 = EDGE_CURVE ( 'NONE', #5791, #10301, #673, .T. ) ;
#3430 = DIRECTION ( 'NONE',  ( 5.782411586589358625E-17, -0.000000000000000000, 1.000000000000000000 ) ) ;
#3431 = CARTESIAN_POINT ( 'NONE',  ( 99.99999999999995737, -4.458734124999988779, 7.937500001365592084 ) ) ;
#3432 = CARTESIAN_POINT ( 'NONE',  ( 93.00000000000000000, 112.2744378736303190, -52.60000000546237686 ) ) ;
#3433 = VECTOR ( 'NONE', #27349, 1000.000000000000000 ) ;
#3434 = CARTESIAN_POINT ( 'NONE',  ( 99.99999999999995737, -4.458734124999988779, 9.687500001365593860 ) ) ;
#3435 = CARTESIAN_POINT ( 'NONE',  ( 94.33688103937537051, 105.8855032339526758, -50.30000000546237970 ) ) ;
#3436 = CARTESIAN_POINT ( 'NONE',  ( 104.4587341249999923, 91.37499999863439371, -1.846868145590737198 ) ) ;
#3437 = DIRECTION ( 'NONE',  ( 0.000000000000000000, -0.000000000000000000, 1.000000000000000000 ) ) ;
#3438 = LINE ( 'NONE', #20408, #19355 ) ;
#3439 = CARTESIAN_POINT ( 'NONE',  ( -13.14518615778179544, 34.40195312608393152, 0.000000000000000000 ) ) ;
#3440 = EDGE_CURVE ( 'NONE', #5694, #9247, #27121, .T. ) ;
#3441 = EDGE_LOOP ( 'NONE', ( #21249, #25162, #12942, #26071 ) ) ;
#3442 = CARTESIAN_POINT ( 'NONE',  ( 95.54126587499996504, 82.68750000136560629, -1.387778780781445676E-14 ) ) ;
#3443 = EDGE_CURVE ( 'NONE', #7689, #10159, #21963, .T. ) ;
#3444 = B_SPLINE_CURVE_WITH_KNOTS ( 'NONE', 3,
 ( #16511, #21484, #14629, #8089, #25204, #3821 ),
 .UNSPECIFIED., .F., .F.,
 ( 4, 2, 4 ),
 ( 0.1250000000000000000, 0.1875000000000000000, 0.2500000000000000000 ),
 .UNSPECIFIED. ) ;
#3445 = CARTESIAN_POINT ( 'NONE',  ( 96.46446609406726225, 91.37500000000000000, -3.535533905932738197 ) ) ;
#3446 = EDGE_CURVE ( 'NONE', #1909, #24277, #8462, .T. ) ;
#3447 = CARTESIAN_POINT ( 'NONE',  ( 208.1451861577818079, 33.80664062608393294, -1.609821015232357215E-15 ) ) ;
#3448 = ORIENTED_EDGE ( 'NONE', *, *, #12134, .T. ) ;
#3449 = CARTESIAN_POINT ( 'NONE',  ( 186.6040612587084695, 54.99999999495823033, -15.00000000000000533 ) ) ;
#3450 = CARTESIAN_POINT ( 'NONE',  ( 95.54126587499995082, 1.846868145590750077, 7.625000001365592084 ) ) ;
#3451 = ORIENTED_EDGE ( 'NONE', *, *, #160, .F. ) ;
#3452 = CARTESIAN_POINT ( 'NONE',  ( 104.9952793366501851, 103.1245878333314323, -48.67500000273119554 ) ) ;
#3453 =( BOUNDED_CURVE ( )  B_SPLINE_CURVE ( 2, ( #22997, #20044, #18438, #3467, #2662, #27147, #24990, #13456, #12133 ),
 .UNSPECIFIED., .F., .F. ) 
 B_SPLINE_CURVE_WITH_KNOTS ( ( 3, 2, 2, 2, 3 ),
 ( 0.1458333333333336757, 0.1562500000000002776, 0.1666666666666669072, 0.1770833333333335369, 0.1875000000000001388 ),
 .UNSPECIFIED. ) 
 CURVE ( )  GEOMETRIC_REPRESENTATION_ITEM ( )  RATIONAL_B_SPLINE_CURVE ( ( 0.9999999999999975575, 0.9238795325112891810, 1.000000000000000000, 0.9238795325112867385, 1.000000000000000000, 0.9238795325112867385, 1.000000000000000000, 0.9238795325112857393, 1.000000000000001110 ) ) 
 REPRESENTATION_ITEM ( '' )  );
#3454 = CARTESIAN_POINT ( 'NONE',  ( 13.14518615778179900, 32.26875000108393721, -5.444914386472297529 ) ) ;
#3455 = CARTESIAN_POINT ( 'NONE',  ( 5.622872871578008080, 36.08867187716787583, -13.57481594606290898 ) ) ;
#3456 = CARTESIAN_POINT ( 'NONE',  ( 13.14518615778179722, 40.10703125108393152, 5.444914386472293977 ) ) ;
#3457 = CARTESIAN_POINT ( 'NONE',  ( -5.444914386472299306, 39.31328125108392868, 13.14518615778179722 ) ) ;
#3458 = CARTESIAN_POINT ( 'NONE',  ( -13.14518615778179189, 40.00781250108393294, 5.444914386472304635 ) ) ;
#3459 = CARTESIAN_POINT ( 'NONE',  ( 95.54126587499999346, 92.99999999863439371, -1.846868145590737864 ) ) ;
#3460 = VECTOR ( 'NONE', #2706, 1000.000000000000000 ) ;
#3461 = DIRECTION ( 'NONE',  ( 0.000000000000000000, 0.000000000000000000, 1.000000000000000000 ) ) ;
#3462 = CARTESIAN_POINT ( 'NONE',  ( -15.00000000000000355, 50.00000000000000000, -9.999999999999998224 ) ) ;
#3463 = CARTESIAN_POINT ( 'NONE',  ( -5.444914386472299306, 33.75703125108393721, 13.14518615778179722 ) ) ;
#3464 = CARTESIAN_POINT ( 'NONE',  ( 99.99999999999995737, 4.458734125000016313, 4.437500001365592084 ) ) ;
#3465 = CARTESIAN_POINT ( 'NONE',  ( 95.54126587499996504, 81.62500000136560629, -1.846868145590750077 ) ) ;
#3466 = CARTESIAN_POINT ( 'NONE',  ( -8.049105076161786076E-16, 35.59257812608393579, -13.14518615778179544 ) ) ;
#3467 = CARTESIAN_POINT ( 'NONE',  ( -13.57481594606304398, 38.76757812716787299, 5.622872871577880183 ) ) ;
#3468 = CARTESIAN_POINT ( 'NONE',  ( 68.03939705080254896, 53.88964894337313183, 14.99999999999997868 ) ) ;
#3469 = ORIENTED_EDGE ( 'NONE', *, *, #802, .F. ) ;
#3470 = CARTESIAN_POINT ( 'NONE',  ( 13.14518615778179544, 34.00507812608393721, -1.609821015232357215E-15 ) ) ;
#3471 = CARTESIAN_POINT ( 'NONE',  ( 102.4999999999999716, 123.0500000021849445, 1.035533905932722876 ) ) ;
#3472 = CARTESIAN_POINT ( 'NONE',  ( -20.00000000000000000, 50.00000000000000000, 10.00000000000000178 ) ) ;
#3473 = CARTESIAN_POINT ( 'NONE',  ( 104.9999999999999858, 90.87499999726880162, -6.938893903907228378E-15 ) ) ;
#3474 = CARTESIAN_POINT ( 'NONE',  ( 99.99999999999998579, 128.0000000000000000, -2.500000000000013767 ) ) ;
#3475 = EDGE_CURVE ( 'NONE', #24171, #14907, #20413, .T. ) ;
#3476 = LINE ( 'NONE', #8024, #3497 ) ;
#3477 = CARTESIAN_POINT ( 'NONE',  ( 100.0000000000000000, 110.0000000000000000, -55.00000000000000711 ) ) ;
#3478 = VECTOR ( 'NONE', #14868, 1000.000000000000000 ) ;
#3479 = ORIENTED_EDGE ( 'NONE', *, *, #1836, .F. ) ;
#3480 = CARTESIAN_POINT ( 'NONE',  ( 74.29505027212704249, 39.66054687608393436, -9.295050272127046043 ) ) ;
#3481 = EDGE_LOOP ( 'NONE', ( #8727, #14805 ) ) ;
#3482 = DIRECTION ( 'NONE',  ( 0.000000000000000000, -1.000000000000000000, -0.000000000000000000 ) ) ;
#3483 = CARTESIAN_POINT ( 'NONE',  ( 181.8548138422182205, 32.02070312608393010, 0.000000000000000000 ) ) ;
#3484 = EDGE_LOOP ( 'NONE', ( #27907, #10636, #20606, #21114 ) ) ;
#3485 = CARTESIAN_POINT ( 'NONE',  ( 95.00000000000000000, 92.43750000000000000, -2.071067811865479058 ) ) ;
#3486 = DIRECTION ( 'NONE',  ( 0.000000000000000000, 1.000000000000000000, 0.000000000000000000 ) ) ;
#3487 = CARTESIAN_POINT ( 'NONE',  ( 203.3922152916383936, 54.99999999999998579, 14.99999999999994316 ) ) ;
#3488 =( BOUNDED_CURVE ( )  B_SPLINE_CURVE ( 2, ( #19860, #9034, #17726, #10594, #8605, #4336, #7450, #921, #24420 ),
 .UNSPECIFIED., .F., .F. ) 
 B_SPLINE_CURVE_WITH_KNOTS ( ( 3, 2, 2, 2, 3 ),
 ( 0.3958333333333331483, 0.4062499999999999445, 0.4166666666666667407, 0.4270833333333335369, 0.4375000000000003331 ),
 .UNSPECIFIED. ) 
 CURVE ( )  GEOMETRIC_REPRESENTATION_ITEM ( )  RATIONAL_B_SPLINE_CURVE ( ( 1.000000000000001110, 0.9238795325112855172, 1.000000000000000000, 0.9238795325112867385, 1.000000000000000000, 0.9238795325112867385, 1.000000000000000000, 0.9238795325112842960, 1.000000000000002442 ) ) 
 REPRESENTATION_ITEM ( '' )  );
#3489 = CARTESIAN_POINT ( 'NONE',  ( 143.5748159460630688, 38.32109375216786873, -1.662435489736055892E-15 ) ) ;
#3490 = VECTOR ( 'NONE', #6838, 1000.000000000000000 ) ;
#3491 = CARTESIAN_POINT ( 'NONE',  ( 94.99999999999995737, -2.071067811865466624, 7.062499999999999112 ) ) ;
#3492 = DIRECTION ( 'NONE',  ( -0.5282856486898074300, 0.000000000000000000, 0.8490667072665075699 ) ) ;
#3493 = PRODUCT_DEFINITION_SHAPE ( 'NONE', 'NONE',  #28215 ) ;
#3494 = CARTESIAN_POINT ( 'NONE',  ( 208.1451861577817795, 37.92421875108392726, 5.444914386472293977 ) ) ;
#3495 = ORIENTED_EDGE ( 'NONE', *, *, #4985, .T. ) ;
#3496 = CARTESIAN_POINT ( 'NONE',  ( 104.4587341249999639, 1.442382525525748735E-14, 14.18750000136559208 ) ) ;
#3497 = VECTOR ( 'NONE', #1488, 1000.000000000000000 ) ;
#3498 = CARTESIAN_POINT ( 'NONE',  ( -1.816500417285228597, 36.00000000000000711, -13.35830014193482285 ) ) ;
#3499 = CARTESIAN_POINT ( 'NONE',  ( 13.57481594606304576, 39.80937499999999574, -1.662435489736055892E-15 ) ) ;
#3500 = CONICAL_SURFACE ( 'NONE', #13019, 23.26794919243113213, 0.5235987755983000369 ) ;
#3501 = CARTESIAN_POINT ( 'NONE',  ( 95.54126587499996504, 83.37500000136563472, -1.846868145590750077 ) ) ;
#3502 = LINE ( 'NONE', #12439, #8056 ) ;
#3503 = DIRECTION ( 'NONE',  ( 0.000000000000000000, 0.000000000000000000, 1.000000000000000000 ) ) ;
#3504 = CARTESIAN_POINT ( 'NONE',  ( 13.14518615778179544, 39.56132812608393579, -1.609821015232357215E-15 ) ) ;
#3505 = CARTESIAN_POINT ( 'NONE',  ( 5.622872871577976994, 40.75195312499999289, -13.57481594606294095 ) ) ;
#3506 = CARTESIAN_POINT ( 'NONE',  ( 104.9999999999999716, -2.071067811865462627, 6.437499999999999112 ) ) ;
#3507 = CARTESIAN_POINT ( 'NONE',  ( -13.14518615778179544, 40.75195312608393294, 0.000000000000000000 ) ) ;
#3508 = CARTESIAN_POINT ( 'NONE',  ( 135.6228728715778686, 32.81445312499999289, -13.57481594606304753 ) ) ;
#3509 = ORIENTED_EDGE ( 'NONE', *, *, #6847, .T. ) ;
#3510 = CARTESIAN_POINT ( 'NONE',  ( 70.62287287157784021, 36.48554687499999716, 13.57481594606309194 ) ) ;
#3511 = PRODUCT_DEFINITION_CONTEXT ( 'detailed design', #1690, 'design' ) ;
#3512 = CARTESIAN_POINT ( 'NONE',  ( 9.598844408820456309, 38.32109374999999574, -9.598844408820458085 ) ) ;
#3513 = CARTESIAN_POINT ( 'NONE',  ( 5.444914386472302859, 40.00781250108393294, 13.14518615778179189 ) ) ;
#3514 = APPLICATION_CONTEXT ( 'automotive_design' ) ;
#3515 = CIRCLE ( 'NONE', #23529, 25.00000000000001066 ) ;
#3516 = CARTESIAN_POINT ( 'NONE',  ( 104.9999999999999716, 1.449011120738813565E-14, 4.625000002731185944 ) ) ;
#3517 = CARTESIAN_POINT ( 'NONE',  ( 120.7049497278729575, 38.27148437608393294, -9.295050272127046043 ) ) ;
#3518 = CARTESIAN_POINT ( 'NONE',  ( 74.29505027212704249, 36.08867187608392868, 9.295050272127046043 ) ) ;
#3519 = ORIENTED_EDGE ( 'NONE', *, *, #18368, .F. ) ;
#3520 = ORIENTED_EDGE ( 'NONE', *, *, #27613, .T. ) ;
#3521 = DIRECTION ( 'NONE',  ( 0.000000000000000000, 0.000000000000000000, -1.000000000000000000 ) ) ;
#3522 = CARTESIAN_POINT ( 'NONE',  ( 9.295050272127047819, 39.26367187608393294, 9.295050272127046043 ) ) ;
#3523 = CARTESIAN_POINT ( 'NONE',  ( 101.0355339059327378, 124.0500000021849445, -2.499999999999997780 ) ) ;
#3524 = CARTESIAN_POINT ( 'NONE',  ( 186.8746960822089136, 36.00000000000000711, 10.34220695173589810 ) ) ;
#3525 = PRODUCT_RELATED_PRODUCT_CATEGORY ( 'part', '', ( #11714 ) ) ;
#3526 = CARTESIAN_POINT ( 'NONE',  ( 108.0825317499999869, 107.3738262389971680, -52.97499999726881725 ) ) ;
#3527 = ADVANCED_FACE ( 'NONE', ( #5308 ), #17491, .T. ) ;
#3528 = CARTESIAN_POINT ( 'NONE',  ( 208.5748159460630688, 40.65273437499999432, -5.622872871577873966 ) ) ;
#3529 = CARTESIAN_POINT ( 'NONE',  ( 195.0000000000000000, 32.41757812608393863, -13.14518615778179544 ) ) ;
#3530 = DIRECTION ( 'NONE',  ( 0.000000000000000000, 0.000000000000000000, -1.000000000000000000 ) ) ;
#3531 = CARTESIAN_POINT ( 'NONE',  ( 101.7677669529663547, 123.1069999999781572, -1.767766952966370209 ) ) ;
#3532 = CARTESIAN_POINT ( 'NONE',  ( 100.8561741729129153, 122.7000000010924623, -2.066987299999999195 ) ) ;
#3533 = CARTESIAN_POINT ( 'NONE',  ( 117.4334932752013145, 36.00000000000000000, -4.295155080288600047 ) ) ;
#3534 =( BOUNDED_CURVE ( )  B_SPLINE_CURVE ( 2, ( #9992, #3455, #23262, #14127, #22706 ),
 .UNSPECIFIED., .F., .F. ) 
 B_SPLINE_CURVE_WITH_KNOTS ( ( 3, 2, 3 ),
 ( 0.4375000000000003331, 0.4479166666666667962, 0.4520580917964582834 ),
 .UNSPECIFIED. ) 
 CURVE ( )  GEOMETRIC_REPRESENTATION_ITEM ( )  RATIONAL_B_SPLINE_CURVE ( ( 0.9999999999999975575, 0.9238795325112891810, 1.000000000000000000, 0.9697362671728727568, 0.9635368512068458458 ) ) 
 REPRESENTATION_ITEM ( '' )  );
#3535 = DIRECTION ( 'NONE',  ( 0.000000000000000000, 0.000000000000000000, 1.000000000000000000 ) ) ;
#3536 = CARTESIAN_POINT ( 'NONE',  ( 104.4587341249999639, 1.442382525525748735E-14, 13.93750000136559208 ) ) ;
#3537 = CARTESIAN_POINT ( 'NONE',  ( 104.9999999999999716, 1.449011120738813565E-14, 13.62500000273118417 ) ) ;
#3538 = ORIENTED_EDGE ( 'NONE', *, *, #9856, .T. ) ;
#3539 = CARTESIAN_POINT ( 'NONE',  ( -11.69037824551319460, 35.99999999999998579, -6.307928093363390332 ) ) ;
#3540 = CARTESIAN_POINT ( 'NONE',  ( -8.049105076161786076E-16, 31.82226562608393650, -13.14518615778179544 ) ) ;
#3541 = CARTESIAN_POINT ( 'NONE',  ( 13.14518615778179722, 32.26875000108393721, -5.444914386472297529 ) ) ;
#3542 = CARTESIAN_POINT ( 'NONE',  ( -9.598844408820454532, 31.67343750216787512, 9.598844408820459861 ) ) ;
#3543 = CARTESIAN_POINT ( 'NONE',  ( 84.99999999999998579, 100.0000000000000000, -13.00000000000000533 ) ) ;
#3544 = CARTESIAN_POINT ( 'NONE',  ( 99.99999999999995737, 79.68750000136559208, 4.458734124999988779 ) ) ;
#3545 = CARTESIAN_POINT ( 'NONE',  ( 78.14518615778179367, 33.75703125108393010, 5.444914386472293977 ) ) ;
#3546 = CARTESIAN_POINT ( 'NONE',  ( 106.5389055433251002, 105.2492070361643215, -50.57500000273120122 ) ) ;
#3547 = FACE_OUTER_BOUND ( 'NONE', #8301, .T. ) ;
#3548 = CARTESIAN_POINT ( 'NONE',  ( 101.4615807364564546, 123.6500000010924651, -1.461580736456474794 ) ) ;
#3549 = DIRECTION ( 'NONE',  ( -1.000000000000000000, 0.000000000000000000, -0.000000000000000000 ) ) ;
#3550 = CARTESIAN_POINT ( 'NONE',  ( 107.0000000000000000, 107.7255621263696668, -47.59999999453764019 ) ) ;
#3551 = CARTESIAN_POINT ( 'NONE',  ( 143.1451861577818079, 35.54296875108394715, 5.444914386472293977 ) ) ;
#3552 = ORIENTED_EDGE ( 'NONE', *, *, #25847, .T. ) ;
#3553 = CARTESIAN_POINT ( 'NONE',  ( 1.605271876576585877, 53.60388944777323417, -15.00000000000000355 ) ) ;
#3554 = FACE_OUTER_BOUND ( 'NONE', #2631, .T. ) ;
#3555 = CARTESIAN_POINT ( 'NONE',  ( -13.57481594606304753, 39.46210937716787726, -5.622872871577873077 ) ) ;
#3556 = CARTESIAN_POINT ( 'NONE',  ( 130.0000000000000000, 39.16445312608392726, 13.14518615778179544 ) ) ;
#3557 = CARTESIAN_POINT ( 'NONE',  ( 65.00000000000000000, 40.10703125216787157, -13.57481594606304576 ) ) ;
#3558 = CARTESIAN_POINT ( 'NONE',  ( 97.50236033167490746, 102.3130555110000159, -55.22499999726881725 ) ) ;
#3559 = CARTESIAN_POINT ( 'NONE',  ( 5.622872871577871301, 39.26367187716787299, -13.57481594606304753 ) ) ;
#3560 = VERTEX_POINT ( 'NONE', #27260 ) ;
#3561 = CARTESIAN_POINT ( 'NONE',  ( 102.0710678118654329, -4.999999999999989342, 8.312500000000000000 ) ) ;
#3562 = EDGE_LOOP ( 'NONE', ( #1507, #10424, #14446, #1359, #25329 ) ) ;
#3563 = CARTESIAN_POINT ( 'NONE',  ( -13.14518615778179900, 31.97109375108393436, -5.444914386472297529 ) ) ;
#3564 = CARTESIAN_POINT ( 'NONE',  ( 204.5988444088204687, 31.87187500216787228, 9.598844408820456309 ) ) ;
#3565 = EDGE_CURVE ( 'NONE', #26666, #18529, #22067, .T. ) ;
#3566 = CARTESIAN_POINT ( 'NONE',  ( -8.312177448680279460E-16, 31.37578125216787583, -13.57481594606304576 ) ) ;
#3567 = CARTESIAN_POINT ( 'NONE',  ( 94.99999999999995737, 2.071067811865491048, 13.06250000273118772 ) ) ;
#3568 = CARTESIAN_POINT ( 'NONE',  ( 143.1451861577818079, 38.56914062608393579, -1.609821015232357215E-15 ) ) ;
#3569 = CARTESIAN_POINT ( 'NONE',  ( 5.444914386472297529, 32.56640625108394005, -13.14518615778179900 ) ) ;
#3570 = EDGE_CURVE ( 'NONE', #15231, #896, #20412, .T. ) ;
#3571 = CARTESIAN_POINT ( 'NONE',  ( 104.9999999999999716, 1.449011120738813565E-14, 11.50000000000000000 ) ) ;
#3572 = CARTESIAN_POINT ( 'NONE',  ( 104.4587341249999923, 93.37499999863440792, -1.846868145590737198 ) ) ;
#3573 =( BOUNDED_CURVE ( )  B_SPLINE_CURVE ( 2, ( #15155, #8905, #17593 ),
 .UNSPECIFIED., .F., .T. ) 
 B_SPLINE_CURVE_WITH_KNOTS ( ( 3, 3 ),
 ( 0.8250000005912483392, 0.8500000000000007550 ),
 .UNSPECIFIED. ) 
 CURVE ( )  GEOMETRIC_REPRESENTATION_ITEM ( )  RATIONAL_B_SPLINE_CURVE ( ( 1.000000000000000000, 0.9238795325112844070, 1.000000000000002442 ) ) 
 REPRESENTATION_ITEM ( '' )  );
#3574 = CARTESIAN_POINT ( 'NONE',  ( 97.50000000000000000, 123.3999999999999915, -9.540979117872439019E-15 ) ) ;
#3575 = CARTESIAN_POINT ( 'NONE',  ( 208.5748159460630120, 37.37851562499999858, 5.622872871577869525 ) ) ;
#3576 = ITEM_DEFINED_TRANSFORMATION ( 'NONE', 'NONE', #6294,  #26844 ) ;
#3577 = CARTESIAN_POINT ( 'NONE',  ( 99.99999999999995737, 4.458734125000016313, 3.437500001365592972 ) ) ;
#3578 = DIRECTION ( 'NONE',  ( 0.000000000000000000, 0.000000000000000000, -1.000000000000000000 ) ) ;
#3579 = CARTESIAN_POINT ( 'NONE',  ( 103.1528011352953342, -3.152801135295355106, 5.812500001365591196 ) ) ;
#3580 = CARTESIAN_POINT ( 'NONE',  ( 93.00000000000001421, 107.7255621263696668, -46.40000000546238113 ) ) ;
#3581 = CARTESIAN_POINT ( 'NONE',  ( 104.4587341249999781, 95.56249999863440792, -6.938893903907228378E-15 ) ) ;
#3582 = FACE_OUTER_BOUND ( 'NONE', #18019, .T. ) ;
#3583 = CARTESIAN_POINT ( 'NONE',  ( -13.09590655363597733, 36.00000000000000000, 1.137167824541468031 ) ) ;
#3584 = CARTESIAN_POINT ( 'NONE',  ( 5.622872871577878406, 38.86679687499999858, 13.57481594606304576 ) ) ;
#3585 = AXIS2_PLACEMENT_3D ( 'NONE', #2384, #11042, #25894 ) ;
#3586 = EDGE_CURVE ( 'NONE', #7991, #9045, #19962, .T. ) ;
#3587 = ORIENTED_EDGE ( 'NONE', *, *, #2192, .F. ) ;
#3588 = CARTESIAN_POINT ( 'NONE',  ( 104.4587341249999781, 83.12500000136560629, 1.846868145590721655 ) ) ;
#3589 = AXIS2_PLACEMENT_3D ( 'NONE', #18258, #11964, #24674 ) ;
#3590 = FACE_OUTER_BOUND ( 'NONE', #3656, .T. ) ;
#3591 = ORIENTED_EDGE ( 'NONE', *, *, #7284, .T. ) ;
#3592 = ORIENTED_EDGE ( 'NONE', *, *, #1010, .F. ) ;
#3593 = CARTESIAN_POINT ( 'NONE',  ( 194.6030005853479850, 51.45716825712459297, -15.00000000000067324 ) ) ;
#3594 = CARTESIAN_POINT ( 'NONE',  ( 99.99999999999995737, 4.458734125000016313, 7.437500001365592084 ) ) ;
#3595 = EDGE_CURVE ( 'NONE', #10432, #10042, #3306, .T. ) ;
#3596 = VERTEX_POINT ( 'NONE', #22840 ) ;
#3597 = CARTESIAN_POINT ( 'NONE',  ( 95.00472066334982912, 103.1245878333314323, -45.07500000273119412 ) ) ;
#3598 = CARTESIAN_POINT ( 'NONE',  ( -13.14518615778179544, 34.99726562608393721, 0.000000000000000000 ) ) ;
#3599 = CARTESIAN_POINT ( 'NONE',  ( 204.5988444088204687, 39.80937500216786873, 9.598844408820456309 ) ) ;
#3600 = CARTESIAN_POINT ( 'NONE',  ( 9.295050272127046043, 39.46210937608393010, -9.295050272127046043 ) ) ;
#3601 = CARTESIAN_POINT ( 'NONE',  ( 93.46109445667491400, 105.2492070361643215, -44.92500000273119554 ) ) ;
#3602 = VECTOR ( 'NONE', #28060, 1000.000000000000000 ) ;
#3603 = CARTESIAN_POINT ( 'NONE',  ( 130.0000000000000000, 39.36289062608393152, 13.14518615778179544 ) ) ;
#3604 = CARTESIAN_POINT ( 'NONE',  ( -13.14518615778179900, 31.77265625108393365, -5.444914386472297529 ) ) ;
#3605 = CARTESIAN_POINT ( 'NONE',  ( 59.37712712842213136, 37.67617187499999432, -13.57481594606304753 ) ) ;
#3606 = CARTESIAN_POINT ( 'NONE',  ( 65.00000000000000000, -7.395377635281828788, 13.57481594606303688 ) ) ;
#3607 = EDGE_CURVE ( 'NONE', #1074, #11913, #13690, .T. ) ;
#3608 = CARTESIAN_POINT ( 'NONE',  ( -13.57481594606304576, 37.13046875216787868, 0.000000000000000000 ) ) ;
#3609 = CARTESIAN_POINT ( 'NONE',  ( 5.444914386472297529, 34.15390625108393863, -13.14518615778179900 ) ) ;
#3610 = CARTESIAN_POINT ( 'NONE',  ( 103.1528011352953342, 3.152801135295383084, 3.312500001365592972 ) ) ;
#3611 = CARTESIAN_POINT ( 'NONE',  ( 99.99999999999995737, 81.93750000136559208, 4.458734124999988779 ) ) ;
#3612 = CARTESIAN_POINT ( 'NONE',  ( -8.049105076161786076E-16, 34.79882812608393294, -13.14518615778179544 ) ) ;
#3613 = CARTESIAN_POINT ( 'NONE',  ( 70.62287287157774074, 38.96601562716787015, 13.57481594606318076 ) ) ;
#3614 = CARTESIAN_POINT ( 'NONE',  ( 71.07908002051881624, 54.65154858643460756, 14.99999999999997513 ) ) ;
#3615 = VERTEX_POINT ( 'NONE', #14259 ) ;
#3616 = CARTESIAN_POINT ( 'NONE',  ( 5.444914386472302859, 33.06250000108393294, 13.14518615778179189 ) ) ;
#3617 = CARTESIAN_POINT ( 'NONE',  ( 98.53841926354351699, 123.8500000010924680, 1.461580736456455920 ) ) ;
#3618 = CARTESIAN_POINT ( 'NONE',  ( 95.54126587499999346, 92.99999999863439371, -1.846868145590737864 ) ) ;
#3619 = CARTESIAN_POINT ( 'NONE',  ( -8.312177448680279460E-16, 32.16953125216787157, -13.57481594606304576 ) ) ;
#3620 = DIRECTION ( 'NONE',  ( 0.000000000000000000, 0.000000000000000000, 1.000000000000000000 ) ) ;
#3621 = LINE ( 'NONE', #1765, #27610 ) ;
#3622 = CARTESIAN_POINT ( 'NONE',  ( 3.755638265659908104, 31.58960998161716560, -13.14518615778179900 ) ) ;
#3623 = PRESENTATION_LAYER_ASSIGNMENT (  '', '', ( #2261 ) ) ;
#3624 = ORIENTED_EDGE ( 'NONE', *, *, #10051, .F. ) ;
#3625 = CARTESIAN_POINT ( 'NONE',  ( 55.70494972787295751, 39.26367187608393294, 9.295050272127047819 ) ) ;
#3626 = PLANE ( 'NONE',  #23713 ) ;
#3627 = CARTESIAN_POINT ( 'NONE',  ( -5.622872871578011633, 39.56132812500000284, 13.57481594606290720 ) ) ;
#3628 = ORIENTED_EDGE ( 'NONE', *, *, #11512, .F. ) ;
#3629 = CARTESIAN_POINT ( 'NONE',  ( 99.99999999999998579, 92.25000000000000000, -4.999999999999997335 ) ) ;
#3630 = LINE ( 'NONE', #12293, #23172 ) ;
#3631 = DIRECTION ( 'NONE',  ( -0.000000000000000000, 1.000000000000000000, -0.000000000000000000 ) ) ;
#3632 = CARTESIAN_POINT ( 'NONE',  ( 135.6228728715778971, 34.20351562716788862, 13.57481594606304576 ) ) ;
#3633 = CARTESIAN_POINT ( 'NONE',  ( 55.40115559117954547, 40.20625000216787726, -9.598844408820458085 ) ) ;
#3634 = CARTESIAN_POINT ( 'NONE',  ( 107.0000000000000000, 110.0000000000000000, -47.49999999453763877 ) ) ;
#3635 = ADVANCED_FACE ( 'NONE', ( #9422 ), #27120, .F. ) ;
#3636 = CARTESIAN_POINT ( 'NONE',  ( 181.8548138422182205, 38.37070312608393152, 0.000000000000000000 ) ) ;
#3637 = EDGE_LOOP ( 'NONE', ( #10292, #16089 ) ) ;
#3638 = VERTEX_POINT ( 'NONE', #2876 ) ;
#3639 = SURFACE_STYLE_FILL_AREA ( #23163 ) ;
#3640 = LINE ( 'NONE', #21302, #24379 ) ;
#3641 = CARTESIAN_POINT ( 'NONE',  ( 2.493653234604083739E-15, 33.26093749999999716, 13.57481594606304576 ) ) ;
#3642 = CARTESIAN_POINT ( 'NONE',  ( 103.1528011352953342, 83.06250000136560629, -3.152801135295383084 ) ) ;
#3643 = CARTESIAN_POINT ( 'NONE',  ( 65.00000000000000000, 40.10703125216787157, -13.57481594606304576 ) ) ;
#3644 = CARTESIAN_POINT ( 'NONE',  ( -8.049105076161786076E-16, 40.55351562608393579, -13.14518615778179544 ) ) ;
#3645 = CARTESIAN_POINT ( 'NONE',  ( -13.14518615778179544, 39.16445312608393436, 0.000000000000000000 ) ) ;
#3646 = CARTESIAN_POINT ( 'NONE',  ( -13.57481594606304753, 39.46210937716787726, -5.622872871577872189 ) ) ;
#3647 = LINE ( 'NONE', #25859, #24405 ) ;
#3648 = CARTESIAN_POINT ( 'NONE',  ( 99.99999999999995737, 83.25000000000000000, 4.999999999999990230 ) ) ;
#3649 = CARTESIAN_POINT ( 'NONE',  ( 102.4976396683250783, 117.6869444889999841, -46.22499999726882436 ) ) ;
#3650 = ORIENTED_EDGE ( 'NONE', *, *, #11058, .T. ) ;
#3651 = AXIS2_PLACEMENT_3D ( 'NONE', #1444, #7844, #18682 ) ;
#3652 = ORIENTED_EDGE ( 'NONE', *, *, #24310, .F. ) ;
#3653 = CARTESIAN_POINT ( 'NONE',  ( 102.0710678118654329, 84.31250000000000000, 4.999999999999999112 ) ) ;
#3654 = CARTESIAN_POINT ( 'NONE',  ( -13.57481594606304576, 39.46210937499999005, 5.622872871577880183 ) ) ;
#3655 = CARTESIAN_POINT ( 'NONE',  ( 9.295050272127046043, 39.46210937608393010, -9.295050272127046043 ) ) ;
#3656 = EDGE_LOOP ( 'NONE', ( #3628, #19484, #11881, #4808 ) ) ;
#3657 =( BOUNDED_CURVE ( )  B_SPLINE_CURVE ( 2, ( #13324, #22189, #21916, #389, #4380, #21772, #10771, #17905, #9071, #26176, #530 ),
 .UNSPECIFIED., .F., .F. ) 
 B_SPLINE_CURVE_WITH_KNOTS ( ( 3, 2, 2, 2, 2, 3 ),
 ( 0.8000000000000000444, 0.8199999999999999512, 0.8399999999999999689, 0.8599999999999999867, 0.8800000000000000044, 0.9000000000000000222 ),
 .UNSPECIFIED. ) 
 CURVE ( )  GEOMETRIC_REPRESENTATION_ITEM ( )  RATIONAL_B_SPLINE_CURVE ( ( 1.000000000000000000, 0.9510565162951535312, 1.000000000000000000, 0.9510565162951535312, 1.000000000000000000, 0.9510565162951535312, 1.000000000000000000, 0.9510565162951535312, 1.000000000000000000, 0.9510565162951535312, 1.000000000000000000 ) ) 
 REPRESENTATION_ITEM ( '' )  );
#3658 = CARTESIAN_POINT ( 'NONE',  ( 94.99999999999995737, 1.387778780781445676E-14, 7.125000002731185056 ) ) ;
#3659 = CARTESIAN_POINT ( 'NONE',  ( 116.8548138422182063, 39.21406250108392300, 5.444914386472304635 ) ) ;
#3660 = CARTESIAN_POINT ( 'NONE',  ( 55.70494972787295751, 38.07304687608393579, -9.295050272127046043 ) ) ;
#3661 = ORIENTED_EDGE ( 'NONE', *, *, #2880, .F. ) ;
#3662 = CARTESIAN_POINT ( 'NONE',  ( 99.99999999999998579, 123.0000000000000000, -5.204170427930421283E-15 ) ) ;
#3663 = CARTESIAN_POINT ( 'NONE',  ( 5.444914386472297529, 37.13046875108393152, -13.14518615778179900 ) ) ;
#3664 = CARTESIAN_POINT ( 'NONE',  ( 51.42518405393695957, 36.28710937499999289, 5.622872871577880183 ) ) ;
#3665 = CARTESIAN_POINT ( 'NONE',  ( 98.23223304703363112, 123.6000000021849416, 1.767766952966351557 ) ) ;
#3666 = CARTESIAN_POINT ( 'NONE',  ( 195.0000000000000000, 36.53515625216787299, 13.57481594606304576 ) ) ;
#3667 = CARTESIAN_POINT ( 'NONE',  ( 99.99999999999995737, 81.75000000000000000, -5.000000000000018652 ) ) ;
#3668 = AXIS2_PLACEMENT_3D ( 'NONE', #15004, #23582, #19305 ) ;
#3669 = VERTEX_POINT ( 'NONE', #22979 ) ;
#3670 = DIRECTION ( 'NONE',  ( -0.000000000000000000, 0.000000000000000000, -1.000000000000000000 ) ) ;
#3671 = CARTESIAN_POINT ( 'NONE',  ( 2.414731522848535132E-15, 37.57695312608392868, 13.14518615778179544 ) ) ;
#3672 = CARTESIAN_POINT ( 'NONE',  ( 131.6855116490828834, 35.99999999999997868, 13.05727741351676130 ) ) ;
#3673 = CARTESIAN_POINT ( 'NONE',  ( 97.50000000000000000, 124.9500000000000028, -1.035533905932742416 ) ) ;
#3674 = CARTESIAN_POINT ( 'NONE',  ( 97.93301270000000613, 122.9500000010924765, -9.540979117872439019E-15 ) ) ;
#3675 = CARTESIAN_POINT ( 'NONE',  ( 116.8473230904128002, 35.99999999999999289, 0.5874252385153416745 ) ) ;
#3676 = CARTESIAN_POINT ( 'NONE',  ( 104.4587341249999781, -1.846868145590721655, 11.87500000136559031 ) ) ;
#3677 = ORIENTED_EDGE ( 'NONE', *, *, #27980, .T. ) ;
#3678 = CARTESIAN_POINT ( 'NONE',  ( 94.33688103937535629, 105.8855032339526758, -50.29999999453763593 ) ) ;
#3679 = CARTESIAN_POINT ( 'NONE',  ( -9.598844408820454532, 39.51171874999999289, 9.598844408820459861 ) ) ;
#3680 = CARTESIAN_POINT ( 'NONE',  ( 96.46446609406721961, 3.535533905932755072, 8.875000000000000000 ) ) ;
#3681 = CARTESIAN_POINT ( 'NONE',  ( 5.622872871577878406, 32.61601562716786873, 13.57481594606304576 ) ) ;
#3682 = CARTESIAN_POINT ( 'NONE',  ( 94.99999999999995737, 1.387778780781445676E-14, 2.999999999999999112 ) ) ;
#3683 = CARTESIAN_POINT ( 'NONE',  ( 99.99999999999995737, 84.43750000136560629, -4.458734125000016313 ) ) ;
#3684 = CARTESIAN_POINT ( 'NONE',  ( 65.00000000000000000, 37.37851562608393863, -13.14518615778179544 ) ) ;
#3685 = CARTESIAN_POINT ( 'NONE',  ( 91.91746824999999887, 110.0000000000000000, -47.37500000273119838 ) ) ;
#3686 = CARTESIAN_POINT ( 'NONE',  ( 95.67376207875072680, 104.0454443415356991, -46.70000000000000284 ) ) ;
#3687 = CARTESIAN_POINT ( 'NONE',  ( 98.53841926354351699, 123.2500000010924737, 1.461580736456455920 ) ) ;
#3688 = DIRECTION ( 'NONE',  ( 5.782411586589358625E-17, -0.000000000000000000, 1.000000000000000000 ) ) ;
#3689 = CARTESIAN_POINT ( 'NONE',  ( 94.33688103937534208, 114.1144967660473242, -52.69999999453764161 ) ) ;
#3690 = CARTESIAN_POINT ( 'NONE',  ( 143.5748159460630404, 39.75976562499999289, 5.622872871577869525 ) ) ;
#3691 = ORIENTED_EDGE ( 'NONE', *, *, #8997, .F. ) ;
#3692 = CARTESIAN_POINT ( 'NONE',  ( 102.0710678118654329, 5.000000000000018652, 7.687499999999999112 ) ) ;
#3693 = EDGE_CURVE ( 'NONE', #4535, #20388, #22882, .T. ) ;
#3694 = CARTESIAN_POINT ( 'NONE',  ( -13.14518615778179544, 39.95820312608393010, 0.000000000000000000 ) ) ;
#3695 = CARTESIAN_POINT ( 'NONE',  ( 95.54126587499996504, 81.43750000136559208, -1.387778780781445676E-14 ) ) ;
#3696 = CARTESIAN_POINT ( 'NONE',  ( 120.7049497278729575, 39.06523437608392868, 9.295050272127047819 ) ) ;
#3697 = CARTESIAN_POINT ( 'NONE',  ( 51.42518405393695957, 37.18007812716787441, 5.622872871577880183 ) ) ;
#3698 = AXIS2_PLACEMENT_3D ( 'NONE', #7625, #16317, #4471 ) ;
#3699 = CARTESIAN_POINT ( 'NONE',  ( 108.0825317499999869, 107.3738262389971538, -54.72499999726881015 ) ) ;
#3700 = CARTESIAN_POINT ( 'NONE',  ( 9.598844408820456309, 35.24531250216787726, -9.598844408820458085 ) ) ;
#3701 = VERTEX_POINT ( 'NONE', #24965 ) ;
#3702 = CARTESIAN_POINT ( 'NONE',  ( 94.99999999999995737, -2.071067811865466624, 11.06250000000000000 ) ) ;
#3703 = CARTESIAN_POINT ( 'NONE',  ( 99.99999999999998579, 117.3602355696678643, -52.50000000000000000 ) ) ;
#3704 =( BOUNDED_CURVE ( )  B_SPLINE_CURVE ( 2, ( #19039, #23469, #14888, #21901, #10756, #22033, #10896, #15456, #23746 ),
 .UNSPECIFIED., .F., .F. ) 
 B_SPLINE_CURVE_WITH_KNOTS ( ( 3, 2, 2, 2, 3 ),
 ( 0.3214285714285713969, 0.3303571428571427937, 0.3392857142857143016, 0.3482142857142856984, 0.3571428571428572063 ),
 .UNSPECIFIED. ) 
 CURVE ( )  GEOMETRIC_REPRESENTATION_ITEM ( )  RATIONAL_B_SPLINE_CURVE ( ( 1.000000000000000444, 0.9238795325112862944, 1.000000000000000000, 0.9238795325112867385, 1.000000000000000000, 0.9238795325112867385, 1.000000000000000000, 0.9238795325112862944, 1.000000000000000444 ) ) 
 REPRESENTATION_ITEM ( '' )  );
#3705 = CARTESIAN_POINT ( 'NONE',  ( -8.049105076161786076E-16, 32.61601562608393579, -13.14518615778179544 ) ) ;
#3706 = CARTESIAN_POINT ( 'NONE',  ( 208.1451861577817795, 37.03125000108393294, -5.444914386472297529 ) ) ;
#3707 = DIRECTION ( 'NONE',  ( 5.782411586589358625E-17, -0.000000000000000000, 1.000000000000000000 ) ) ;
#3708 = CARTESIAN_POINT ( 'NONE',  ( 130.0000000000000000, 37.97382812608393721, -13.14518615778179544 ) ) ;
#3709 = CARTESIAN_POINT ( 'NONE',  ( -13.14518615778179544, 32.81445312608393294, 0.000000000000000000 ) ) ;
#3710 = DIRECTION ( 'NONE',  ( 1.000000000000000000, 0.000000000000000000, -0.000000000000000000 ) ) ;
#3711 = CARTESIAN_POINT ( 'NONE',  ( 95.54126587499999346, 93.87499999863439371, 1.846868145590722543 ) ) ;
#3712 = CARTESIAN_POINT ( 'NONE',  ( 106.5389055433251002, 105.2492070361643215, -52.57500000273119412 ) ) ;
#3713 = CARTESIAN_POINT ( 'NONE',  ( 99.99999999999998579, 122.9500000010924765, -2.066987299999998751 ) ) ;
#3714 = CARTESIAN_POINT ( 'NONE',  ( 204.5988444088204403, 36.73359374999999716, -9.598844408820458085 ) ) ;
#3715 = APPLICATION_PROTOCOL_DEFINITION ( 'draft international standard', 'automotive_design', 1998, #12763 ) ;
#3716 = CARTESIAN_POINT ( 'NONE',  ( 125.6259778691823641, 36.00000000000001421, 12.40367315690590466 ) ) ;
#3717 = CARTESIAN_POINT ( 'NONE',  ( 104.4587341249999781, 1.846868145590750299, 1.250000001365592750 ) ) ;
#3718 = CARTESIAN_POINT ( 'NONE',  ( 65.00000000000000000, 39.95820312608393010, 13.14518615778179544 ) ) ;
#3719 = CARTESIAN_POINT ( 'NONE',  ( 99.99999999999995737, -4.458734124999988779, 4.687500001365592084 ) ) ;
#3720 = CARTESIAN_POINT ( 'NONE',  ( 94.33688103937537051, 114.1144967660473242, -48.70000000546237828 ) ) ;
#3721 = CARTESIAN_POINT ( 'NONE',  ( 95.54126587499999346, 92.99999999863439371, -1.846868145590737864 ) ) ;
#3722 = CARTESIAN_POINT ( 'NONE',  ( 13.57481594606304931, 39.75976562499999289, 5.622872871577868636 ) ) ;
#3723 = CARTESIAN_POINT ( 'NONE',  ( 99.99999999999995737, 1.387778780781445676E-14, 34.79898987322334136 ) ) ;
#3724 = CARTESIAN_POINT ( 'NONE',  ( -8.312177448680279460E-16, 39.21406249999999716, -13.57481594606304576 ) ) ;
#3725 = ORIENTED_EDGE ( 'NONE', *, *, #2373, .T. ) ;
#3726 = CARTESIAN_POINT ( 'NONE',  ( 104.4587341249999781, 81.12500000136559208, 1.846868145590721655 ) ) ;
#3727 = CARTESIAN_POINT ( 'NONE',  ( 101.8468681455907330, 91.49999999863440792, -4.458734124999994997 ) ) ;
#3728 = ORIENTED_EDGE ( 'NONE', *, *, #3075, .T. ) ;
#3729 = EDGE_CURVE ( 'NONE', #23665, #499, #24540, .T. ) ;
#3730 = ORIENTED_EDGE ( 'NONE', *, *, #288, .F. ) ;
#3731 = CARTESIAN_POINT ( 'NONE',  ( 99.99999999999998579, 90.00000000000000000, -6.938893903907228378E-15 ) ) ;
#3732 = CARTESIAN_POINT ( 'NONE',  ( 99.99999999999995737, -4.458734124999988779, 4.937500001365592972 ) ) ;
#3733 = ORIENTED_EDGE ( 'NONE', *, *, #2971, .F. ) ;
#3734 = CARTESIAN_POINT ( 'NONE',  ( 106.5389055433251002, 105.2492070361643215, -48.57500000273119412 ) ) ;
#3735 = CARTESIAN_POINT ( 'NONE',  ( 13.14518615778179544, 33.80664062608393294, -1.609821015232357215E-15 ) ) ;
#3736 = FACE_OUTER_BOUND ( 'NONE', #14946, .T. ) ;
#3737 = CARTESIAN_POINT ( 'NONE',  ( 9.295050272127047819, 40.05742187608392868, 9.295050272127046043 ) ) ;
#3738 = CARTESIAN_POINT ( 'NONE',  ( 91.91746824999998466, 107.3738262389971680, -47.02500000273118985 ) ) ;
#3739 = CARTESIAN_POINT ( 'NONE',  ( 143.1451861577818079, 40.35507812608393863, -1.609821015232357215E-15 ) ) ;
#3740 = CARTESIAN_POINT ( 'NONE',  ( 9.295050272127047819, 32.11992187608393579, 9.295050272127046043 ) ) ;
#3741 = EDGE_LOOP ( 'NONE', ( #13883, #19434, #3079, #22446, #17485 ) ) ;
#3742 = CARTESIAN_POINT ( 'NONE',  ( 55.40115559117954547, 38.51953124999999289, -9.598844408820458085 ) ) ;
#3743 = CYLINDRICAL_SURFACE ( 'NONE', #4130, 4.999999999999989342 ) ;
#3744 = CARTESIAN_POINT ( 'NONE',  ( 201.1066586549484896, 35.99999999999998579, 11.74215035806523488 ) ) ;
#3745 = EDGE_CURVE ( 'NONE', #13023, #12136, #16133, .T. ) ;
#3746 = CARTESIAN_POINT ( 'NONE',  ( 98.15313185440925281, 4.458734125000016313, 2.250000001365591640 ) ) ;
#3747 = CARTESIAN_POINT ( 'NONE',  ( -5.444914386472297529, 34.25312500108393010, -13.14518615778179900 ) ) ;
#3748 = CARTESIAN_POINT ( 'NONE',  ( 95.54126587499996504, 1.846868145590750077, 3.625000001365592528 ) ) ;
#3749 = CARTESIAN_POINT ( 'NONE',  ( 104.4587341249999639, 81.18750000136559208, -1.442382525525748735E-14 ) ) ;
#3750 = CARTESIAN_POINT ( 'NONE',  ( -5.444914386472299306, 33.55859375108393294, 13.14518615778179722 ) ) ;
#3751 = CARTESIAN_POINT ( 'NONE',  ( 5.444914386472302859, 39.41250000108393436, 13.14518615778179189 ) ) ;
#3752 = CARTESIAN_POINT ( 'NONE',  ( 195.0000000000000000, -7.395377635281828788, -13.57481594606306707 ) ) ;
#3753 = ORIENTED_EDGE ( 'NONE', *, *, #11729, .F. ) ;
#3754 = CARTESIAN_POINT ( 'NONE',  ( -13.14518615778179544, 32.02070312608393010, 0.000000000000000000 ) ) ;
#3756 = EDGE_CURVE ( 'NONE', #13728, #10337, #8134, .T. ) ;
#3755 = CARTESIAN_POINT ( 'NONE',  ( 97.93301270000000613, 124.5000000010924879, -0.8561741729129506151 ) ) ;
#3757 = CARTESIAN_POINT ( 'NONE',  ( 99.99999999999995737, 85.00000000000000000, -1.387778780781445676E-14 ) ) ;
#3758 = CARTESIAN_POINT ( 'NONE',  ( 65.00000000000000000, -7.395377635281828788, -7.517135062566165128E-15 ) ) ;
#3759 = CARTESIAN_POINT ( 'NONE',  ( 104.9952793366501709, 103.1245878333314323, -53.17499999726882010 ) ) ;
#3760 = ADVANCED_FACE ( 'NONE', ( #1039 ), #18413, .T. ) ;
#3761 = DIRECTION ( 'NONE',  ( 0.000000000000000000, 0.000000000000000000, 1.000000000000000000 ) ) ;
#3762 = ORIENTED_EDGE ( 'NONE', *, *, #25973, .F. ) ;
#3763 = CARTESIAN_POINT ( 'NONE',  ( 55.70494972787295751, 37.47773437608393010, -9.295050272127046043 ) ) ;
#3764 = EDGE_CURVE ( 'NONE', #19447, #15410, #17090, .T. ) ;
#3765 = LINE ( 'NONE', #14155, #5523 ) ;
#3766 = CARTESIAN_POINT ( 'NONE',  ( 189.5550856135277229, 32.16953125108393152, 13.14518615778179722 ) ) ;
#3767 = ORIENTED_EDGE ( 'NONE', *, *, #27102, .T. ) ;
#3768 = CARTESIAN_POINT ( 'NONE',  ( 130.0000000000000000, 38.02343749999999289, 13.57481594606304576 ) ) ;
#3769 = DIRECTION ( 'NONE',  ( -0.000000000000000000, -0.000000000000000000, -1.000000000000000000 ) ) ;
#3770 = CIRCLE ( 'NONE', #15587, 11.57481594606304398 ) ;
#3771 = ADVANCED_FACE ( 'NONE', ( #3590 ), #8131, .T. ) ;
#3772 = CARTESIAN_POINT ( 'NONE',  ( 130.0000000000000000, 33.36015625216786873, 13.57481594606304576 ) ) ;
#3773 = CARTESIAN_POINT ( 'NONE',  ( 185.4011555911795313, 40.90078124999999432, -9.598844408820458085 ) ) ;
#3774 = FACE_OUTER_BOUND ( 'NONE', #5831, .T. ) ;
#3775 = CARTESIAN_POINT ( 'NONE',  ( 204.2950502721270425, 38.07304687608393579, -9.295050272127046043 ) ) ;
#3776 = VERTEX_POINT ( 'NONE', #6135 ) ;
#3777 = ORIENTED_EDGE ( 'NONE', *, *, #26938, .T. ) ;
#3778 = CARTESIAN_POINT ( 'NONE',  ( 98.15313185440923860, 4.458734125000016313, 13.50000000136559386 ) ) ;
#3779 = CARTESIAN_POINT ( 'NONE',  ( 99.99999999999998579, 90.75000000000000000, 4.999999999999984013 ) ) ;
#3780 = CARTESIAN_POINT ( 'NONE',  ( 102.1631189606246295, 103.3426043859339103, -51.90000000546238113 ) ) ;
#3781 = CARTESIAN_POINT ( 'NONE',  ( 5.622872871577878406, 34.20351562716788152, 13.57481594606304398 ) ) ;
#3782 = DIRECTION ( 'NONE',  ( 0.000000000000000000, 0.000000000000000000, -1.000000000000000000 ) ) ;
#3783 = LINE ( 'NONE', #25858, #15457 ) ;
#3784 = CARTESIAN_POINT ( 'NONE',  ( 10.56308295035981182, 36.00000000000000000, 8.196709705857815109 ) ) ;
#3785 = FACE_OUTER_BOUND ( 'NONE', #12144, .T. ) ;
#3786 = CARTESIAN_POINT ( 'NONE',  ( 91.91746824999997045, 112.6261737610028320, -49.72499999726881725 ) ) ;
#3787 = VECTOR ( 'NONE', #20153, 1000.000000000000000 ) ;
#3788 = VERTEX_POINT ( 'NONE', #9983 ) ;
#3789 = CARTESIAN_POINT ( 'NONE',  ( -5.622872871577873077, 40.05742187499999574, -13.57481594606304753 ) ) ;
#3790 = CARTESIAN_POINT ( 'NONE',  ( 13.57481594606304576, 31.97109375216787441, -1.662435489736055892E-15 ) ) ;
#3791 = CARTESIAN_POINT ( 'NONE',  ( 94.99999999999995737, 1.387778780781445676E-14, 4.125000002731185056 ) ) ;
#3792 = CARTESIAN_POINT ( 'NONE',  ( 120.7049497278729575, 31.72304687608393081, -9.295050272127046043 ) ) ;
#3793 = CARTESIAN_POINT ( 'NONE',  ( 65.00000000000000000, 37.18007812608393436, -13.14518615778179544 ) ) ;
#3794 = EDGE_CURVE ( 'NONE', #25494, #26327, #6565, .T. ) ;
#3795 = CARTESIAN_POINT ( 'NONE',  ( 91.91746824999998466, 110.0000000000000000, -45.74999999726882294 ) ) ;
#3796 = CARTESIAN_POINT ( 'NONE',  ( 9.295050272127047819, 36.08867187608392868, 9.295050272127046043 ) ) ;
#3797 = CARTESIAN_POINT ( 'NONE',  ( 181.8258427830772916, 35.99999999999999289, 0.03826467346029673727 ) ) ;
#3798 = DIRECTION ( 'NONE',  ( -0.000000000000000000, 1.000000000000000000, -0.000000000000000000 ) ) ;
#3799 = CARTESIAN_POINT ( 'NONE',  ( -20.00000000000000000, 50.00000000000000000, 10.00000000000000178 ) ) ;
#3800 = PRESENTATION_STYLE_ASSIGNMENT (( #16485 ) ) ;
#3801 = CARTESIAN_POINT ( 'NONE',  ( 13.14518615778179900, 38.51953125108393294, 5.444914386472293977 ) ) ;
#3802 = CARTESIAN_POINT ( 'NONE',  ( 136.3519322287719717, 36.00000000000000000, 11.61660627739482621 ) ) ;
#3803 = CARTESIAN_POINT ( 'NONE',  ( 101.0355339059327378, 124.7500000000000142, -2.499999999999997780 ) ) ;
#3804 = CARTESIAN_POINT ( 'NONE',  ( 99.14382582708707048, 123.3000000010924708, 2.066987299999979211 ) ) ;
#3805 = CARTESIAN_POINT ( 'NONE',  ( 98.53841926354351699, 124.0500000010924708, 1.461580736456455920 ) ) ;
#3806 = VECTOR ( 'NONE', #3707, 1000.000000000000000 ) ;
#3807 = DIRECTION ( 'NONE',  ( -0.000000000000000000, -0.000000000000000000, -1.000000000000000000 ) ) ;
#3808 = CARTESIAN_POINT ( 'NONE',  ( 99.99999999999995737, 4.458734125000016313, 14.18750000136559208 ) ) ;
#3809 = CARTESIAN_POINT ( 'NONE',  ( -13.57481594606304398, 32.41757812716787868, 5.622872871577880183 ) ) ;
#3810 = VERTEX_POINT ( 'NONE', #1456 ) ;
#3811 = CARTESIAN_POINT ( 'NONE',  ( 98.23223304703363112, 123.6000000021849416, 1.767766952966351557 ) ) ;
#3812 = CARTESIAN_POINT ( 'NONE',  ( 9.598844408820456309, 40.70234374999999716, -9.598844408820458085 ) ) ;
#3813 = CARTESIAN_POINT ( 'NONE',  ( 5.444914386472297529, 33.95546875108394147, -13.14518615778179722 ) ) ;
#3814 = CARTESIAN_POINT ( 'NONE',  ( -8.312177448680279460E-16, 31.37578125216787583, -13.57481594606304576 ) ) ;
#3815 = DIRECTION ( 'NONE',  ( -0.000000000000000000, 1.000000000000000000, -0.000000000000000000 ) ) ;
#3816 = CARTESIAN_POINT ( 'NONE',  ( 95.54126587499995082, 80.37500000136562051, -1.846868145590750077 ) ) ;
#3817 = CARTESIAN_POINT ( 'NONE',  ( 78.14518615778179367, 39.51171875108392584, 5.444914386472293977 ) ) ;
#3818 = CARTESIAN_POINT ( 'NONE',  ( 91.91746824999998466, 107.3738262389971538, -49.27500000273118985 ) ) ;
#3819 =( BOUNDED_CURVE ( )  B_SPLINE_CURVE ( 2, ( #22835, #7564, #1451, #16258, #1177, #18820, #16682, #25381, #9843 ),
 .UNSPECIFIED., .F., .F. ) 
 B_SPLINE_CURVE_WITH_KNOTS ( ( 3, 2, 2, 2, 3 ),
 ( 0.1041666666666664909, 0.1145833333333332732, 0.1250000000000000833, 0.1354166666666668517, 0.1458333333333336757 ),
 .UNSPECIFIED. ) 
 CURVE ( )  GEOMETRIC_REPRESENTATION_ITEM ( )  RATIONAL_B_SPLINE_CURVE ( ( 1.000000000000001332, 0.9238795325112854062, 1.000000000000000000, 0.9238795325112867385, 1.000000000000000000, 0.9238795325112867385, 1.000000000000000000, 0.9238795325112842960, 1.000000000000002442 ) ) 
 REPRESENTATION_ITEM ( '' )  );
#3820 = CARTESIAN_POINT ( 'NONE',  ( 100.8561741729129153, 124.5000000010924737, -2.066987299999999195 ) ) ;
#3821 = CARTESIAN_POINT ( 'NONE',  ( 102.4999999999999858, 123.0000000000000000, -8.724596124144689908E-15 ) ) ;
#3822 = CARTESIAN_POINT ( 'NONE',  ( 107.0000000000000000, 112.2744378736303332, -49.39999999453763735 ) ) ;
#3823 = CARTESIAN_POINT ( 'NONE',  ( 116.4251840539369454, 39.36289062499999858, -5.622872871577873077 ) ) ;
#3824 = VERTEX_POINT ( 'NONE', #4002 ) ;
#3825 = CARTESIAN_POINT ( 'NONE',  ( -1.501019124304961982, 53.60014735326988244, -14.99999999999999822 ) ) ;
#3826 = CARTESIAN_POINT ( 'NONE',  ( 5.444914386472297529, 39.71015625108393010, -13.14518615778179900 ) ) ;
#3827 = CARTESIAN_POINT ( 'NONE',  ( -8.312177448680279460E-16, 40.10703125216787157, -13.57481594606304576 ) ) ;
#3828 = CARTESIAN_POINT ( 'NONE',  ( 139.2950502721270425, 39.46210937608393010, -9.295050272127046043 ) ) ;
#3829 = CARTESIAN_POINT ( 'NONE',  ( 74.59884440882045453, 36.83281250216787583, -9.598844408820458085 ) ) ;
#3830 = CARTESIAN_POINT ( 'NONE',  ( 106.5389055433250860, 105.2492070361643215, -52.82499999726881867 ) ) ;
#3831 = CARTESIAN_POINT ( 'NONE',  ( -9.598844408820458085, 36.23750000216787726, -9.598844408820458085 ) ) ;
#3832 = ORIENTED_EDGE ( 'NONE', *, *, #13926, .T. ) ;
#3833 = CARTESIAN_POINT ( 'NONE',  ( 103.5355339059327093, -3.535533905932726206, 8.375000000000000000 ) ) ;
#3834 = CARTESIAN_POINT ( 'NONE',  ( 93.00000000000000000, 112.2744378736303190, -52.10000000000000142 ) ) ;
#3835 = CARTESIAN_POINT ( 'NONE',  ( 5.444914386472302859, 34.65000000108393863, 13.14518615778179189 ) ) ;
#3836 = CARTESIAN_POINT ( 'NONE',  ( 200.4449143864723055, 36.33671875108394289, -13.14518615778179900 ) ) ;
#3837 = LINE ( 'NONE', #18674, #6926 ) ;
#3838 = CARTESIAN_POINT ( 'NONE',  ( 124.5550856135277087, 36.73359375108393010, 13.14518615778179722 ) ) ;
#3839 = CARTESIAN_POINT ( 'NONE',  ( 102.4999999999999858, 122.3500000021849701, -1.035533905932742638 ) ) ;
#3840 = EDGE_CURVE ( 'NONE', #16572, #23831, #15188, .T. ) ;
#3841 = CARTESIAN_POINT ( 'NONE',  ( 130.0000000000000000, 37.62656249999999858, -13.57481594606304576 ) ) ;
#3842 = CARTESIAN_POINT ( 'NONE',  ( 0.000000000000000000, 0.4999999999999970024, 0.000000000000000000 ) ) ;
#3843 = DIRECTION ( 'NONE',  ( -0.000000000000000000, 1.000000000000000000, -0.000000000000000000 ) ) ;
#3844 = FACE_OUTER_BOUND ( 'NONE', #19807, .T. ) ;
#3845 = CARTESIAN_POINT ( 'NONE',  ( 204.5988444088204687, 38.91640624999999432, 9.598844408820456309 ) ) ;
#3846 = APPLICATION_PROTOCOL_DEFINITION ( 'draft international standard', 'automotive_design', 1998, #25524 ) ;
#3847 = CARTESIAN_POINT ( 'NONE',  ( 104.9999999999999716, -2.071067811865462627, 8.562500002731185944 ) ) ;
#3848 = CARTESIAN_POINT ( 'NONE',  ( 104.4587341249999781, -1.846868145590721655, 1.125000001365592750 ) ) ;
#3849 = CARTESIAN_POINT ( 'NONE',  ( 55.70494972787295751, 38.27148437608393294, 9.295050272127047819 ) ) ;
#3850 = CARTESIAN_POINT ( 'NONE',  ( 95.54126587499996504, 1.387778780781445676E-14, 7.437500001365592084 ) ) ;
#3851 = CARTESIAN_POINT ( 'NONE',  ( 102.1631189606246295, 103.3426043859339103, -49.90000000546238113 ) ) ;
#3852 = CARTESIAN_POINT ( 'NONE',  ( 99.99999999999998579, 93.81249999863440792, -4.458734124999994997 ) ) ;
#3853 = CARTESIAN_POINT ( 'NONE',  ( 107.0000000000000142, 110.0000000000000000, -55.00000000000000711 ) ) ;
#3854 = CARTESIAN_POINT ( 'NONE',  ( -9.598844408820454532, 39.51171874999999289, 9.598844408820459861 ) ) ;
#3855 = CARTESIAN_POINT ( 'NONE',  ( 99.99999999999998579, 124.1000000021849416, -2.499999999999997780 ) ) ;
#3856 = ORIENTED_EDGE ( 'NONE', *, *, #7501, .T. ) ;
#3857 = CARTESIAN_POINT ( 'NONE',  ( 101.8468681455906903, 82.00000000136560629, 4.458734124999987891 ) ) ;
#3858 = VECTOR ( 'NONE', #3338, 1000.000000000000000 ) ;
#3859 = CARTESIAN_POINT ( 'NONE',  ( 104.4587341249999923, 91.24999999863439371, 1.846868145590726318 ) ) ;
#3860 = EDGE_LOOP ( 'NONE', ( #20155, #26876, #23303 ) ) ;
#3861 =( BOUNDED_CURVE ( )  B_SPLINE_CURVE ( 2, ( #24797, #22525, #5804, #3664, #14606, #7544, #21182, #1664, #6075 ),
 .UNSPECIFIED., .F., .T. ) 
 B_SPLINE_CURVE_WITH_KNOTS ( ( 3, 2, 2, 2, 3 ),
 ( 0.4791666666666667962, 0.4895833333333333703, 0.5000000000000000000, 0.5104166666666665186, 0.5208333333333332593 ),
 .UNSPECIFIED. ) 
 CURVE ( )  GEOMETRIC_REPRESENTATION_ITEM ( )  RATIONAL_B_SPLINE_CURVE ( ( 0.9999999999999992228, 0.9238795325112875156, 1.000000000000000000, 0.9238795325112867385, 1.000000000000000000, 0.9238795325112867385, 1.000000000000000000, 0.9238795325112875156, 0.9999999999999992228 ) ) 
 REPRESENTATION_ITEM ( '' )  );
#3862 = CARTESIAN_POINT ( 'NONE',  ( 99.99999999999998579, 94.62499999726881583, 4.999999999999984013 ) ) ;
#3863 = VERTEX_POINT ( 'NONE', #12247 ) ;
#3864 = CARTESIAN_POINT ( 'NONE',  ( -9.598844408820458085, 33.06250000216787299, -9.598844408820458085 ) ) ;
#3865 = CARTESIAN_POINT ( 'NONE',  ( 99.99999999999995737, 4.458734125000016313, 6.437500001365592084 ) ) ;
#3866 = ORIENTED_EDGE ( 'NONE', *, *, #18381, .F. ) ;
#3867 = CARTESIAN_POINT ( 'NONE',  ( -8.049105076161786076E-16, 35.79101562608394005, -13.14518615778179544 ) ) ;
#3868 = CARTESIAN_POINT ( 'NONE',  ( 13.14518615778179544, 33.01289062608393010, -1.609821015232357215E-15 ) ) ;
#3869 = CARTESIAN_POINT ( 'NONE',  ( 181.4251840539369596, 38.76757812716787299, 5.622872871577880183 ) ) ;
#3870 = CARTESIAN_POINT ( 'NONE',  ( 5.444914386472302859, 40.00781250108393294, 13.14518615778179189 ) ) ;
#3871 = CARTESIAN_POINT ( 'NONE',  ( -8.312177448680279460E-16, 31.37578125216787583, -13.57481594606304576 ) ) ;
#3872 = CARTESIAN_POINT ( 'NONE',  ( 190.4284083674847636, 51.44262710532314742, 15.00000000000126654 ) ) ;
#3873 = CARTESIAN_POINT ( 'NONE',  ( 116.8548138422182205, 40.75195312608393294, 0.000000000000000000 ) ) ;
#3874 = CARTESIAN_POINT ( 'NONE',  ( -5.444914386472299306, 33.55859375108393294, 13.14518615778179722 ) ) ;
#3875 = EDGE_CURVE ( 'NONE', #25304, #12114, #13949, .T. ) ;
#3876 = AXIS2_PLACEMENT_3D ( 'NONE', #21322, #21044, #18763 ) ;
#3877 = VERTEX_POINT ( 'NONE', #25792 ) ;
#3878 = CARTESIAN_POINT ( 'NONE',  ( 65.00000000000000000, 37.62656249999999858, -13.57481594606304576 ) ) ;
#3879 = CARTESIAN_POINT ( 'NONE',  ( 97.50000000000000000, 124.6500000010924651, -9.540979117872439019E-15 ) ) ;
#3880 = CARTESIAN_POINT ( 'NONE',  ( 99.99999999999998579, 117.3602355696678643, -46.50000000000000711 ) ) ;
#3881 = CARTESIAN_POINT ( 'NONE',  ( 99.99999999999995737, -4.458734124999988779, 5.687500001365591196 ) ) ;
#3882 = CARTESIAN_POINT ( 'NONE',  ( -13.14518615778179544, 32.81445312608393294, 0.000000000000000000 ) ) ;
#3883 = CARTESIAN_POINT ( 'NONE',  ( 98.15313185440923860, -4.458734124999987891, 1.875000001365591862 ) ) ;
#3884 = CARTESIAN_POINT ( 'NONE',  ( 104.4587341249999639, 83.18750000136560629, -1.442382525525748735E-14 ) ) ;
#3885 = CARTESIAN_POINT ( 'NONE',  ( -8.049105076161786076E-16, 32.41757812608393863, -13.14518615778179544 ) ) ;
#3886 = CARTESIAN_POINT ( 'NONE',  ( -8.049105076161786076E-16, 38.96601562608393721, -13.14518615778179544 ) ) ;
#3887 = FACE_OUTER_BOUND ( 'NONE', #9286, .T. ) ;
#3888 = ORIENTED_EDGE ( 'NONE', *, *, #440, .T. ) ;
#3889 = CARTESIAN_POINT ( 'NONE',  ( 13.14518615778179722, 32.36796875108393579, 5.444914386472293977 ) ) ;
#3890 = DIRECTION ( 'NONE',  ( 0.000000000000000000, 0.000000000000000000, 1.000000000000000000 ) ) ;
#3891 = CARTESIAN_POINT ( 'NONE',  ( 98.15313185440923860, 94.24999999863439371, 4.458734124999980786 ) ) ;
#3892 = CARTESIAN_POINT ( 'NONE',  ( 104.9999999999999716, -2.071067811865462627, 3.562500002731184612 ) ) ;
#3893 = CARTESIAN_POINT ( 'NONE',  ( 100.4820290753432488, 123.0000000000000284, -2.155989633091683011 ) ) ;
#3894 = CIRCLE ( 'NONE', #23465, 7.000000000000006217 ) ;
#3895 = CARTESIAN_POINT ( 'NONE',  ( -9.598844408820454532, 32.36796874999999574, 9.598844408820459861 ) ) ;
#3896 = VERTEX_POINT ( 'NONE', #19241 ) ;
#3897 = CARTESIAN_POINT ( 'NONE',  ( 74.29505027212704249, 38.07304687608393579, -9.295050272127046043 ) ) ;
#3898 = CYLINDRICAL_SURFACE ( 'NONE', #24842, 7.000000000000006217 ) ;
#3899 = CARTESIAN_POINT ( 'NONE',  ( 2.493653234604083739E-15, 34.84843749999999574, 13.57481594606304576 ) ) ;
#3900 = EDGE_CURVE ( 'NONE', #21810, #18157, #27942, .T. ) ;
#3901 = ORIENTED_EDGE ( 'NONE', *, *, #11311, .F. ) ;
#3902 = CARTESIAN_POINT ( 'NONE',  ( 97.92893218813449607, 92.31249999999997158, -4.999999999999971578 ) ) ;
#3903 = CARTESIAN_POINT ( 'NONE',  ( -3.979814445820054392, 50.00000000123264954, -13.01613927312573793 ) ) ;
#3904 = AXIS2_PLACEMENT_3D ( 'NONE', #10327, #25180, #21720 ) ;
#3905 = CARTESIAN_POINT ( 'NONE',  ( 97.93301269999999192, 124.0000000010924879, 0.8561741729129329626 ) ) ;
#3906 = CARTESIAN_POINT ( 'NONE',  ( 143.5748159460630404, 34.40195312716787157, -5.622872871577873077 ) ) ;
#3907 = CARTESIAN_POINT ( 'NONE',  ( 51.85481384221820633, 40.00781250108393294, 5.444914386472304635 ) ) ;
#3908 = ADVANCED_FACE ( 'NONE', ( #27396 ), #23953, .T. ) ;
#3909 = CARTESIAN_POINT ( 'NONE',  ( -18.00000000000000711, 78.00000000000000000, -12.99999999999999822 ) ) ;
#3910 = CARTESIAN_POINT ( 'NONE',  ( 208.1451861577818079, 37.97382812608393721, -1.609821015232357215E-15 ) ) ;
#3911 = ORIENTED_EDGE ( 'NONE', *, *, #26252, .T. ) ;
#3912 = ORIENTED_EDGE ( 'NONE', *, *, #27435, .F. ) ;
#3913 = EDGE_CURVE ( 'NONE', #10042, #17637, #8373, .T. ) ;
#3914 = VERTEX_POINT ( 'NONE', #20803 ) ;
#3915 = CARTESIAN_POINT ( 'NONE',  ( -13.14518615778179189, 33.45937500108392726, 5.444914386472304635 ) ) ;
#3916 = SURFACE_STYLE_FILL_AREA ( #25572 ) ;
#3917 = LINE ( 'NONE', #1643, #8440 ) ;
#3918 = CARTESIAN_POINT ( 'NONE',  ( 13.57481594606304931, 38.17226562499999432, 5.622872871577868636 ) ) ;
#3919 = ADVANCED_FACE ( 'NONE', ( #19066 ), #23048, .T. ) ;
#3920 = CARTESIAN_POINT ( 'NONE',  ( 103.5355339059327093, 3.535533905932755072, 13.62500000000000000 ) ) ;
#3921 = DIRECTION ( 'NONE',  ( -1.000000000000000000, 0.000000000000000000, 0.000000000000000000 ) ) ;
#3922 = CARTESIAN_POINT ( 'NONE',  ( 94.99999999999995737, 1.387778780781445676E-14, 34.79898987322334136 ) ) ;
#3923 = FACE_OUTER_BOUND ( 'NONE', #4866, .T. ) ;
#3924 = AXIS2_PLACEMENT_3D ( 'NONE', #18616, #20896, #1378 ) ;
#3925 = CARTESIAN_POINT ( 'NONE',  ( 104.9999999999999716, 1.449011120738813565E-14, 6.499999999999999112 ) ) ;
#3926 = DIRECTION ( 'NONE',  ( -0.000000000000000000, 1.000000000000000000, -0.000000000000000000 ) ) ;
#3927 = CARTESIAN_POINT ( 'NONE',  ( 143.5748159460630404, 32.61601562499999574, 5.622872871577869525 ) ) ;
#3928 = ADVANCED_FACE ( 'NONE', ( #16156 ), #9046, .T. ) ;
#3929 = ORIENTED_EDGE ( 'NONE', *, *, #17022, .T. ) ;
#3930 = CARTESIAN_POINT ( 'NONE',  ( 13.57481594606304753, 39.85898437499999858, -5.622872871577873077 ) ) ;
#3931 = CARTESIAN_POINT ( 'NONE',  ( -5.444914386472297529, 38.81718750108393579, -13.14518615778179900 ) ) ;
#3932 = CARTESIAN_POINT ( 'NONE',  ( 97.92893218813451028, -4.999999999999989342, 3.312500002731184612 ) ) ;
#3933 = CARTESIAN_POINT ( 'NONE',  ( 120.7049497278729575, 40.05742187608393579, 9.295050272127047819 ) ) ;
#3934 = CARTESIAN_POINT ( 'NONE',  ( 55.70494972787295751, 36.48554687608393721, -9.295050272127046043 ) ) ;
#3935 = CARTESIAN_POINT ( 'NONE',  ( 185.7049497278729575, 32.51679687608393721, -9.295050272127046043 ) ) ;
#3936 = PLANE ( 'NONE',  #11130 ) ;
#3937 = CARTESIAN_POINT ( 'NONE',  ( 9.295050272127047819, 36.88242187608393152, 9.295050272127046043 ) ) ;
#3938 = CARTESIAN_POINT ( 'NONE',  ( 195.3745404134769785, 35.99999999999998579, -13.51869779562198381 ) ) ;
#3939 = CIRCLE ( 'NONE', #3023, 2.499999999999995115 ) ;
#3940 = CARTESIAN_POINT ( 'NONE',  ( 189.4309414480975704, 36.00000000000000000, 11.91493531101289882 ) ) ;
#3941 = EDGE_CURVE ( 'NONE', #3615, #25660, #21527, .T. ) ;
#3942 = CYLINDRICAL_SURFACE ( 'NONE', #336, 10.50000000000001599 ) ;
#3943 = CARTESIAN_POINT ( 'NONE',  ( 5.444914386472302859, 39.21406250108392300, 13.14518615778179189 ) ) ;
#3944 = VECTOR ( 'NONE', #21325, 1000.000000000000000 ) ;
#3945 = CARTESIAN_POINT ( 'NONE',  ( -7.623941961925451594, 55.00000000000000000, 14.99999999999999645 ) ) ;
#3946 = CARTESIAN_POINT ( 'NONE',  ( 101.0355339059327378, 123.9500000000000028, -2.499999999999997780 ) ) ;
#3947 = CARTESIAN_POINT ( 'NONE',  ( 130.0000000000000000, -7.395377635281828788, -1.503427012513233026E-14 ) ) ;
#3948 = CARTESIAN_POINT ( 'NONE',  ( 102.0669873000000081, 123.5000000010924737, 0.8561741729129311862 ) ) ;
#3949 = EDGE_CURVE ( 'NONE', #21855, #19872, #18453, .T. ) ;
#3950 = CARTESIAN_POINT ( 'NONE',  ( 101.8468681455906903, 4.458734125000016313, 14.12500000136559208 ) ) ;
#3951 = CARTESIAN_POINT ( 'NONE',  ( 130.0000000000000000, 38.51953125216787299, -13.57481594606304576 ) ) ;
#3952 = ORIENTED_EDGE ( 'NONE', *, *, #17696, .F. ) ;
#3953 = CARTESIAN_POINT ( 'NONE',  ( 93.00000000000001421, 107.7255621263696241, -50.39999999453763024 ) ) ;
#3954 = CARTESIAN_POINT ( 'NONE',  ( 13.57481594606304576, 40.60312499999999858, -1.662435489736055892E-15 ) ) ;
#3955 = CARTESIAN_POINT ( 'NONE',  ( -5.444914386472297529, 31.67343750108393863, -13.14518615778179722 ) ) ;
#3956 = ADVANCED_FACE ( 'NONE', ( #22873 ), #25655, .F. ) ;
#3957 = CARTESIAN_POINT ( 'NONE',  ( 13.57481594606304931, 31.92148437716787512, 5.622872871577869525 ) ) ;
#3958 = CARTESIAN_POINT ( 'NONE',  ( 104.9999999999999574, 2.071067811865511032, 2.562499999999999556 ) ) ;
#3959 = CARTESIAN_POINT ( 'NONE',  ( 101.8468681455906903, 80.12500000136560629, -4.458734125000016313 ) ) ;
#3960 = CARTESIAN_POINT ( 'NONE',  ( 65.00000000000000000, 38.17226562608394147, -13.14518615778179544 ) ) ;
#3961 = CARTESIAN_POINT ( 'NONE',  ( 108.0825317500000011, 112.6261737610028320, -48.27500000273119696 ) ) ;
#3962 = CARTESIAN_POINT ( 'NONE',  ( -8.049105076161786076E-16, 40.35507812608393152, -13.14518615778179544 ) ) ;
#3963 = AXIS2_PLACEMENT_3D ( 'NONE', #20723, #23383, #6408 ) ;
#3964 = LINE ( 'NONE', #14903, #24861 ) ;
#3965 = CARTESIAN_POINT ( 'NONE',  ( 59.37712712842218110, 38.56914062716787583, -13.57481594606310260 ) ) ;
#3966 = CARTESIAN_POINT ( 'NONE',  ( 93.00000000000000000, 112.2744378736303332, -50.59999999453763309 ) ) ;
#3967 = CARTESIAN_POINT ( 'NONE',  ( 130.0000000000000000, 31.82226562608393650, -13.14518615778179544 ) ) ;
#3968 = ORIENTED_EDGE ( 'NONE', *, *, #11866, .F. ) ;
#3969 = CARTESIAN_POINT ( 'NONE',  ( 103.5355339059327093, 3.535533905932755072, 7.624999999999999112 ) ) ;
#3970 = CYLINDRICAL_SURFACE ( 'NONE', #27177, 13.57481594606304398 ) ;
#3971 = CARTESIAN_POINT ( 'NONE',  ( 99.99999999999995737, 81.18750000136559208, -4.458734125000016313 ) ) ;
#3972 = CARTESIAN_POINT ( 'NONE',  ( 143.1451861577818079, 40.10703125108393152, 5.444914386472293977 ) ) ;
#3973 = CARTESIAN_POINT ( 'NONE',  ( 59.37712712842213136, 38.56914062716788294, -13.57481594606304753 ) ) ;
#3974 = CARTESIAN_POINT ( 'NONE',  ( 108.0825317500000011, 110.0000000000000000, -52.62499999726882294 ) ) ;
#3975 = CARTESIAN_POINT ( 'NONE',  ( 5.622872871577878406, 34.99726562716787726, 13.57481594606304576 ) ) ;
#3976 = VERTEX_POINT ( 'NONE', #6137 ) ;
#3977 = CARTESIAN_POINT ( 'NONE',  ( 97.92893218813451028, 5.000000000000018652, 6.812499999999999112 ) ) ;
#3978 = ORIENTED_EDGE ( 'NONE', *, *, #26236, .F. ) ;
#3979 = CARTESIAN_POINT ( 'NONE',  ( 195.0000000000000000, 35.98945312608393010, 13.14518615778179544 ) ) ;
#3980 = CLOSED_SHELL ( 'NONE', ( #3417, #18569, #824, #23023, #19804, #19694, #21880, #22070, #12567, #8474, #205, #21637, #26572, #19130, #7546, #12067, #18198, #3209, #6160, #23117, #22791, #9244, #12595, #12804, #18563, #25354, #460, #26694, #24822, #16692, #11939, #21191, #12947, #11029 ) ) ;
#3981 = ADVANCED_FACE ( 'NONE', ( #8403 ), #25003, .F. ) ;
#3982 = CARTESIAN_POINT ( 'NONE',  ( 124.5550856135277087, 37.22968750108394431, -13.14518615778179722 ) ) ;
#3983 = CARTESIAN_POINT ( 'NONE',  ( 101.7677669529663547, 122.4000000021849530, -1.767766952966370209 ) ) ;
#3984 = DIRECTION ( 'NONE',  ( 0.000000000000000000, -2.775557561562890720E-14, -1.000000000000000000 ) ) ;
#3985 = DIRECTION ( 'NONE',  ( -0.000000000000000000, -1.000000000000000000, -0.000000000000000000 ) ) ;
#3986 = LINE ( 'NONE', #23782, #5722 ) ;
#3987 =( BOUNDED_CURVE ( )  B_SPLINE_CURVE ( 2, ( #14435, #3627, #5766, #16993, #25693, #6176, #16442, #9885, #23565 ),
 .UNSPECIFIED., .F., .T. ) 
 B_SPLINE_CURVE_WITH_KNOTS ( ( 3, 2, 2, 2, 3 ),
 ( 0.1458333333333336757, 0.1562500000000002776, 0.1666666666666669072, 0.1770833333333335369, 0.1875000000000001388 ),
 .UNSPECIFIED. ) 
 CURVE ( )  GEOMETRIC_REPRESENTATION_ITEM ( )  RATIONAL_B_SPLINE_CURVE ( ( 0.9999999999999975575, 0.9238795325112891810, 1.000000000000000000, 0.9238795325112867385, 1.000000000000000000, 0.9238795325112867385, 1.000000000000000000, 0.9238795325112857393, 1.000000000000001110 ) ) 
 REPRESENTATION_ITEM ( '' )  );
#3988 = CARTESIAN_POINT ( 'NONE',  ( -8.049105076161786076E-16, 40.35507812608393152, -13.14518615778179544 ) ) ;
#3989 = CARTESIAN_POINT ( 'NONE',  ( 181.4251840539369596, 36.28710937499999289, 5.622872871577880183 ) ) ;
#3990 = SHAPE_DEFINITION_REPRESENTATION ( #8986, #17883 ) ;
#3991 = CARTESIAN_POINT ( 'NONE',  ( 104.9999999999999716, 1.449011120738813565E-14, 8.625000002731185944 ) ) ;
#3992 = CARTESIAN_POINT ( 'NONE',  ( 95.54126587499995082, -1.846868145590724986, 3.750000001365591640 ) ) ;
#3993 = CARTESIAN_POINT ( 'NONE',  ( 78.14518615778179367, 38.61875000108393152, -5.444914386472297529 ) ) ;
#3994 = CARTESIAN_POINT ( 'NONE',  ( 96.84719886470459471, 3.152801135295383084, 4.312500001365592084 ) ) ;
#3995 = CARTESIAN_POINT ( 'NONE',  ( 99.99999999999998579, 95.62499999726881583, 4.999999999999984013 ) ) ;
#3996 = CARTESIAN_POINT ( 'NONE',  ( 96.84719886470463734, 93.18749999863440792, 3.152801135295351997 ) ) ;
#3997 = DIRECTION ( 'NONE',  ( -0.000000000000000000, -1.000000000000000000, -0.000000000000000000 ) ) ;
#3998 = CARTESIAN_POINT ( 'NONE',  ( -8.312177448680279460E-16, 38.42031249999999432, -13.57481594606304576 ) ) ;
#3999 = CARTESIAN_POINT ( 'NONE',  ( 99.99999999999998579, 102.6397644303321215, -45.50000000000000000 ) ) ;
#4000 = ORIENTED_EDGE ( 'NONE', *, *, #10677, .T. ) ;
#4001 = CARTESIAN_POINT ( 'NONE',  ( 101.8468681455906903, 84.00000000136560629, 4.458734124999987891 ) ) ;
#4002 = CARTESIAN_POINT ( 'NONE',  ( 99.99999999999998579, 136.0000000000000000, 10.50000000000001066 ) ) ;
#4003 = VERTEX_POINT ( 'NONE', #1218 ) ;
#4004 = CARTESIAN_POINT ( 'NONE',  ( 104.3262379212492448, 104.0454443415356991, -46.30000000000001847 ) ) ;
#4005 = CARTESIAN_POINT ( 'NONE',  ( 55.70494972787295751, 35.29492187608393294, 9.295050272127047819 ) ) ;
#4006 = ORIENTED_EDGE ( 'NONE', *, *, #12484, .T. ) ;
#4007 = DIRECTION ( 'NONE',  ( 5.782411586589358625E-17, -0.000000000000000000, 1.000000000000000000 ) ) ;
#4008 = CARTESIAN_POINT ( 'NONE',  ( 98.15313185440925281, 4.458734125000016313, 3.500000001365592528 ) ) ;
#4009 = VERTEX_POINT ( 'NONE', #3862 ) ;
#4010 = FACE_OUTER_BOUND ( 'NONE', #7858, .T. ) ;
#4011 = CARTESIAN_POINT ( 'NONE',  ( 13.14518615778179544, 34.60039062608392868, -1.609821015232357215E-15 ) ) ;
#4012 = CARTESIAN_POINT ( 'NONE',  ( 200.6228728715778686, 38.17226562716786731, 13.57481594606304576 ) ) ;
#4013 = CARTESIAN_POINT ( 'NONE',  ( 13.14518615778179722, 38.51953125108393294, 5.444914386472293977 ) ) ;
#4014 = CARTESIAN_POINT ( 'NONE',  ( 130.0000000000000000, 36.00000000000000000, -1.503427012513233026E-14 ) ) ;
#4015 = CARTESIAN_POINT ( 'NONE',  ( 204.1801758136480203, 55.00000000000000711, 14.99999999999994671 ) ) ;
#4016 = CARTESIAN_POINT ( 'NONE',  ( 120.7049497278729575, 39.06523437608392868, -9.295050272127046043 ) ) ;
#4017 = CARTESIAN_POINT ( 'NONE',  ( 13.14518615778179900, 39.61093750108393863, -5.444914386472297529 ) ) ;
#4018 = ORIENTED_EDGE ( 'NONE', *, *, #26747, .F. ) ;
#4019 = CARTESIAN_POINT ( 'NONE',  ( 74.59884440882045453, 37.32890624999999574, 9.598844408820456309 ) ) ;
#4020 = CARTESIAN_POINT ( 'NONE',  ( 0.000000000000000000, 0.4999999999999970024, 22.40192378864669465 ) ) ;
#4021 = AXIS2_PLACEMENT_3D ( 'NONE', #3543, #1411, #25063 ) ;
#4022 = CARTESIAN_POINT ( 'NONE',  ( 104.4587341249999781, -1.846868145590721655, 0.8750000013655926390 ) ) ;
#4023 = CARTESIAN_POINT ( 'NONE',  ( 198.3041185978229350, 36.00000000000001421, 12.77244747738234487 ) ) ;
#4024 = CARTESIAN_POINT ( 'NONE',  ( 98.15313185440925281, 4.458734125000016313, 3.250000001365592528 ) ) ;
#4025 = CARTESIAN_POINT ( 'NONE',  ( 106.5389055433251002, 114.7507929638356785, -51.92500000273119554 ) ) ;
#4026 = CARTESIAN_POINT ( 'NONE',  ( 102.4999999999999858, 123.7500000000000142, 1.035533905932722876 ) ) ;
#4027 = CARTESIAN_POINT ( 'NONE',  ( 95.54126587499996504, 1.387778780781445676E-14, 4.687500001365592084 ) ) ;
#4028 = CARTESIAN_POINT ( 'NONE',  ( 96.84719886470459471, 79.81250000136559208, 3.152801135295355994 ) ) ;
#4029 = CARTESIAN_POINT ( 'NONE',  ( 3.755638265659908104, 31.58960998161716560, -13.14518615778179900 ) ) ;
#4030 = CARTESIAN_POINT ( 'NONE',  ( 9.295050272127047819, 40.25585937608393294, 9.295050272127046043 ) ) ;
#4031 = CARTESIAN_POINT ( 'NONE',  ( 104.9952793366501709, 103.1245878333314323, -47.17499999726881299 ) ) ;
#4032 = ORIENTED_EDGE ( 'NONE', *, *, #3440, .F. ) ;
#4033 =( BOUNDED_CURVE ( )  B_SPLINE_CURVE ( 2, ( #1141, #7816, #5407, #1274, #20793, #18512, #14218, #3686, #14494, #27219, #11792 ),
 .UNSPECIFIED., .F., .F. ) 
 B_SPLINE_CURVE_WITH_KNOTS ( ( 3, 2, 2, 2, 2, 3 ),
 ( 0.1000000000000000056, 0.1200000000000000233, 0.1400000000000000688, 0.1600000000000001144, 0.1800000000000001044, 0.2000000000000001776 ),
 .UNSPECIFIED. ) 
 CURVE ( )  GEOMETRIC_REPRESENTATION_ITEM ( )  RATIONAL_B_SPLINE_CURVE ( ( 1.000000000000000000, 0.9510565162951535312, 1.000000000000000000, 0.9510565162951535312, 1.000000000000000000, 0.9510565162951535312, 1.000000000000000000, 0.9510565162951535312, 1.000000000000000000, 0.9510565162951530871, 1.000000000000000444 ) ) 
 REPRESENTATION_ITEM ( '' )  );
#4034 = DIRECTION ( 'NONE',  ( 0.000000000000000000, 0.000000000000000000, 1.000000000000000000 ) ) ;
#4035 = CARTESIAN_POINT ( 'NONE',  ( 102.0710678118654329, 5.000000000000018652, 5.687500000000000000 ) ) ;
#4036 = CARTESIAN_POINT ( 'NONE',  ( 99.99999999999995737, 82.37500000273119838, 4.999999999999990230 ) ) ;
#4037 = CARTESIAN_POINT ( 'NONE',  ( 106.5389055433250860, 105.2492070361643215, -53.07499999726881867 ) ) ;
#4038 = EDGE_CURVE ( 'NONE', #4887, #506, #27532, .T. ) ;
#4039 = CARTESIAN_POINT ( 'NONE',  ( 189.5550856135277229, 39.61093750108393152, -13.14518615778179900 ) ) ;
#4040 = VERTEX_POINT ( 'NONE', #17092 ) ;
#4041 = CARTESIAN_POINT ( 'NONE',  ( 78.14518615778180788, 37.22968750108394431, -5.444914386472297529 ) ) ;
#4042 = DIRECTION ( 'NONE',  ( 0.000000000000000000, -1.000000000000000000, 0.000000000000000000 ) ) ;
#4043 = CIRCLE ( 'NONE', #10389, 5.000000000000004441 ) ;
#4044 = CIRCLE ( 'NONE', #28108, 1.000000000000000888 ) ;
#4045 = CARTESIAN_POINT ( 'NONE',  ( 94.99999999999995737, 1.387778780781445676E-14, 34.79898987322334136 ) ) ;
#4046 = ORIENTED_EDGE ( 'NONE', *, *, #14668, .F. ) ;
#4047 = CARTESIAN_POINT ( 'NONE',  ( 93.00000000000001421, 107.7255621263696668, -51.89999999999999858 ) ) ;
#4048 = CARTESIAN_POINT ( 'NONE',  ( -1.505492181556997933, 53.60078691996342570, -14.99999999999999645 ) ) ;
#4049 = VECTOR ( 'NONE', #16493, 1000.000000000000000 ) ;
#4050 = CARTESIAN_POINT ( 'NONE',  ( 102.0710678118654755, 92.68749999726881583, 4.999999999999961808 ) ) ;
#4051 = CARTESIAN_POINT ( 'NONE',  ( 143.5748159460630688, 34.35234375216787583, -1.662435489736055892E-15 ) ) ;
#4052 = FACE_OUTER_BOUND ( 'NONE', #786, .T. ) ;
#4053 = CARTESIAN_POINT ( 'NONE',  ( 2.493653234604083739E-15, 34.94765625216787441, 13.57481594606304576 ) ) ;
#4054 = CARTESIAN_POINT ( 'NONE',  ( 195.0000000000000000, 35.39414062608393863, 13.14518615778179544 ) ) ;
#4055 = ORIENTED_EDGE ( 'NONE', *, *, #24116, .T. ) ;
#4056 = ORIENTED_EDGE ( 'NONE', *, *, #1334, .T. ) ;
#4057 = CARTESIAN_POINT ( 'NONE',  ( -13.14518615778179544, 38.37070312608393152, 0.000000000000000000 ) ) ;
#4058 = CARTESIAN_POINT ( 'NONE',  ( 95.54126587499996504, 1.387778780781445676E-14, 14.68750000136559208 ) ) ;
#4059 = CARTESIAN_POINT ( 'NONE',  ( 70.44491438647229131, 40.00781250108393294, 13.14518615778179189 ) ) ;
#4060 = CARTESIAN_POINT ( 'NONE',  ( 101.8468681455907046, 80.75000000136560629, 4.458734124999987891 ) ) ;
#4061 = DIRECTION ( 'NONE',  ( -1.000000000000000000, 0.000000000000000000, 7.228014483236696740E-18 ) ) ;
#4062 = CARTESIAN_POINT ( 'NONE',  ( 99.99999999999998579, 90.00000000000000000, -6.938893903907228378E-15 ) ) ;
#4063 = CARTESIAN_POINT ( 'NONE',  ( 99.99999999999998579, 89.99899999999999523, -9.540979117872439019E-15 ) ) ;
#4064 =( GEOMETRIC_REPRESENTATION_CONTEXT ( 3 ) GLOBAL_UNCERTAINTY_ASSIGNED_CONTEXT ( ( #8332 ) ) GLOBAL_UNIT_ASSIGNED_CONTEXT ( ( #17603, #22887, #1232 ) ) REPRESENTATION_CONTEXT ( 'NONE', 'WORKASPACE' ) );
#4065 = CYLINDRICAL_SURFACE ( 'NONE', #12103, 5.000000000000004441 ) ;
#4066 = MECHANICAL_DESIGN_GEOMETRIC_PRESENTATION_REPRESENTATION (  '', ( #1354 ), #14062 ) ;
#4067 = CARTESIAN_POINT ( 'NONE',  ( 181.8548138422182205, 40.00781250108393294, 5.444914386472304635 ) ) ;
#4068 = CARTESIAN_POINT ( 'NONE',  ( 137.1713912169990124, 31.99955315621561525, -11.52591757658528948 ) ) ;
#4069 = ORIENTED_EDGE ( 'NONE', *, *, #16974, .F. ) ;
#4070 = CARTESIAN_POINT ( 'NONE',  ( 2.493653234604083739E-15, 38.81718749999999574, 13.57481594606304576 ) ) ;
#4071 = CARTESIAN_POINT ( 'NONE',  ( 13.14518615778179900, 40.20625000108393010, -5.444914386472297529 ) ) ;
#4072 = CARTESIAN_POINT ( 'NONE',  ( 103.5355339059327093, -3.535533905932726206, 1.500000002731184612 ) ) ;
#4073 = CARTESIAN_POINT ( 'NONE',  ( 130.0000000000000000, 36.18789062608393436, 13.14518615778179544 ) ) ;
#4074 = CARTESIAN_POINT ( 'NONE',  ( 74.29505027212704249, 36.28710937608393294, -9.295050272127046043 ) ) ;
#4075 = CARTESIAN_POINT ( 'NONE',  ( 181.8548138422181921, 31.87187500108393223, 5.444914386472304635 ) ) ;
#4076 = ADVANCED_FACE ( 'NONE', ( #19380 ), #25794, .T. ) ;
#4077 = CARTESIAN_POINT ( 'NONE',  ( 65.00000000000000000, 52.00000000000000711, 11.57481594606303688 ) ) ;
#4078 = CARTESIAN_POINT ( 'NONE',  ( -5.444914386472297529, 34.84843750108393579, -13.14518615778179900 ) ) ;
#4079 = DIRECTION ( 'NONE',  ( -1.000000000000000000, 0.000000000000000000, 0.000000000000000000 ) ) ;
#4080 = CARTESIAN_POINT ( 'NONE',  ( -13.57481594606304753, 38.66835937716787441, -5.622872871577872189 ) ) ;
#4081 = CYLINDRICAL_SURFACE ( 'NONE', #8078, 13.57481594606304576 ) ;
#4082 = CARTESIAN_POINT ( 'NONE',  ( 5.444914386472297529, 39.51171875108392584, -13.14518615778179900 ) ) ;
#4083 = DIRECTION ( 'NONE',  ( 1.000000000000000000, 1.387778780781445478E-15, 0.000000000000000000 ) ) ;
#4084 = CARTESIAN_POINT ( 'NONE',  ( 98.23223304703363112, 123.4000000021849530, -1.767766952966370209 ) ) ;
#4085 = CARTESIAN_POINT ( 'NONE',  ( 60.93741645942577634, 50.00000000116062182, 12.98908657125237376 ) ) ;
#4086 = LINE ( 'NONE', #5946, #14603 ) ;
#4087 = CARTESIAN_POINT ( 'NONE',  ( 101.8468681455906903, -4.458734124999987891, 8.750000001365592084 ) ) ;
#4088 = CARTESIAN_POINT ( 'NONE',  ( 95.67376207875072680, 104.0454443415356991, -48.20000000546237118 ) ) ;
#4089 = CARTESIAN_POINT ( 'NONE',  ( 97.50000000000000000, 123.5500000021849587, 1.035533905932725096 ) ) ;
#4090 = CARTESIAN_POINT ( 'NONE',  ( 95.54126587499996504, 1.387778780781445676E-14, 10.43750000136559208 ) ) ;
#4091 = CARTESIAN_POINT ( 'NONE',  ( -5.444914386472297529, 32.46718750108393436, -13.14518615778179722 ) ) ;
#4092 = B_SPLINE_CURVE_WITH_KNOTS ( 'NONE', 3,
 ( #22896, #18879, #1240, #8190, #1515, #12582, #7778, #27730, #27451, #5788, #25445, #14593, #17012, #23312, #9903, #3784, #25716, #23035, #14728, #10039, #16745, #5926, #1649, #14455, #21168, #7912, #20755, #16465, #12442, #10309, #19016 ),
 .UNSPECIFIED., .F., .F.,
 ( 4, 2, 2, 2, 2, 2, 2, 2, 2, 2, 1, 2, 2, 2, 2, 4 ),
 ( 0.000000000000000000, 0.001647793485000534136, 0.003295586970001068271, 0.004943380455001602190, 0.005767277197501870234, 0.006591173940002139145, 0.008238967425002673498, 0.009886760910003206115, 0.01318234788000428176, 0.01483014136500482132, 0.01647793485000536087, 0.01812572833500590216, 0.01977352182000643999, 0.02306910879000751910, 0.02471690227500805692, 0.02636469576000859821 ),
 .UNSPECIFIED. ) ;
#4093 = AXIS2_PLACEMENT_3D ( 'NONE', #23003, #8022, #18584 ) ;
#4094 = CARTESIAN_POINT ( 'NONE',  ( -13.14518615778179544, 38.96601562608393721, 0.000000000000000000 ) ) ;
#4095 = DIRECTION ( 'NONE',  ( 5.782411586589358625E-17, -0.000000000000000000, 1.000000000000000000 ) ) ;
#4096 = CARTESIAN_POINT ( 'NONE',  ( 95.54126587499996504, 83.68750000136560629, -1.387778780781445676E-14 ) ) ;
#4097 = CARTESIAN_POINT ( 'NONE',  ( 78.14518615778179367, 39.56132812608393579, -1.609821015232357215E-15 ) ) ;
#4098 = CARTESIAN_POINT ( 'NONE',  ( 91.91746824999999887, 110.0000000000000000, -51.12500000273119127 ) ) ;
#4099 = CARTESIAN_POINT ( 'NONE',  ( 13.14518615778179722, 40.20625000108393010, -5.444914386472297529 ) ) ;
#4100 = CARTESIAN_POINT ( 'NONE',  ( 0.000000000000000000, 36.00000000000000000, 0.000000000000000000 ) ) ;
#4101 = CARTESIAN_POINT ( 'NONE',  ( -5.622872871577767384, 40.85117187499999147, -13.57481594606315412 ) ) ;
#4102 = CARTESIAN_POINT ( 'NONE',  ( 93.00000000000000000, 107.7255621263696526, -50.39999999453763024 ) ) ;
#4103 = CARTESIAN_POINT ( 'NONE',  ( 130.0000000000000000, 40.00781250000000000, -13.57481594606304576 ) ) ;
#4104 = ORIENTED_EDGE ( 'NONE', *, *, #12527, .F. ) ;
#4105 = CARTESIAN_POINT ( 'NONE',  ( 1.662435489736055498E-15, -7.395377635281828788, -13.57481594606304398 ) ) ;
#4106 = CARTESIAN_POINT ( 'NONE',  ( 9.295050272127047819, 39.46210937608393721, 9.295050272127046043 ) ) ;
#4107 = CARTESIAN_POINT ( 'NONE',  ( -13.57481594606304576, 39.51171875216787299, 0.000000000000000000 ) ) ;
#4108 = CARTESIAN_POINT ( 'NONE',  ( 124.5550856135277087, 36.73359375108393010, 13.14518615778179722 ) ) ;
#4109 = EDGE_CURVE ( 'NONE', #15719, #3050, #14153, .T. ) ;
#4110 = CARTESIAN_POINT ( 'NONE',  ( 51.42518405393695957, 37.13046875216787868, 0.000000000000000000 ) ) ;
#4111 = CARTESIAN_POINT ( 'NONE',  ( 97.50236033167490746, 102.3130555110000159, -53.22499999726882436 ) ) ;
#4112 = CARTESIAN_POINT ( 'NONE',  ( -9.598844408820454532, 37.22968750216787726, 9.598844408820459861 ) ) ;
#4113 = EDGE_CURVE ( 'NONE', #9852, #16430, #11364, .T. ) ;
#4114 = CARTESIAN_POINT ( 'NONE',  ( 99.99999999999995737, 5.000000000000018652, 3.750000000000000000 ) ) ;
#4115 = CARTESIAN_POINT ( 'NONE',  ( 105.6631189606246295, 114.1144967660473242, -47.30000000546237260 ) ) ;
#4116 = CARTESIAN_POINT ( 'NONE',  ( 200.4449143864723055, 36.83281250108392868, 13.14518615778179189 ) ) ;
#4117 = CARTESIAN_POINT ( 'NONE',  ( -8.312177448680279460E-16, 38.42031249999999432, -13.57481594606304576 ) ) ;
#4118 = ADVANCED_FACE ( 'NONE', ( #23667 ), #25775, .F. ) ;
#4119 = CARTESIAN_POINT ( 'NONE',  ( 135.4449143864723339, 39.51171875108393294, -13.14518615778179722 ) ) ;
#4120 = CARTESIAN_POINT ( 'NONE',  ( 97.50000000000000000, 122.6500000021849530, -1.035533905932742416 ) ) ;
#4121 = DIRECTION ( 'NONE',  ( -0.000000000000000000, -0.000000000000000000, 1.000000000000000000 ) ) ;
#4122 = DIRECTION ( 'NONE',  ( 0.000000000000000000, -1.000000000000000000, 0.000000000000000000 ) ) ;
#4123 = CARTESIAN_POINT ( 'NONE',  ( 102.1631189606246295, 103.3426043859339103, -48.40000000000001279 ) ) ;
#4124 = CARTESIAN_POINT ( 'NONE',  ( 9.295050272127047819, 37.87460937608393863, 9.295050272127046043 ) ) ;
#4125 = CARTESIAN_POINT ( 'NONE',  ( 13.14518615778179900, 38.51953125108393294, 5.444914386472293977 ) ) ;
#4126 = CARTESIAN_POINT ( 'NONE',  ( 181.4251840539369596, 37.82499999999999574, 0.000000000000000000 ) ) ;
#4127 = CARTESIAN_POINT ( 'NONE',  ( 13.57481594606304576, 35.84062499999999574, -1.662435489736055892E-15 ) ) ;
#4128 = CARTESIAN_POINT ( 'NONE',  ( 96.84719886470459471, -3.152801135295355994, 3.812500001365591640 ) ) ;
#4129 = CARTESIAN_POINT ( 'NONE',  ( 59.55508561352770158, 37.52734375108393294, 13.14518615778179722 ) ) ;
#4130 = AXIS2_PLACEMENT_3D ( 'NONE', #7589, #9998, #9866 ) ;
#4131 = CARTESIAN_POINT ( 'NONE',  ( 104.4587341249999781, -1.846868145590721655, 5.875000001365592084 ) ) ;
#4132 = FACE_OUTER_BOUND ( 'NONE', #19605, .T. ) ;
#4133 = CARTESIAN_POINT ( 'NONE',  ( 104.4587341249999923, 94.24999999863439371, 1.846868145590726318 ) ) ;
#4134 = CYLINDRICAL_SURFACE ( 'NONE', #9349, 5.000000000000004441 ) ;
#4135 = CARTESIAN_POINT ( 'NONE',  ( -8.312177448680279460E-16, 40.80156249999999574, -13.57481594606304576 ) ) ;
#4136 = CARTESIAN_POINT ( 'NONE',  ( 135.4449143864723055, 40.20625000108394431, 13.14518615778179189 ) ) ;
#4137 = ORIENTED_EDGE ( 'NONE', *, *, #26047, .T. ) ;
#4138 = CARTESIAN_POINT ( 'NONE',  ( 96.46446609406721961, 84.87500000000000000, -3.535533905932755072 ) ) ;
#4139 =( GEOMETRIC_REPRESENTATION_CONTEXT ( 3 ) GLOBAL_UNCERTAINTY_ASSIGNED_CONTEXT ( ( #155 ) ) GLOBAL_UNIT_ASSIGNED_CONTEXT ( ( #20072, #13771, #2823 ) ) REPRESENTATION_CONTEXT ( 'NONE', 'WORKASPACE' ) );
#4140 = CARTESIAN_POINT ( 'NONE',  ( 95.54126587500000767, 90.81249999863440792, -7.484931351350258973E-15 ) ) ;
#4141 = VERTEX_POINT ( 'NONE', #1427 ) ;
#4142 = DIRECTION ( 'NONE',  ( 0.000000000000000000, -1.000000000000000000, -0.000000000000000000 ) ) ;
#4143 = CARTESIAN_POINT ( 'NONE',  ( 55.70494972787295751, 36.08867187608393579, 9.295050272127047819 ) ) ;
#4144 =( BOUNDED_CURVE ( )  B_SPLINE_CURVE ( 2, ( #10791, #21092, #14651, #17216, #6526, #25776, #1581, #6255, #10653 ),
 .UNSPECIFIED., .F., .T. ) 
 B_SPLINE_CURVE_WITH_KNOTS ( ( 3, 2, 2, 2, 3 ),
 ( 0.3958333333333331483, 0.4062499999999999445, 0.4166666666666667407, 0.4270833333333335369, 0.4375000000000003331 ),
 .UNSPECIFIED. ) 
 CURVE ( )  GEOMETRIC_REPRESENTATION_ITEM ( )  RATIONAL_B_SPLINE_CURVE ( ( 1.000000000000001110, 0.9238795325112855172, 1.000000000000000000, 0.9238795325112867385, 1.000000000000000000, 0.9238795325112867385, 1.000000000000000000, 0.9238795325112842960, 1.000000000000002442 ) ) 
 REPRESENTATION_ITEM ( '' )  );
#4145 = VERTEX_POINT ( 'NONE', #10085 ) ;
#4146 = CARTESIAN_POINT ( 'NONE',  ( 13.57481594606304931, 32.61601562499999574, 5.622872871577868636 ) ) ;
#4147 = EDGE_CURVE ( 'NONE', #11554, #25472, #19069, .T. ) ;
#4148 = AXIS2_PLACEMENT_3D ( 'NONE', #21012, #3482, #12146 ) ;
#4149 = CARTESIAN_POINT ( 'NONE',  ( 101.8468681455906903, 4.458734125000016313, 2.375000001365592084 ) ) ;
#4150 = ORIENTED_EDGE ( 'NONE', *, *, #23532, .T. ) ;
#4151 = CARTESIAN_POINT ( 'NONE',  ( 13.14518615778179722, 35.54296875108394715, 5.444914386472293977 ) ) ;
#4152 = CARTESIAN_POINT ( 'NONE',  ( -13.14518615778179900, 38.32109375108394289, -5.444914386472297529 ) ) ;
#4153 = CARTESIAN_POINT ( 'NONE',  ( 181.4251840539369596, 36.28710937716787299, -5.622872871577873077 ) ) ;
#4154 = CARTESIAN_POINT ( 'NONE',  ( 2.414731522848535132E-15, 37.57695312608392868, 13.14518615778179544 ) ) ;
#4155 = DIRECTION ( 'NONE',  ( 0.000000000000000000, -0.000000000000000000, 1.000000000000000000 ) ) ;
#4156 = CARTESIAN_POINT ( 'NONE',  ( 93.00000000000000000, 110.0000000000000000, -52.00000000000000711 ) ) ;
#4157 = CARTESIAN_POINT ( 'NONE',  ( 130.0000000000000000, 38.56914062608393579, 13.14518615778179544 ) ) ;
#4158 = CARTESIAN_POINT ( 'NONE',  ( 9.295050272127047819, 39.46210937608393721, 9.295050272127046043 ) ) ;
#4159 = VECTOR ( 'NONE', #12298, 1000.000000000000000 ) ;
#4160 = CARTESIAN_POINT ( 'NONE',  ( 130.0000000000000000, 34.40195312608393152, 13.14518615778179544 ) ) ;
#4161 = CARTESIAN_POINT ( 'NONE',  ( 74.59884440882045453, 36.73359374999999716, -9.598844408820458085 ) ) ;
#4162 = CARTESIAN_POINT ( 'NONE',  ( 97.92893218813451028, 5.000000000000018652, 9.812499999999998224 ) ) ;
#4163 = CARTESIAN_POINT ( 'NONE',  ( 101.8468681455906903, -4.458734124999987891, 2.750000001365592084 ) ) ;
#4164 = CARTESIAN_POINT ( 'NONE',  ( 2.493653234604083739E-15, 34.84843749999999574, 13.57481594606304576 ) ) ;
#4165 = CARTESIAN_POINT ( 'NONE',  ( 98.15313185440925281, -4.458734124999987891, 5.625000001365591196 ) ) ;
#4166 = CARTESIAN_POINT ( 'NONE',  ( 99.99999999999998579, 118.4984768113314004, -53.62500000273119127 ) ) ;
#4167 = CARTESIAN_POINT ( 'NONE',  ( 87.00000000000000000, 123.0000000000000000, -13.00000000000000888 ) ) ;
#4168 = CYLINDRICAL_SURFACE ( 'NONE', #26722, 13.57481594606304576 ) ;
#4169 = CARTESIAN_POINT ( 'NONE',  ( -9.295050272127046043, 33.31054687608393294, -9.295050272127046043 ) ) ;
#4170 = CARTESIAN_POINT ( 'NONE',  ( 13.14518615778179544, 40.35507812608393863, -1.609821015232357215E-15 ) ) ;
#4171 = CARTESIAN_POINT ( 'NONE',  ( 95.00472066334982912, 116.8754121666685393, -46.17499999726882720 ) ) ;
#4172 = VERTEX_POINT ( 'NONE', #8235 ) ;
#4173 = CARTESIAN_POINT ( 'NONE',  ( 0.000000000000000000, 36.00000000000000000, 0.000000000000000000 ) ) ;
#4174 = CARTESIAN_POINT ( 'NONE',  ( -13.09590655363597733, 36.00000000000000000, 1.137167824541468031 ) ) ;
#4175 = CARTESIAN_POINT ( 'NONE',  ( 100.1069863019943114, 123.0000000000000000, -2.169275729499147598 ) ) ;
#4176 = CARTESIAN_POINT ( 'NONE',  ( 185.7049497278729575, 38.86679687608393863, -9.295050272127046043 ) ) ;
#4177 = EDGE_LOOP ( 'NONE', ( #21455, #8984, #5874, #7678 ) ) ;
#4178 = CARTESIAN_POINT ( 'NONE',  ( 142.0772764098356333, 36.00000000000000711, -6.197985357349214297 ) ) ;
#4179 = CARTESIAN_POINT ( 'NONE',  ( 105.6631189606246295, 105.8855032339526758, -54.20000000000000995 ) ) ;
#4180 = CARTESIAN_POINT ( 'NONE',  ( 84.99999999999998579, 120.0000000000000000, -45.00000000000000711 ) ) ;
#4181 = ORIENTED_EDGE ( 'NONE', *, *, #4147, .F. ) ;
#4182 = CARTESIAN_POINT ( 'NONE',  ( 95.67376207875072680, 104.0454443415356991, -47.70000000000000995 ) ) ;
#4183 = CARTESIAN_POINT ( 'NONE',  ( -8.312177448680279460E-16, 33.75703125216787726, -13.57481594606304576 ) ) ;
#4184 = CARTESIAN_POINT ( 'NONE',  ( 102.0669872999999939, 123.5000000010924595, 0.8561741729129311862 ) ) ;
#4185 = CARTESIAN_POINT ( 'NONE',  ( 135.6228728715778686, 34.50117187716788436, -13.57481594606304753 ) ) ;
#4186 = CARTESIAN_POINT ( 'NONE',  ( 102.1631189606246295, 103.3426043859339103, -43.90000000546237402 ) ) ;
#4187 = CARTESIAN_POINT ( 'NONE',  ( -5.622872871577782483, 34.60039062716787583, -13.57481594606313990 ) ) ;
#4188 = CARTESIAN_POINT ( 'NONE',  ( 181.8548138422182205, 35.98945312608393721, 0.000000000000000000 ) ) ;
#4189 = ORIENTED_EDGE ( 'NONE', *, *, #3756, .F. ) ;
#4190 = ADVANCED_FACE ( 'NONE', ( #16926 ), #14774, .T. ) ;
#4191 =( BOUNDED_CURVE ( )  B_SPLINE_CURVE ( 2, ( #8750, #2354, #26140, #23863, #21590, #15291, #19445, #352, #24008, #11009, #19722, #17731, #6199, #14869, #23583, #4067, #12729, #21453, #1931, #10599, #19307, #8471, #17158, #24285, #20446, #13428, #13719, #14004, #927, #24717, #16149, #3053, #9312, #24857, #22156, #20158, #9739, #6892, #17871, #7166, #4766, #9598, #11720, #15863, #24573, #13575, #26433, #9178, #26576, #639, #18300, #22727, #26720, #2634, #11864, #7455, #3193, #2774, #9454, #7025, #2908, #5195, #11577, #18010, #15723, #5054, #24426, #20587, #22299, #26868, #7314, #22441, #20297, #27008, #784, #5338, #18154, #4915, #16003, #13859, #1070, #15578, #22585, #11294, #20017, #497, #11438, #5477, #25555, #14427, #18992, #27290, #16856, #16434, #20865, #3334, #27701 ),
 .UNSPECIFIED., .F., .T. ) 
 B_SPLINE_CURVE_WITH_KNOTS ( ( 3, 2, 2, 2, 2, 2, 2, 2, 2, 2, 2, 2, 2, 2, 2, 2, 2, 2, 2, 2, 2, 2, 2, 2, 2, 2, 2, 2, 2, 2, 2, 2, 2, 2, 2, 2, 2, 2, 2, 2, 2, 2, 2, 2, 2, 2, 2, 2, 3 ),
 ( 0.000000000000000000, 0.01041666666666666609, 0.02083333333333333218, 0.03125000000000000000, 0.04166666666666666435, 0.05208333333333333565, 0.06250000000000000000, 0.07291666666666667129, 0.08333333333333332871, 0.09374999999999998612, 0.1041666666666666713, 0.1145833333333333287, 0.1250000000000000000, 0.1354166666666666574, 0.1458333333333333426, 0.1562500000000000000, 0.1666666666666666574, 0.1770833333333333426, 0.1874999999999999722, 0.1979166666666666574, 0.2083333333333333426, 0.2187500000000000000, 0.2291666666666666574, 0.2395833333333333426, 0.2500000000000000000, 0.2604166666666666852, 0.2708333333333333148, 0.2812500000000000000, 0.2916666666666666852, 0.3020833333333333148, 0.3125000000000000000, 0.3229166666666666852, 0.3333333333333333148, 0.3437500000000000000, 0.3541666666666666852, 0.3645833333333333148, 0.3749999999999999445, 0.3854166666666666852, 0.3958333333333333148, 0.4062500000000000000, 0.4166666666666666852, 0.4270833333333333148, 0.4375000000000000000, 0.4479166666666666852, 0.4583333333333333148, 0.4687500000000000000, 0.4791666666666666852, 0.4895833333333333148, 0.4988304892921909817 ),
 .UNSPECIFIED. ) 
 CURVE ( )  GEOMETRIC_REPRESENTATION_ITEM ( )  RATIONAL_B_SPLINE_CURVE ( ( 1.000000000000000000, 0.9238795325112867385, 1.000000000000000000, 0.9238795325112867385, 1.000000000000000000, 0.9238795325112867385, 1.000000000000000000, 0.9238795325112867385, 1.000000000000000000, 0.9238795325112867385, 1.000000000000000000, 0.9238795325112867385, 1.000000000000000000, 0.9238795325112867385, 1.000000000000000000, 0.9238795325112867385, 1.000000000000000000, 0.9238795325112867385, 1.000000000000000000, 0.9238795325112867385, 1.000000000000000000, 0.9238795325112867385, 1.000000000000000000, 0.9238795325112867385, 1.000000000000000000, 0.9238795325112867385, 1.000000000000000000, 0.9238795325112867385, 1.000000000000000000, 0.9238795325112867385, 1.000000000000000000, 0.9238795325112867385, 1.000000000000000000, 0.9238795325112867385, 1.000000000000000000, 0.9238795325112867385, 1.000000000000000000, 0.9238795325112867385, 1.000000000000000000, 0.9238795325112867385, 1.000000000000000000, 0.9238795325112867385, 1.000000000000000000, 0.9238795325112867385, 1.000000000000000000, 0.9238795325112867385, 1.000000000000000000, 0.9238795325112867385, 1.000000000000000000, 0.9238795325112867385, 1.000000000000000000, 0.9238795325112867385, 1.000000000000000000, 0.9238795325112867385, 1.000000000000000000, 0.9238795325112867385, 1.000000000000000000, 0.9238795325112867385, 1.000000000000000000, 0.9238795325112867385, 1.000000000000000000, 0.9238795325112867385, 1.000000000000000000, 0.9238795325112867385, 1.000000000000000000, 0.9238795325112867385, 1.000000000000000000, 0.9238795325112867385, 1.000000000000000000, 0.9238795325112867385, 1.000000000000000000, 0.9238795325112867385, 1.000000000000000000, 0.9238795325112867385, 1.000000000000000000, 0.9238795325112867385, 1.000000000000000000, 0.9238795325112867385, 1.000000000000000000, 0.9238795325112867385, 1.000000000000000000, 0.9238795325112867385, 1.000000000000000000, 0.9238795325112867385, 1.000000000000000000, 0.9238795325112867385, 1.000000000000000000, 0.9238795325112867385, 1.000000000000000000, 0.9238795325112867385, 1.000000000000000000, 0.9238795325112867385, 1.000000000000000000, 0.9238795325112867385, 1.000000000000000000, 0.9324258078851886955, 0.9848264816800353927 ) ) 
 REPRESENTATION_ITEM ( '' )  );
#4192 = ORIENTED_EDGE ( 'NONE', *, *, #16531, .F. ) ;
#4193 = ORIENTED_EDGE ( 'NONE', *, *, #10447, .F. ) ;
#4194 = CARTESIAN_POINT ( 'NONE',  ( 5.444914386472297529, 38.12265625108393152, -13.14518615778179900 ) ) ;
#4195 = CARTESIAN_POINT ( 'NONE',  ( 97.92893218813451028, 83.81250000000001421, -5.000000000000031974 ) ) ;
#4196 = CARTESIAN_POINT ( 'NONE',  ( 99.99999999999998579, 124.3999999999999915, 2.499999999999978684 ) ) ;
#4197 = CARTESIAN_POINT ( 'NONE',  ( 101.8468681455907046, 81.75000000136560629, 4.458734124999987891 ) ) ;
#4198 = CARTESIAN_POINT ( 'NONE',  ( 185.7049497278729575, 37.47773437608393010, 9.295050272127047819 ) ) ;
#4199 = CARTESIAN_POINT ( 'NONE',  ( 107.0000000000000142, 110.0000000000000000, -53.00000000000000711 ) ) ;
#4200 = CARTESIAN_POINT ( 'NONE',  ( 84.99999999999998579, 123.0000000000000000, -13.00000000000000888 ) ) ;
#4201 = PLANE ( 'NONE',  #22590 ) ;
#4202 = CARTESIAN_POINT ( 'NONE',  ( 94.33688103937537051, 105.8855032339526758, -49.80000000000000426 ) ) ;
#4203 = CARTESIAN_POINT ( 'NONE',  ( 130.0000000000000000, 32.46718749999999432, 13.57481594606304576 ) ) ;
#4204 = EDGE_LOOP ( 'NONE', ( #24878, #14436, #9981, #9822 ) ) ;
#4205 = CARTESIAN_POINT ( 'NONE',  ( -9.598844408820454532, 37.13046874999999147, 9.598844408820459861 ) ) ;
#4206 = CARTESIAN_POINT ( 'NONE',  ( 2.414731522848535132E-15, 35.98945312608393010, 13.14518615778179544 ) ) ;
#4207 = CARTESIAN_POINT ( 'NONE',  ( 96.46446609406721961, 3.535533905932755072, 3.000000002731185944 ) ) ;
#4208 = CARTESIAN_POINT ( 'NONE',  ( 116.8548138422182063, 35.14609375108393152, -5.444914386472297529 ) ) ;
#4209 = CARTESIAN_POINT ( 'NONE',  ( 51.85481384221820633, 34.99726562608393721, 0.000000000000000000 ) ) ;
#4210 = AXIS2_PLACEMENT_3D ( 'NONE', #3842, #12373, #9966 ) ;
#4211 = CARTESIAN_POINT ( 'NONE',  ( 189.5550856135277229, 36.13828125108393863, 13.14518615778179722 ) ) ;
#4212 = ORIENTED_EDGE ( 'NONE', *, *, #16018, .F. ) ;
#4213 = CARTESIAN_POINT ( 'NONE',  ( 93.00000000000000000, 110.0000000000000000, -46.50000000546238255 ) ) ;
#4214 = CARTESIAN_POINT ( 'NONE',  ( 13.14518615778179900, 34.65000000108393152, -5.444914386472297529 ) ) ;
#4215 = CARTESIAN_POINT ( 'NONE',  ( 133.7165341137897201, 51.46663580899082291, -14.99999999999932143 ) ) ;
#4216 = CARTESIAN_POINT ( 'NONE',  ( -5.622872871578011633, 38.86679687716787868, 13.57481594606290720 ) ) ;
#4217 = CARTESIAN_POINT ( 'NONE',  ( 99.99999999999998579, 138.0000000000000000, -5.204170427930421283E-15 ) ) ;
#4218 = CARTESIAN_POINT ( 'NONE',  ( -13.14518615778179189, 38.22187500108393010, 5.444914386472304635 ) ) ;
#4219 = DIRECTION ( 'NONE',  ( -1.000000000000000000, 0.000000000000000000, 5.782411586589357392E-17 ) ) ;
#4220 = CARTESIAN_POINT ( 'NONE',  ( 101.0355339059327378, 122.9500000021849502, 2.499999999999977796 ) ) ;
#4221 = LINE ( 'NONE', #26307, #21882 ) ;
#4222 = SURFACE_SIDE_STYLE ('',( #8212 ) ) ;
#4223 = CARTESIAN_POINT ( 'NONE',  ( 96.84719886470459471, 3.152801135295383084, 7.312500001365592084 ) ) ;
#4224 = CARTESIAN_POINT ( 'NONE',  ( 77.32011696698889125, 36.00000000000002132, -5.704949255836485378 ) ) ;
#4225 = ORIENTED_EDGE ( 'NONE', *, *, #5130, .T. ) ;
#4226 = CARTESIAN_POINT ( 'NONE',  ( 92.99999999999998579, 110.0000000000000000, -50.49999999453763877 ) ) ;
#4227 = CARTESIAN_POINT ( 'NONE',  ( 96.84719886470459471, 3.152801135295383084, 13.31250000136559386 ) ) ;
#4228 = CARTESIAN_POINT ( 'NONE',  ( 121.7314026716134379, 50.00000000054362914, 10.78867689284450826 ) ) ;
#4229 = VECTOR ( 'NONE', #1619, 1000.000000000000000 ) ;
#4230 = CARTESIAN_POINT ( 'NONE',  ( 13.14518615778179900, 37.72578125108393721, 5.444914386472293977 ) ) ;
#4231 = CARTESIAN_POINT ( 'NONE',  ( 181.6399989480775901, 40.87597656304196647, 0.000000000000000000 ) ) ;
#4232 = CARTESIAN_POINT ( 'NONE',  ( 103.1528011352953342, 82.31250000136559208, -3.152801135295383084 ) ) ;
#4233 = CARTESIAN_POINT ( 'NONE',  ( 65.00000000000000000, 34.60039062608393579, 13.14518615778179544 ) ) ;
#4234 = CARTESIAN_POINT ( 'NONE',  ( 106.5389055433251002, 105.2492070361643215, -50.32500000273120122 ) ) ;
#4235 = CARTESIAN_POINT ( 'NONE',  ( 185.8198241863519797, 50.00000000000000000, -9.999999999999991118 ) ) ;
#4236 = DIRECTION ( 'NONE',  ( 0.000000000000000000, 0.000000000000000000, 1.000000000000000000 ) ) ;
#4237 = CARTESIAN_POINT ( 'NONE',  ( 97.92893218813451028, -4.999999999999989342, 11.31250000273118772 ) ) ;
#4238 = CARTESIAN_POINT ( 'NONE',  ( 102.0710678118654329, 82.68750000000000000, -4.999999999999992006 ) ) ;
#4239 = CARTESIAN_POINT ( 'NONE',  ( 143.5748159460630404, 39.85898437499999858, -5.622872871577873077 ) ) ;
#4240 = ORIENTED_EDGE ( 'NONE', *, *, #11098, .F. ) ;
#4241 = DIRECTION ( 'NONE',  ( 0.000000000000000000, 0.000000000000000000, -1.000000000000000000 ) ) ;
#4242 = CARTESIAN_POINT ( 'NONE',  ( 9.295050272127046043, 36.48554687608393721, -9.295050272127046043 ) ) ;
#4243 = CARTESIAN_POINT ( 'NONE',  ( -5.622872871577873077, 36.48554687716787015, 13.57481594606304753 ) ) ;
#4244 = CARTESIAN_POINT ( 'NONE',  ( 139.2950502721270425, 35.29492187608393294, 9.295050272127046043 ) ) ;
#4245 = CARTESIAN_POINT ( 'NONE',  ( 78.57481594606305464, 37.52734375216787299, -1.662435489736055892E-15 ) ) ;
#4246 = CARTESIAN_POINT ( 'NONE',  ( 0.000000000000000000, 10.00000000000000178, 0.000000000000000000 ) ) ;
#4247 = CARTESIAN_POINT ( 'NONE',  ( -5.622872871577873077, 36.18789062716787441, -13.57481594606304753 ) ) ;
#4248 = AXIS2_PLACEMENT_3D ( 'NONE', #23430, #3486, #1362 ) ;
#4249 = CARTESIAN_POINT ( 'NONE',  ( 104.9999999999999574, -2.071067811865462627, 4.437500000000000000 ) ) ;
#4250 = ORIENTED_EDGE ( 'NONE', *, *, #22553, .F. ) ;
#4251 = EDGE_CURVE ( 'NONE', #8417, #27733, #21046, .T. ) ;
#4252 = CARTESIAN_POINT ( 'NONE',  ( 185.7049497278729575, 38.07304687608393579, -9.295050272127046043 ) ) ;
#4253 = CARTESIAN_POINT ( 'NONE',  ( 78.57481594606305464, 39.01562500000000000, -1.662435489736055892E-15 ) ) ;
#4254 = EDGE_LOOP ( 'NONE', ( #472, #20433, #20283, #6177 ) ) ;
#4255 = DIRECTION ( 'NONE',  ( -0.000000000000000000, -1.000000000000000000, -0.000000000000000000 ) ) ;
#4256 = CARTESIAN_POINT ( 'NONE',  ( 102.1631189606246295, 103.3426043859339103, -47.89999999453763735 ) ) ;
#4257 = CARTESIAN_POINT ( 'NONE',  ( -9.598844408820454532, 36.33671874999999574, 9.598844408820459861 ) ) ;
#4258 = DIRECTION ( 'NONE',  ( -0.000000000000000000, 1.000000000000000000, -0.000000000000000000 ) ) ;
#4259 = CARTESIAN_POINT ( 'NONE',  ( 2.414731522848535132E-15, 36.18789062608393436, 13.14518615778179544 ) ) ;
#4260 = CARTESIAN_POINT ( 'NONE',  ( 101.0355339059327378, 123.1499999999999915, -2.499999999999997780 ) ) ;
#4261 = ADVANCED_FACE ( 'NONE', ( #6651 ), #28189, .T. ) ;
#4262 = CARTESIAN_POINT ( 'NONE',  ( 189.3771271284221314, 34.50117187499999005, -13.57481594606304753 ) ) ;
#4263 = CARTESIAN_POINT ( 'NONE',  ( 102.4976396683250925, 117.6869444889999841, -47.97500000273119269 ) ) ;
#4264 = CARTESIAN_POINT ( 'NONE',  ( 0.000000000000000000, 36.00000000000000000, 0.000000000000000000 ) ) ;
#4265 = CARTESIAN_POINT ( 'NONE',  ( 51.85481384221819923, 37.32890625108393579, -5.444914386472297529 ) ) ;
#4266 = EDGE_CURVE ( 'NONE', #19839, #18468, #23446, .T. ) ;
#4267 = CARTESIAN_POINT ( 'NONE',  ( 103.1528011352953342, 3.152801135295383084, 3.062500001365592528 ) ) ;
#4268 = PLANE ( 'NONE',  #13187 ) ;
#4269 = CARTESIAN_POINT ( 'NONE',  ( 96.84719886470463734, 94.93749999863440792, 3.152801135295351997 ) ) ;
#4270 = CARTESIAN_POINT ( 'NONE',  ( 102.4999999999999858, 123.8500000000000085, -1.035533905932742638 ) ) ;
#4271 = CARTESIAN_POINT ( 'NONE',  ( 13.57481594606304753, 35.89023437499999858, -5.622872871577873077 ) ) ;
#4272 = CARTESIAN_POINT ( 'NONE',  ( 102.1631189606246295, 103.3426043859339103, -45.40000000000001279 ) ) ;
#4273 = ADVANCED_FACE ( 'NONE', ( #17486 ), #21925, .T. ) ;
#4274 = ORIENTED_EDGE ( 'NONE', *, *, #24347, .T. ) ;
#4275 = CARTESIAN_POINT ( 'NONE',  ( 99.99999999999995737, 80.43750000136559208, -4.458734125000016313 ) ) ;
#4276 = VECTOR ( 'NONE', #3249, 1000.000000000000227 ) ;
#4277 = CARTESIAN_POINT ( 'NONE',  ( 98.15313185440925281, 94.62499999863439371, -4.458734124999994997 ) ) ;
#4278 = ORIENTED_EDGE ( 'NONE', *, *, #26223, .T. ) ;
#4279 = EDGE_CURVE ( 'NONE', #13199, #4566, #7028, .T. ) ;
#4280 = CARTESIAN_POINT ( 'NONE',  ( 97.83688103937535629, 116.6573956140660897, -49.40000000000001279 ) ) ;
#4281 = CARTESIAN_POINT ( 'NONE',  ( 51.85481384221819923, 33.55859375108393294, -5.444914386472297529 ) ) ;
#4282 = EDGE_LOOP ( 'NONE', ( #16873, #26377, #18015 ) ) ;
#4283 = CARTESIAN_POINT ( 'NONE',  ( 129.2802394038908176, 53.51499872091922327, -15.00000000000000000 ) ) ;
#4284 = CARTESIAN_POINT ( 'NONE',  ( 98.15313185440925281, 4.458734125000016313, 4.500000001365592084 ) ) ;
#4285 = ORIENTED_EDGE ( 'NONE', *, *, #4299, .F. ) ;
#4286 = CARTESIAN_POINT ( 'NONE',  ( 97.92893218813449607, 82.31250000273122680, 4.999999999999968914 ) ) ;
#4287 = CARTESIAN_POINT ( 'NONE',  ( -9.295050272127046043, 31.72304687608393081, -9.295050272127046043 ) ) ;
#4288 = CARTESIAN_POINT ( 'NONE',  ( 204.5988444088204687, 38.22187500216787015, 9.598844408820456309 ) ) ;
#4289 = CARTESIAN_POINT ( 'NONE',  ( 13.14518615778179722, 35.44375000108393436, -5.444914386472297529 ) ) ;
#4290 = CARTESIAN_POINT ( 'NONE',  ( 65.00000000000000000, 38.81718749999999574, 13.57481594606304576 ) ) ;
#4291 = CARTESIAN_POINT ( 'NONE',  ( 191.2834658862103936, 51.46663580899083001, 14.99999999999791989 ) ) ;
#4292 = EDGE_CURVE ( 'NONE', #3863, #13215, #24052, .T. ) ;
#4293 = CARTESIAN_POINT ( 'NONE',  ( 208.5748159460630688, 39.85898437716787157, 5.622872871577868636 ) ) ;
#4294 = VERTEX_POINT ( 'NONE', #24332 ) ;
#4295 = CARTESIAN_POINT ( 'NONE',  ( -13.14518615778179544, 36.78320312608393294, 0.000000000000000000 ) ) ;
#4296 = CARTESIAN_POINT ( 'NONE',  ( 116.8548138422182063, 35.04687500108393294, 5.444914386472304635 ) ) ;
#4297 = CARTESIAN_POINT ( 'NONE',  ( 65.00000000000000000, 35.24531249999999716, -13.57481594606304576 ) ) ;
#4298 = LINE ( 'NONE', #21690, #22804 ) ;
#4299 = EDGE_CURVE ( 'NONE', #3596, #18166, #12148, .T. ) ;
#4300 = CARTESIAN_POINT ( 'NONE',  ( 96.84719886470459471, -3.152801135295355994, 1.562500001365591418 ) ) ;
#4301 = CARTESIAN_POINT ( 'NONE',  ( 199.8599772695822878, 36.00000000000001421, 12.29462155906273502 ) ) ;
#4302 = AXIS2_PLACEMENT_3D ( 'NONE', #7000, #15694, #24688 ) ;
#4304 = EDGE_CURVE ( 'NONE', #947, #15078, #18125, .T. ) ;
#4303 = CARTESIAN_POINT ( 'NONE',  ( 99.99999999999995737, 4.458734125000016313, 13.18750000136559208 ) ) ;
#4305 = CARTESIAN_POINT ( 'NONE',  ( 95.00472066334982912, 103.1245878333314323, -52.82500000273118701 ) ) ;
#4306 = CARTESIAN_POINT ( 'NONE',  ( 107.0000000000000142, 110.0000000000000000, -55.00000000000000711 ) ) ;
#4307 = DIRECTION ( 'NONE',  ( 0.000000000000000000, 0.000000000000000000, -1.000000000000000000 ) ) ;
#4308 = CARTESIAN_POINT ( 'NONE',  ( 9.295050272127046043, 33.11210937608393579, -9.295050272127046043 ) ) ;
#4309 = CARTESIAN_POINT ( 'NONE',  ( -13.14518615778179900, 40.70234375108393721, -5.444914386472297529 ) ) ;
#4310 = EDGE_CURVE ( 'NONE', #2357, #2527, #14284, .T. ) ;
#4311 = CARTESIAN_POINT ( 'NONE',  ( 102.4976396683250783, 102.3130555110000159, -49.27499999726882152 ) ) ;
#4312 = EDGE_LOOP ( 'NONE', ( #15865, #11332, #4570, #17656 ) ) ;
#4313 =( BOUNDED_CURVE ( )  B_SPLINE_CURVE ( 2, ( #27249, #15962, #5583, #27109, #22686, #11680, #3156, #16399, #12235 ),
 .UNSPECIFIED., .F., .T. ) 
 B_SPLINE_CURVE_WITH_KNOTS ( ( 3, 2, 2, 2, 3 ),
 ( 0.2291666666666665741, 0.2395833333333332316, 0.2499999999999998335, 0.2604166666666665186, 0.2708333333333330928 ),
 .UNSPECIFIED. ) 
 CURVE ( )  GEOMETRIC_REPRESENTATION_ITEM ( )  RATIONAL_B_SPLINE_CURVE ( ( 1.000000000000000666, 0.9238795325112861834, 1.000000000000000000, 0.9238795325112867385, 1.000000000000000000, 0.9238795325112867385, 1.000000000000000000, 0.9238795325112884038, 0.9999999999999983347 ) ) 
 REPRESENTATION_ITEM ( '' )  );
#4314 = CARTESIAN_POINT ( 'NONE',  ( 120.4011555911795455, 37.22968750216787726, 9.598844408820459861 ) ) ;
#4315 = CARTESIAN_POINT ( 'NONE',  ( -8.312177448680279460E-16, 35.34453125216787583, -13.57481594606304576 ) ) ;
#4316 = CARTESIAN_POINT ( 'NONE',  ( 204.2950502721270425, 39.46210937608393010, -9.295050272127046043 ) ) ;
#4317 = ORIENTED_EDGE ( 'NONE', *, *, #5970, .F. ) ;
#4318 = CARTESIAN_POINT ( 'NONE',  ( 135.6228728715777834, 39.95820312499999716, -13.57481594606312036 ) ) ;
#4319 = ORIENTED_EDGE ( 'NONE', *, *, #24397, .F. ) ;
#4320 = CARTESIAN_POINT ( 'NONE',  ( 94.33688103937537051, 114.1144967660473242, -50.20000000000000995 ) ) ;
#4321 = AXIS2_PLACEMENT_3D ( 'NONE', #26443, #23594, #13007 ) ;
#4322 = CARTESIAN_POINT ( 'NONE',  ( -13.14518615778179189, 39.80937500108392868, 5.444914386472304635 ) ) ;
#4323 = CARTESIAN_POINT ( 'NONE',  ( 99.14382582708707048, 123.0000000010925021, -2.066987299999999195 ) ) ;
#4324 = CARTESIAN_POINT ( 'NONE',  ( 130.0000000000000000, 31.77265625216787370, 13.57481594606304576 ) ) ;
#4325 =( LENGTH_UNIT ( ) NAMED_UNIT ( * ) SI_UNIT ( .MILLI., .METRE. ) );
#4326 = CARTESIAN_POINT ( 'NONE',  ( 103.5355339059327093, 81.75000000273119838, -3.535533905932755072 ) ) ;
#4327 = DIRECTION ( 'NONE',  ( 1.000000000000000000, 0.000000000000000000, 0.000000000000000000 ) ) ;
#4328 = CARTESIAN_POINT ( 'NONE',  ( 181.8548138422181921, 35.93984375108393436, -5.444914386472297529 ) ) ;
#4329 = ORIENTED_EDGE ( 'NONE', *, *, #8782, .F. ) ;
#4330 = ORIENTED_EDGE ( 'NONE', *, *, #20686, .T. ) ;
#4331 = ORIENTED_EDGE ( 'NONE', *, *, #3900, .F. ) ;
#4332 = CARTESIAN_POINT ( 'NONE',  ( 9.295050272127047819, 38.66835937608393436, 9.295050272127046043 ) ) ;
#4333 = SURFACE_SIDE_STYLE ('',( #23719 ) ) ;
#4334 = CARTESIAN_POINT ( 'NONE',  ( 104.4587341249999781, 1.846868145590750521, 11.25000000136559386 ) ) ;
#4335 = CARTESIAN_POINT ( 'NONE',  ( 102.4999999999999858, 124.6500000000000057, -1.035533905932742638 ) ) ;
#4336 = CARTESIAN_POINT ( 'NONE',  ( 51.42518405393695957, 36.28710937716787299, -5.622872871577872189 ) ) ;
#4337 = CARTESIAN_POINT ( 'NONE',  ( 185.7049497278729575, 38.27148437608393294, 9.295050272127047819 ) ) ;
#4338 = CARTESIAN_POINT ( 'NONE',  ( -5.444914386472299306, 39.31328125108392868, 13.14518615778179722 ) ) ;
#4339 = DIRECTION ( 'NONE',  ( -0.000000000000000000, 1.000000000000000000, -0.000000000000000000 ) ) ;
#4340 = VECTOR ( 'NONE', #20910, 1000.000000000000114 ) ;
#4341 = CARTESIAN_POINT ( 'NONE',  ( 99.99999999999998579, 91.75000000000000000, 4.999999999999984013 ) ) ;
#4342 = CARTESIAN_POINT ( 'NONE',  ( 65.00000000000000000, 36.03906250000000000, -13.57481594606304576 ) ) ;
#4343 = CARTESIAN_POINT ( 'NONE',  ( 104.9952793366501709, 103.1245878333314323, -50.92499999726882010 ) ) ;
#4344 = ORIENTED_EDGE ( 'NONE', *, *, #18830, .T. ) ;
#4345 = CARTESIAN_POINT ( 'NONE',  ( -13.57481594606304576, 37.08085937499999574, 5.622872871577880183 ) ) ;
#4346 = CARTESIAN_POINT ( 'NONE',  ( -5.444914386472299306, 37.52734375108393294, 13.14518615778179722 ) ) ;
#4347 = AXIS2_PLACEMENT_3D ( 'NONE', #10855, #13559, #17565 ) ;
#4348 = AXIS2_PLACEMENT_3D ( 'NONE', #22690, #5587, #9977 ) ;
#4349 = CARTESIAN_POINT ( 'NONE',  ( 94.99999999999995737, -2.071067811865466624, 2.187500002731185500 ) ) ;
#4350 = CARTESIAN_POINT ( 'NONE',  ( 143.1451861577818079, 34.84843750108393579, -5.444914386472297529 ) ) ;
#4351 = CARTESIAN_POINT ( 'NONE',  ( 55.70494972787295751, 32.71523437608393436, 9.295050272127047819 ) ) ;
#4352 = CARTESIAN_POINT ( 'NONE',  ( 181.8548138422181921, 36.83281250108393579, 5.444914386472304635 ) ) ;
#4353 = CARTESIAN_POINT ( 'NONE',  ( 99.99999999999998579, 125.0000000000000000, 2.499999999999985789 ) ) ;
#4354 = CARTESIAN_POINT ( 'NONE',  ( 134.0625835405769237, 50.00000000116060761, -12.98908657125173960 ) ) ;
#4355 = CARTESIAN_POINT ( 'NONE',  ( 104.9999999999999716, 1.449011120738813565E-14, 34.79898987322334136 ) ) ;
#4356 = CARTESIAN_POINT ( 'NONE',  ( 2.493653234604083739E-15, 32.46718749999999432, 13.57481594606304576 ) ) ;
#4357 = CARTESIAN_POINT ( 'NONE',  ( 97.50236033167492167, 117.6869444889999841, -51.52500000273119696 ) ) ;
#4358 =( BOUNDED_CURVE ( )  B_SPLINE_CURVE ( 2, ( #27634, #10080, #23217, #27771, #18792, #21355, #12356, #25208, #8093, #1563, #27225 ),
 .UNSPECIFIED., .F., .F. ) 
 B_SPLINE_CURVE_WITH_KNOTS ( ( 3, 2, 2, 2, 2, 3 ),
 ( 0.4999999999999996669, 0.5199999999999996847, 0.5399999999999998135, 0.5599999999999998312, 0.5799999999999998490, 0.5999999999999998668 ),
 .UNSPECIFIED. ) 
 CURVE ( )  GEOMETRIC_REPRESENTATION_ITEM ( )  RATIONAL_B_SPLINE_CURVE ( ( 1.000000000000000888, 0.9510565162951527540, 1.000000000000000000, 0.9510565162951535312, 1.000000000000000000, 0.9510565162951535312, 1.000000000000000000, 0.9510565162951535312, 1.000000000000000000, 0.9510565162951537532, 0.9999999999999997780 ) ) 
 REPRESENTATION_ITEM ( '' )  );
#4359 = CARTESIAN_POINT ( 'NONE',  ( -13.14518615778179900, 35.74140625108393721, -5.444914386472297529 ) ) ;
#4360 = DIRECTION ( 'NONE',  ( -0.000000000000000000, 1.000000000000000000, -0.000000000000000000 ) ) ;
#4361 = CARTESIAN_POINT ( 'NONE',  ( 97.50000000000000000, 122.7500000021849615, 1.035533905932725096 ) ) ;
#4362 = CARTESIAN_POINT ( 'NONE',  ( 219.9999999999999716, 55.00000000000000000, -10.00000000000000000 ) ) ;
#4363 = CARTESIAN_POINT ( 'NONE',  ( -8.312177448680279460E-16, 36.83281249999999574, -13.57481594606304576 ) ) ;
#4364 = ORIENTED_EDGE ( 'NONE', *, *, #6983, .T. ) ;
#4365 = CARTESIAN_POINT ( 'NONE',  ( 101.8468681455906903, 4.458734125000016313, 8.125000001365592084 ) ) ;
#4366 = AXIS2_PLACEMENT_3D ( 'NONE', #5476, #20864, #1346 ) ;
#4367 = VERTEX_POINT ( 'NONE', #3239 ) ;
#4368 = CARTESIAN_POINT ( 'NONE',  ( 97.93301270000000613, 123.7500000010924879, -9.540979117872439019E-15 ) ) ;
#4369 = CARTESIAN_POINT ( 'NONE',  ( 98.15313185440925281, 4.458734125000016313, 13.25000000136559208 ) ) ;
#4370 = CARTESIAN_POINT ( 'NONE',  ( 121.2273907538632898, 50.37415326813481897, 15.00000000000582645 ) ) ;
#4371 = CARTESIAN_POINT ( 'NONE',  ( 5.444914386472302859, 40.00781250108393294, 13.14518615778179189 ) ) ;
#4372 = CARTESIAN_POINT ( 'NONE',  ( 100.0000000000000000, 110.0000000000000000, -55.00000000000000711 ) ) ;
#4373 = CARTESIAN_POINT ( 'NONE',  ( 101.8468681455906903, 80.00000000136559208, 4.458734124999987891 ) ) ;
#4374 = CARTESIAN_POINT ( 'NONE',  ( 51.85481384221819923, 34.35234375108393579, -5.444914386472297529 ) ) ;
#4375 = CARTESIAN_POINT ( 'NONE',  ( 91.91746824999999887, 110.0000000000000000, -49.12500000273119838 ) ) ;
#4376 = CYLINDRICAL_SURFACE ( 'NONE', #23682, 13.57481594606304398 ) ;
#4377 = EDGE_LOOP ( 'NONE', ( #1231, #15868, #14798, #15280 ) ) ;
#4378 = CARTESIAN_POINT ( 'NONE',  ( -13.57481594606304398, 39.46210937499999005, 5.622872871577880183 ) ) ;
#4379 = DIRECTION ( 'NONE',  ( 0.000000000000000000, 0.000000000000000000, 1.000000000000000000 ) ) ;
#4380 = CARTESIAN_POINT ( 'NONE',  ( 97.83688103937535629, 116.6573956140660897, -54.89999999453763735 ) ) ;
#4381 = CARTESIAN_POINT ( 'NONE',  ( 116.4251840539369454, 36.18789062499999432, -5.622872871577873077 ) ) ;
#4382 = ORIENTED_EDGE ( 'NONE', *, *, #8158, .T. ) ;
#4383 = CARTESIAN_POINT ( 'NONE',  ( 99.99999999999998579, 128.0000000000000000, -2.500000000000013767 ) ) ;
#4384 = CARTESIAN_POINT ( 'NONE',  ( 5.444914386472297529, 36.53515625108393294, -13.14518615778179900 ) ) ;
#4385 = CARTESIAN_POINT ( 'NONE',  ( 13.57481594606304753, 38.37070312716786447, -5.622872871577873077 ) ) ;
#4386 = CARTESIAN_POINT ( 'NONE',  ( 120.7049497278729575, 37.27929687608393294, -9.295050272127046043 ) ) ;
#4387 = CARTESIAN_POINT ( 'NONE',  ( 70.62287287157786864, 34.50117187716788436, -13.57481594606304753 ) ) ;
#4388 = ADVANCED_FACE ( 'NONE', ( #7074 ), #685, .F. ) ;
#4389 = DIRECTION ( 'NONE',  ( 0.000000000000000000, 0.000000000000000000, -1.000000000000000000 ) ) ;
#4390 = CARTESIAN_POINT ( 'NONE',  ( 5.622872871577878406, 31.82226562716787654, 13.57481594606304576 ) ) ;
#4391 = CIRCLE ( 'NONE', #759, 11.50000000000001776 ) ;
#4392 = CARTESIAN_POINT ( 'NONE',  ( 99.99999999999995737, -4.999999999999990230, 6.249999999999998224 ) ) ;
#4393 = CARTESIAN_POINT ( 'NONE',  ( 99.99999999999997158, 101.5015231886685712, -49.37499999726882294 ) ) ;
#4394 = CARTESIAN_POINT ( 'NONE',  ( 195.0000000000000000, 34.40195312608393152, 13.14518615778179544 ) ) ;
#4395 =( BOUNDED_CURVE ( )  B_SPLINE_CURVE ( 2, ( #18183, #7340, #5364, #20476, #3221, #953, #2798 ),
 .UNSPECIFIED., .F., .T. ) 
 B_SPLINE_CURVE_WITH_KNOTS ( ( 3, 2, 2, 3 ),
 ( 0.7500000000000006661, 0.7750000000000004663, 0.8000000000000002665, 0.8250000005912483392 ),
 .UNSPECIFIED. ) 
 CURVE ( )  GEOMETRIC_REPRESENTATION_ITEM ( )  RATIONAL_B_SPLINE_CURVE ( ( 0.9999999999999980016, 0.9238795325112887369, 1.000000000000000000, 0.9238795325112867385, 1.000000000000000000, 0.9238795325112867385, 1.000000000000000000 ) ) 
 REPRESENTATION_ITEM ( '' )  );
#4396 = LINE ( 'NONE', #23917, #22880 ) ;
#4397 = CARTESIAN_POINT ( 'NONE',  ( 139.2950502721270425, 36.08867187608392868, 9.295050272127046043 ) ) ;
#4398 = CARTESIAN_POINT ( 'NONE',  ( 99.99999999999998579, 122.9000000021849530, 2.499999999999978684 ) ) ;
#4399 = LINE ( 'NONE', #27924, #13581 ) ;
#4400 = CARTESIAN_POINT ( 'NONE',  ( 208.5748159460630688, 36.58476562499999574, 5.622872871577868636 ) ) ;
#4401 = CARTESIAN_POINT ( 'NONE',  ( 9.598844408820459861, 38.12265624999999858, 9.598844408820456309 ) ) ;
#4402 = CARTESIAN_POINT ( 'NONE',  ( 0.000000000000000000, -7.395377635281828788, 0.000000000000000000 ) ) ;
#4403 = AXIS2_PLACEMENT_3D ( 'NONE', #14813, #21261, #6556 ) ;
#4404 = CARTESIAN_POINT ( 'NONE',  ( -5.444914386472297529, 36.63437500108393152, -13.14518615778179900 ) ) ;
#4405 = CARTESIAN_POINT ( 'NONE',  ( 5.444914386472297529, 38.71796875108393721, -13.14518615778179900 ) ) ;
#4406 = CARTESIAN_POINT ( 'NONE',  ( 204.5988444088204403, 35.14609374999999858, -9.598844408820458085 ) ) ;
#4407 = CARTESIAN_POINT ( 'NONE',  ( 95.00472066334981491, 116.8754121666685393, -47.67500000273120975 ) ) ;
#4408 = CARTESIAN_POINT ( 'NONE',  ( 13.57481594606304753, 39.06523437499999574, -5.622872871577873966 ) ) ;
#4409 = CARTESIAN_POINT ( 'NONE',  ( 65.00000000000000000, 35.98945312608393010, 13.14518615778179544 ) ) ;
#4410 = CARTESIAN_POINT ( 'NONE',  ( 99.99999999999995737, -4.458734124999988779, 3.687500001365591640 ) ) ;
#4411 = CARTESIAN_POINT ( 'NONE',  ( 97.83688103937538472, 116.6573956140660897, -44.90000000546237402 ) ) ;
#4412 = CARTESIAN_POINT ( 'NONE',  ( 95.54126587499999346, 93.74999999863439371, -1.846868145590737864 ) ) ;
#4413 = CIRCLE ( 'NONE', #2137, 2.499999999999995115 ) ;
#4414 = CARTESIAN_POINT ( 'NONE',  ( 98.14149105024047515, 122.9999999999999432, -0.9146729478038871930 ) ) ;
#4415 = CARTESIAN_POINT ( 'NONE',  ( 9.598844408820456309, 36.73359374999999716, -9.598844408820458085 ) ) ;
#4416 = CARTESIAN_POINT ( 'NONE',  ( 139.2950502721270425, 40.45429687608393721, -9.295050272127046043 ) ) ;
#4417 = ORIENTED_EDGE ( 'NONE', *, *, #7410, .T. ) ;
#4418 = VECTOR ( 'NONE', #17117, 1000.000000000000000 ) ;
#4419 = VERTEX_POINT ( 'NONE', #18491 ) ;
#4420 = CARTESIAN_POINT ( 'NONE',  ( 96.84719886470459471, 80.81250000136559208, 3.152801135295355994 ) ) ;
#4421 = CARTESIAN_POINT ( 'NONE',  ( 101.8468681455907330, 93.49999999863442213, -4.458734124999994997 ) ) ;
#4422 = CARTESIAN_POINT ( 'NONE',  ( 62.91300135136894056, 36.00000000000000000, -13.31420566034952380 ) ) ;
#4423 = ORIENTED_EDGE ( 'NONE', *, *, #15615, .F. ) ;
#4424 = CARTESIAN_POINT ( 'NONE',  ( 104.3262379212492448, 115.9545556584642867, -51.70000000000001705 ) ) ;
#4425 = CARTESIAN_POINT ( 'NONE',  ( 78.14518615778179367, 36.33671875108394289, 5.444914386472293977 ) ) ;
#4426 = ORIENTED_EDGE ( 'NONE', *, *, #20131, .F. ) ;
#4427 = EDGE_CURVE ( 'NONE', #21367, #4613, #25948, .T. ) ;
#4428 = CARTESIAN_POINT ( 'NONE',  ( 2.849501950123402596E-15, 1.000000000000000000, -23.26794919243112858 ) ) ;
#4429 = CARTESIAN_POINT ( 'NONE',  ( 95.54126587499995082, 1.846868145590750077, 1.625000001365592972 ) ) ;
#4430 = EDGE_CURVE ( 'NONE', #28041, #4816, #656, .T. ) ;
#4431 = VERTEX_POINT ( 'NONE', #975 ) ;
#4432 = CARTESIAN_POINT ( 'NONE',  ( 9.295050272127047819, 33.90585937608393863, 9.295050272127046043 ) ) ;
#4433 = CARTESIAN_POINT ( 'NONE',  ( 13.14518615778179544, 40.35507812608393863, -1.609821015232357215E-15 ) ) ;
#4434 = CARTESIAN_POINT ( 'NONE',  ( 185.4011555911795597, 38.81718750216787583, 9.598844408820459861 ) ) ;
#4435 = CARTESIAN_POINT ( 'NONE',  ( -13.14518615778179722, 34.94765625108394147, -5.444914386472297529 ) ) ;
#4436 = CARTESIAN_POINT ( 'NONE',  ( 3.878384841496545388, 31.34156311272377238, -13.57481594606304753 ) ) ;
#4437 = CARTESIAN_POINT ( 'NONE',  ( 116.8548138422182205, 37.62656250108393152, 5.444914386472304635 ) ) ;
#4438 = CARTESIAN_POINT ( 'NONE',  ( 9.295050272127046043, 38.07304687608393579, -9.295050272127046043 ) ) ;
#4439 = CARTESIAN_POINT ( 'NONE',  ( 143.1451861577818079, 34.60039062608392868, -1.609821015232357215E-15 ) ) ;
#4440 = CARTESIAN_POINT ( 'NONE',  ( 78.57481594606304043, 35.89023437499999858, -5.622872871577873077 ) ) ;
#4441 = CARTESIAN_POINT ( 'NONE',  ( 55.40115559117954547, 39.41250000216787441, -9.598844408820458085 ) ) ;
#4442 = EDGE_CURVE ( 'NONE', #27424, #3039, #17958, .T. ) ;
#4443 = CARTESIAN_POINT ( 'NONE',  ( 101.8468681455906903, -4.458734124999987891, 11.00000000136559208 ) ) ;
#4444 = DIRECTION ( 'NONE',  ( 1.000000000000000000, -0.000000000000000000, -5.782411586589357392E-17 ) ) ;
#4445 = CARTESIAN_POINT ( 'NONE',  ( 95.54126587499996504, 1.387778780781445676E-14, 13.43750000136559386 ) ) ;
#4446 = CARTESIAN_POINT ( 'NONE',  ( 91.91746824999999887, 110.0000000000000000, -49.12500000273119838 ) ) ;
#4447 = DIRECTION ( 'NONE',  ( 1.000000000000000000, 0.000000000000000000, 0.000000000000000000 ) ) ;
#4448 = CARTESIAN_POINT ( 'NONE',  ( 99.99999999999995737, 80.43750000136559208, -4.458734125000016313 ) ) ;
#4449 = CARTESIAN_POINT ( 'NONE',  ( 106.5389055433250860, 114.7507929638356785, -48.42499999726882010 ) ) ;
#4450 = CARTESIAN_POINT ( 'NONE',  ( 5.444914386472297529, 36.53515625108393294, -13.14518615778179900 ) ) ;
#4451 = CARTESIAN_POINT ( 'NONE',  ( 104.9952793366501709, 116.8754121666685393, -48.57499999726881867 ) ) ;
#4452 = ORIENTED_EDGE ( 'NONE', *, *, #20813, .F. ) ;
#4453 = CYLINDRICAL_SURFACE ( 'NONE', #13603, 4.999999999999989342 ) ;
#4454 = CARTESIAN_POINT ( 'NONE',  ( 195.0000000000000000, -7.395377635281828788, -2.255140518769849538E-14 ) ) ;
#4455 = DIRECTION ( 'NONE',  ( 0.000000000000000000, 0.000000000000000000, 1.000000000000000000 ) ) ;
#4456 = EDGE_CURVE ( 'NONE', #11568, #4141, #26911, .T. ) ;
#4457 = CARTESIAN_POINT ( 'NONE',  ( 204.2950502721270425, 40.25585937608393294, -9.295050272127046043 ) ) ;
#4458 = VERTEX_POINT ( 'NONE', #24621 ) ;
#4459 = CARTESIAN_POINT ( 'NONE',  ( 139.5988444088204403, 36.03906250216787299, -9.598844408820458085 ) ) ;
#4460 = FACE_OUTER_BOUND ( 'NONE', #25903, .T. ) ;
#4461 = CARTESIAN_POINT ( 'NONE',  ( 103.1528011352953342, 3.152801135295383084, 13.31250000136559386 ) ) ;
#4462 = ORIENTED_EDGE ( 'NONE', *, *, #14513, .F. ) ;
#4463 = CARTESIAN_POINT ( 'NONE',  ( 107.0000000000000142, 107.7255621263696526, -53.10000000000000142 ) ) ;
#4464 = CARTESIAN_POINT ( 'NONE',  ( 13.57481594606304931, 33.50898437716787015, 5.622872871577868636 ) ) ;
#4465 = CARTESIAN_POINT ( 'NONE',  ( 103.5355339059327235, 92.99999999726881583, -3.535533905932738197 ) ) ;
#4466 = EDGE_CURVE ( 'NONE', #506, #4887, #11580, .T. ) ;
#4467 = CARTESIAN_POINT ( 'NONE',  ( 124.5550856135277087, 39.90859375108393436, 13.14518615778179722 ) ) ;
#4468 = DIRECTION ( 'NONE',  ( 0.000000000000000000, 0.000000000000000000, -1.000000000000000000 ) ) ;
#4469 = CARTESIAN_POINT ( 'NONE',  ( 95.00000000000000000, 92.31249999726880162, -2.071067811865479058 ) ) ;
#4470 = CARTESIAN_POINT ( 'NONE',  ( 51.85481384221819923, 39.11484375108394573, -5.444914386472297529 ) ) ;
#4471 = DIRECTION ( 'NONE',  ( 0.000000000000000000, 0.000000000000000000, -1.000000000000000000 ) ) ;
#4472 = CARTESIAN_POINT ( 'NONE',  ( 200.4449143864723055, 34.94765625108394147, -13.14518615778179900 ) ) ;
#4473 = ORIENTED_EDGE ( 'NONE', *, *, #1321, .T. ) ;
#4474 = ORIENTED_EDGE ( 'NONE', *, *, #10559, .T. ) ;
#4475 = ORIENTED_EDGE ( 'NONE', *, *, #21691, .T. ) ;
#4476 = CARTESIAN_POINT ( 'NONE',  ( -5.444914386472299306, 37.72578125108395142, 13.14518615778179722 ) ) ;
#4477 = CARTESIAN_POINT ( 'NONE',  ( 0.000000000000000000, 0.000000000000000000, 0.000000000000000000 ) ) ;
#4478 = CARTESIAN_POINT ( 'NONE',  ( 95.54126587499996504, 1.387778780781445676E-14, 9.687500001365593860 ) ) ;
#4479 =( BOUNDED_CURVE ( )  B_SPLINE_CURVE ( 2, ( #25280, #20738, #25012, #25562, #14576, #7758, #14710, #18861, #27710 ),
 .UNSPECIFIED., .F., .T. ) 
 B_SPLINE_CURVE_WITH_KNOTS ( ( 3, 2, 2, 2, 3 ),
 ( 0.8571428571428570953, 0.8660714285714286031, 0.8750000000000000000, 0.8839285714285712858, 0.8928571428571427937 ),
 .UNSPECIFIED. ) 
 CURVE ( )  GEOMETRIC_REPRESENTATION_ITEM ( )  RATIONAL_B_SPLINE_CURVE ( ( 1.000000000000000000, 0.9238795325112867385, 1.000000000000000000, 0.9238795325112867385, 1.000000000000000000, 0.9238795325112867385, 1.000000000000000000, 0.9238795325112877377, 0.9999999999999990008 ) ) 
 REPRESENTATION_ITEM ( '' )  );
#4480 = CARTESIAN_POINT ( 'NONE',  ( 99.99999999999995737, 82.18750000136559208, -4.458734125000016313 ) ) ;
#4481 = CARTESIAN_POINT ( 'NONE',  ( 181.8548138422182205, 39.01562500108393294, 5.444914386472304635 ) ) ;
#4482 = CARTESIAN_POINT ( 'NONE',  ( -9.295050272127046043, 37.47773437608393010, -9.295050272127046043 ) ) ;
#4483 = CARTESIAN_POINT ( 'NONE',  ( 189.6345034319466549, 54.48174559707876341, 14.99999999999995026 ) ) ;
#4484 = LINE ( 'NONE', #22011, #2089 ) ;
#4485 = LINE ( 'NONE', #25860, #22307 ) ;
#4486 = CARTESIAN_POINT ( 'NONE',  ( 91.91746824999997045, 112.6261737610028320, -53.72499999726881725 ) ) ;
#4487 = AXIS2_PLACEMENT_3D ( 'NONE', #271, #8957, #15501 ) ;
#4488 = ORIENTED_EDGE ( 'NONE', *, *, #21320, .F. ) ;
#4489 = CARTESIAN_POINT ( 'NONE',  ( -9.598844408820454532, 36.33671874999999574, 9.598844408820459861 ) ) ;
#4490 = CARTESIAN_POINT ( 'NONE',  ( 9.295050272127047819, 36.88242187608393152, 9.295050272127046043 ) ) ;
#4491 = CARTESIAN_POINT ( 'NONE',  ( 97.92893218813451028, -4.999999999999989342, 1.312500002731184612 ) ) ;
#4492 = CARTESIAN_POINT ( 'NONE',  ( 135.4449143864723055, 36.23750000108393721, 13.14518615778179189 ) ) ;
#4493 = CARTESIAN_POINT ( 'NONE',  ( 70.44491438647230552, 34.45156250108393436, 13.14518615778179189 ) ) ;
#4494 = CARTESIAN_POINT ( 'NONE',  ( 185.7049497278729575, 38.46992187608393721, 9.295050272127047819 ) ) ;
#4495 = ORIENTED_EDGE ( 'NONE', *, *, #3570, .T. ) ;
#4496 = CARTESIAN_POINT ( 'NONE',  ( 84.99999999999998579, -14.99999999999999467, 15.00000000000000000 ) ) ;
#4497 = CARTESIAN_POINT ( 'NONE',  ( -13.14518615778179900, 32.56640625108394005, -5.444914386472297529 ) ) ;
#4498 = CARTESIAN_POINT ( 'NONE',  ( 135.3654965680425732, 54.48174559707607756, -15.00000000000000178 ) ) ;
#4499 = ADVANCED_FACE ( 'NONE', ( #11623 ), #16049, .T. ) ;
#4500 = DIRECTION ( 'NONE',  ( -1.156482317317871478E-16, 0.000000000000000000, -1.000000000000000000 ) ) ;
#4501 = CARTESIAN_POINT ( 'NONE',  ( 143.5748159460630404, 39.85898437716787157, 5.622872871577869525 ) ) ;
#4502 = DIRECTION ( 'NONE',  ( 0.000000000000000000, 1.000000000000000000, 0.000000000000000000 ) ) ;
#4503 = CARTESIAN_POINT ( 'NONE',  ( -6.116560239716795522, 54.66944451632673463, 14.99999999999999822 ) ) ;
#4504 = CARTESIAN_POINT ( 'NONE',  ( 102.4999999999999716, 123.1500000021849672, -1.035533905932742638 ) ) ;
#4505 = CARTESIAN_POINT ( 'NONE',  ( 56.78868598481955843, 50.68678854790645971, 14.99999999999929479 ) ) ;
#4506 = AXIS2_PLACEMENT_3D ( 'NONE', #13491, #13773, #11494 ) ;
#4507 = CARTESIAN_POINT ( 'NONE',  ( 98.15313185440925281, 4.458734125000016313, 10.25000000136559386 ) ) ;
#4508 = VERTEX_POINT ( 'NONE', #5663 ) ;
#4509 = CARTESIAN_POINT ( 'NONE',  ( 102.0669872999999939, 124.1000000010924964, 0.8561741729129311862 ) ) ;
#4510 = CARTESIAN_POINT ( 'NONE',  ( 99.99999999999995737, -4.458734124999988779, 11.68750000136559208 ) ) ;
#4511 = CARTESIAN_POINT ( 'NONE',  ( 120.8198241863519939, 50.00000000000000000, 9.999999999999968026 ) ) ;
#4512 = CARTESIAN_POINT ( 'NONE',  ( -5.444914386472299306, 38.32109375108394289, 13.14518615778179722 ) ) ;
#4513 = CARTESIAN_POINT ( 'NONE',  ( 5.622872871577733633, 32.81445312500000000, -13.57481594606318254 ) ) ;
#4514 = LINE ( 'NONE', #9624, #14211 ) ;
#4515 = CARTESIAN_POINT ( 'NONE',  ( 59.55508561352770158, 36.13828125108393863, 13.14518615778179722 ) ) ;
#4516 = CARTESIAN_POINT ( 'NONE',  ( 95.00472066334982912, 103.1245878333314323, -45.07500000273119412 ) ) ;
#4517 = CARTESIAN_POINT ( 'NONE',  ( 5.444914386472302859, 37.62656250108393152, 13.14518615778179189 ) ) ;
#4518 = CARTESIAN_POINT ( 'NONE',  ( 116.4251840539369596, 36.18789062499999432, -5.622872871577872189 ) ) ;
#4519 = CARTESIAN_POINT ( 'NONE',  ( 104.3262379212492448, 115.9545556584642867, -49.70000000000001705 ) ) ;
#4520 = CARTESIAN_POINT ( 'NONE',  ( 143.5748159460630404, 36.68398437499999432, -5.622872871577873077 ) ) ;
#4521 = ORIENTED_EDGE ( 'NONE', *, *, #20656, .T. ) ;
#4522 = DIRECTION ( 'NONE',  ( -0.000000000000000000, -1.000000000000000000, -0.000000000000000000 ) ) ;
#4523 = CARTESIAN_POINT ( 'NONE',  ( -9.295050272127044266, 36.08867187608393579, 9.295050272127047819 ) ) ;
#4524 = CARTESIAN_POINT ( 'NONE',  ( -8.312177448680279460E-16, 36.93203125216787441, -13.57481594606304576 ) ) ;
#4525 = CARTESIAN_POINT ( 'NONE',  ( 143.1451861577818079, 36.98164062608393010, -1.609821015232357215E-15 ) ) ;
#4526 = CARTESIAN_POINT ( 'NONE',  ( 65.00000000000000000, 32.56640625216787299, 13.57481594606304576 ) ) ;
#4527 = DIRECTION ( 'NONE',  ( 0.000000000000000000, 0.000000000000000000, 1.000000000000000000 ) ) ;
#4528 = COLOUR_RGB ( '', 0.08235294, 0.09019608, 0.10196078) ;
#4529 = CARTESIAN_POINT ( 'NONE',  ( 13.57481594606304753, 33.60820312716787583, -5.622872871577873077 ) ) ;
#4530 = VECTOR ( 'NONE', #23690, 1000.000000000000000 ) ;
#4531 = CARTESIAN_POINT ( 'NONE',  ( 103.5355339059327093, 3.535533905932755072, 6.624999999999999112 ) ) ;
#4532 = CARTESIAN_POINT ( 'NONE',  ( 181.8548138422181921, 35.04687500108393294, 5.444914386472304635 ) ) ;
#4533 = CARTESIAN_POINT ( 'NONE',  ( -5.622872871577873966, 34.10429687716786873, 13.57481594606304753 ) ) ;
#4534 = CARTESIAN_POINT ( 'NONE',  ( 104.9999999999999858, 93.00000000000000000, -6.938893903907228378E-15 ) ) ;
#4535 = VERTEX_POINT ( 'NONE', #27332 ) ;
#4537 = ORIENTED_EDGE ( 'NONE', *, *, #6691, .F. ) ;
#4536 = CARTESIAN_POINT ( 'NONE',  ( 200.6228728715779539, 39.16445312500000142, -13.57481594606299247 ) ) ;
#4538 = CARTESIAN_POINT ( 'NONE',  ( 96.46446609406721961, 3.535533905932755072, 6.874999999999999112 ) ) ;
#4539 = CARTESIAN_POINT ( 'NONE',  ( 92.99999999999998579, 107.7255621263696952, -48.39999999453764445 ) ) ;
#4540 = CARTESIAN_POINT ( 'NONE',  ( -9.598844408820454532, 37.92421874999999432, 9.598844408820459861 ) ) ;
#4541 = CARTESIAN_POINT ( 'NONE',  ( 0.3745404134779373173, 36.00000000000003553, -13.51869779562201757 ) ) ;
#4542 = CARTESIAN_POINT ( 'NONE',  ( 9.295050272127047819, 37.08085937608393579, 9.295050272127046043 ) ) ;
#4543 = CARTESIAN_POINT ( 'NONE',  ( 13.14518615778179544, 35.39414062608393152, -1.609821015232357215E-15 ) ) ;
#4544 = CARTESIAN_POINT ( 'NONE',  ( 189.3771271284221314, 33.70742187500000142, -13.57481594606304753 ) ) ;
#4545 = CARTESIAN_POINT ( 'NONE',  ( 95.00472066334981491, 116.8754121666685393, -45.67500000273119554 ) ) ;
#4546 = LINE ( 'NONE', #8676, #12390 ) ;
#4547 = CARTESIAN_POINT ( 'NONE',  ( 59.55508561352770158, 34.05468750108393294, -13.14518615778179900 ) ) ;
#4548 = ADVANCED_FACE ( 'NONE', ( #10322, #23046 ), #14327, .F. ) ;
#4549 = CARTESIAN_POINT ( 'NONE',  ( 103.1528011352953342, -3.152801135295355106, 1.812500001365591640 ) ) ;
#4550 = CARTESIAN_POINT ( 'NONE',  ( 101.0337790074118658, 123.0000000000000000, -2.280707637605766891 ) ) ;
#4551 = LINE ( 'NONE', #9626, #14531 ) ;
#4552 = CARTESIAN_POINT ( 'NONE',  ( 101.7677669529663547, 123.7000000000000028, 1.767766952966350891 ) ) ;
#4553 = CARTESIAN_POINT ( 'NONE',  ( 5.622872871577871301, 37.57695312499998863, -13.57481594606304753 ) ) ;
#4554 = CARTESIAN_POINT ( 'NONE',  ( 139.2950502721270425, 37.87460937608393863, 9.295050272127046043 ) ) ;
#4555 = ORIENTED_EDGE ( 'NONE', *, *, #28182, .F. ) ;
#4556 = CARTESIAN_POINT ( 'NONE',  ( 96.46446609406721961, 83.87500000000000000, -3.535533905932755072 ) ) ;
#4557 = CARTESIAN_POINT ( 'NONE',  ( 104.9999999999999716, 80.62500000273119838, -1.449011120738813565E-14 ) ) ;
#4558 = CARTESIAN_POINT ( 'NONE',  ( 98.15313185440925281, 94.99999999863439371, 4.458734124999979898 ) ) ;
#4559 = CARTESIAN_POINT ( 'NONE',  ( 53.06475762330939006, 36.00000000000000000, -5.809862729998005904 ) ) ;
#4560 = CARTESIAN_POINT ( 'NONE',  ( 94.33688103937534208, 114.1144967660473242, -49.20000000000001705 ) ) ;
#4561 = CARTESIAN_POINT ( 'NONE',  ( 51.85481384221819923, 34.35234375108393579, -5.444914386472297529 ) ) ;
#4562 = ORIENTED_EDGE ( 'NONE', *, *, #20293, .F. ) ;
#4563 =( BOUNDED_CURVE ( )  B_SPLINE_CURVE ( 2, ( #17617, #6785, #11895, #13894, #9351, #26900, #7490, #676, #18190 ),
 .UNSPECIFIED., .F., .F. ) 
 B_SPLINE_CURVE_WITH_KNOTS ( ( 3, 2, 2, 2, 3 ),
 ( 0.02083333333333358892, 0.03125000000000020123, 0.04166666666666681007, 0.05208333333333342585, 0.06250000000000004163 ),
 .UNSPECIFIED. ) 
 CURVE ( )  GEOMETRIC_REPRESENTATION_ITEM ( )  RATIONAL_B_SPLINE_CURVE ( ( 0.9999999999999981126, 0.9238795325112886259, 1.000000000000000000, 0.9238795325112867385, 1.000000000000000000, 0.9238795325112867385, 1.000000000000000000, 0.9238795325112864054, 1.000000000000000222 ) ) 
 REPRESENTATION_ITEM ( '' )  );
#4564 = CARTESIAN_POINT ( 'NONE',  ( 13.57481594606304753, 32.81445312716787299, -5.622872871577873966 ) ) ;
#4565 = CARTESIAN_POINT ( 'NONE',  ( 98.15313185440925281, -4.458734124999987891, 1.875000001365591862 ) ) ;
#4566 = VERTEX_POINT ( 'NONE', #27466 ) ;
#4567 = DIRECTION ( 'NONE',  ( 0.000000000000000000, 0.000000000000000000, -1.000000000000000000 ) ) ;
#4568 = CARTESIAN_POINT ( 'NONE',  ( -13.14518615778179900, 31.77265625108393365, -5.444914386472297529 ) ) ;
#4569 = CARTESIAN_POINT ( 'NONE',  ( 208.5748159460630120, 35.89023437716787868, 5.622872871577869525 ) ) ;
#4570 = ORIENTED_EDGE ( 'NONE', *, *, #11427, .F. ) ;
#4571 = CARTESIAN_POINT ( 'NONE',  ( 5.444914386472297529, 34.74921875108393721, -13.14518615778179722 ) ) ;
#4572 = CARTESIAN_POINT ( 'NONE',  ( 13.57481594606304576, 36.73359375216787015, -1.662435489736055892E-15 ) ) ;
#4573 = CARTESIAN_POINT ( 'NONE',  ( 124.5550856135277087, 36.13828125108393152, 13.14518615778179722 ) ) ;
#4574 = ORIENTED_EDGE ( 'NONE', *, *, #6386, .F. ) ;
#4576 = AXIS2_PLACEMENT_3D ( 'NONE', #14901, #19337, #25611 ) ;
#4575 = CARTESIAN_POINT ( 'NONE',  ( -9.295050272127044266, 36.08867187608393579, 9.295050272127047819 ) ) ;
#4577 = CARTESIAN_POINT ( 'NONE',  ( 135.4449143864723055, 36.33671875108394289, -13.14518615778179900 ) ) ;
#4578 = CARTESIAN_POINT ( 'NONE',  ( 74.59884440882045453, 35.14609374999999858, -9.598844408820458085 ) ) ;
#4579 = CARTESIAN_POINT ( 'NONE',  ( 103.5355339059327235, 92.12500000000000000, -3.535533905932738197 ) ) ;
#4580 = CARTESIAN_POINT ( 'NONE',  ( 104.4587341249999781, -1.846868145590721655, 10.12500000136559386 ) ) ;
#4581 = CARTESIAN_POINT ( 'NONE',  ( 181.4251840539369596, 37.03124999999999289, 0.000000000000000000 ) ) ;
#4582 = CARTESIAN_POINT ( 'NONE',  ( 104.4587341249999781, 1.846868145590750299, 2.000000001365591640 ) ) ;
#4583 = CARTESIAN_POINT ( 'NONE',  ( 102.4976396683250925, 102.3130555110000159, -50.52500000273119696 ) ) ;
#4584 = DIRECTION ( 'NONE',  ( 0.000000000000000000, 0.000000000000000000, 1.000000000000000000 ) ) ;
#4585 = CARTESIAN_POINT ( 'NONE',  ( 99.99999999999995737, 1.387778780781445676E-14, 34.79898987322334136 ) ) ;
#4586 = CARTESIAN_POINT ( 'NONE',  ( 102.4976396683250783, 117.6869444889999841, -52.22499999726882436 ) ) ;
#4587 = CARTESIAN_POINT ( 'NONE',  ( 9.295050272127046043, 37.27929687608394005, -9.295050272127046043 ) ) ;
#4588 = CARTESIAN_POINT ( 'NONE',  ( 106.5389055433250860, 105.2492070361643215, -47.07499999726882578 ) ) ;
#4589 = ORIENTED_EDGE ( 'NONE', *, *, #23600, .F. ) ;
#4590 = EDGE_CURVE ( 'NONE', #1922, #27220, #27600, .T. ) ;
#4591 = CARTESIAN_POINT ( 'NONE',  ( 98.53841926354351699, 123.2500000010924737, 1.461580736456455920 ) ) ;
#4592 = CARTESIAN_POINT ( 'NONE',  ( 116.4251840539369596, 37.13046875216787868, 0.000000000000000000 ) ) ;
#4593 = CARTESIAN_POINT ( 'NONE',  ( 208.1451861577817795, 39.41250000108393436, -5.444914386472297529 ) ) ;
#4594 = ORIENTED_EDGE ( 'NONE', *, *, #11950, .F. ) ;
#4595 = CARTESIAN_POINT ( 'NONE',  ( 104.9999999999999716, 1.449011120738813565E-14, 7.625000002731185056 ) ) ;
#4596 = CARTESIAN_POINT ( 'NONE',  ( 204.1801758136480203, 50.00000000000000000, -9.999999999999992895 ) ) ;
#4597 = FACE_OUTER_BOUND ( 'NONE', #20007, .T. ) ;
#4598 = EDGE_LOOP ( 'NONE', ( #3415, #23865, #7640, #25561 ) ) ;
#4599 = CARTESIAN_POINT ( 'NONE',  ( 94.33688103937537051, 114.1144967660473242, -48.20000000000000995 ) ) ;
#4600 = VECTOR ( 'NONE', #25704, 1000.000000000000000 ) ;
#4601 = CARTESIAN_POINT ( 'NONE',  ( 9.295050272127047819, 39.26367187608393294, 9.295050272127046043 ) ) ;
#4602 = CARTESIAN_POINT ( 'NONE',  ( 101.7677669529663547, 123.0999999999999943, -1.767766952966370209 ) ) ;
#4603 = CARTESIAN_POINT ( 'NONE',  ( 139.5988444088204403, 32.86406250216787583, -9.598844408820458085 ) ) ;
#4604 = CARTESIAN_POINT ( 'NONE',  ( -5.444914386472297529, 40.60312500108393863, -13.14518615778179722 ) ) ;
#4605 = ADVANCED_FACE ( 'NONE', ( #12180 ), #3936, .F. ) ;
#4606 =( BOUNDED_CURVE ( )  B_SPLINE_CURVE ( 2, ( #19158, #5781, #14307, #8185, #3499, #5921, #27314, #10452, #23165 ),
 .UNSPECIFIED., .F., .F. ) 
 B_SPLINE_CURVE_WITH_KNOTS ( ( 3, 2, 2, 2, 3 ),
 ( 0.1041666666666664909, 0.1145833333333332732, 0.1250000000000000833, 0.1354166666666668517, 0.1458333333333336757 ),
 .UNSPECIFIED. ) 
 CURVE ( )  GEOMETRIC_REPRESENTATION_ITEM ( )  RATIONAL_B_SPLINE_CURVE ( ( 1.000000000000001332, 0.9238795325112854062, 1.000000000000000000, 0.9238795325112867385, 1.000000000000000000, 0.9238795325112867385, 1.000000000000000000, 0.9238795325112842960, 1.000000000000002442 ) ) 
 REPRESENTATION_ITEM ( '' )  );
#4607 = ADVANCED_BREP_SHAPE_REPRESENTATION ( '', ( #7649, #26844 ), #10431 ) ;
#4608 = CARTESIAN_POINT ( 'NONE',  ( 99.99999999999998579, 92.12499999726880162, -4.999999999999997335 ) ) ;
#4609 = CARTESIAN_POINT ( 'NONE',  ( 55.70494972787295751, 36.88242187608393152, 9.295050272127047819 ) ) ;
#4610 = CARTESIAN_POINT ( 'NONE',  ( 74.18017581364799184, 50.00000000000000000, -15.00000000000000000 ) ) ;
#4611 = CARTESIAN_POINT ( 'NONE',  ( 181.8548138422182205, 33.60820312608393579, 0.000000000000000000 ) ) ;
#4612 = ORIENTED_EDGE ( 'NONE', *, *, #18222, .T. ) ;
#4613 = VERTEX_POINT ( 'NONE', #5936 ) ;
#4614 = CARTESIAN_POINT ( 'NONE',  ( -13.14518615778179900, 40.70234375108393721, -5.444914386472297529 ) ) ;
#4615 = DIRECTION ( 'NONE',  ( 1.000000000000000000, 0.000000000000000000, 0.000000000000000000 ) ) ;
#4616 = CARTESIAN_POINT ( 'NONE',  ( 104.4587341249999781, 1.846868145590750521, 10.25000000136559031 ) ) ;
#4617 = EDGE_CURVE ( 'NONE', #5488, #4145, #15221, .T. ) ;
#4618 = CARTESIAN_POINT ( 'NONE',  ( 70.44491438647229131, 40.30546875108393579, -13.14518615778179722 ) ) ;
#4619 = CARTESIAN_POINT ( 'NONE',  ( 103.1528011352953342, 79.81250000136559208, 3.152801135295355106 ) ) ;
#4620 = CARTESIAN_POINT ( 'NONE',  ( 208.1451861577818079, 37.77539062608393294, -1.609821015232357215E-15 ) ) ;
#4621 = ADVANCED_FACE ( 'NONE', ( #20767, #8200 ), #6073, .F. ) ;
#4622 = CARTESIAN_POINT ( 'NONE',  ( 13.14518615778179544, 37.97382812608393721, -1.609821015232357215E-15 ) ) ;
#4623 = CARTESIAN_POINT ( 'NONE',  ( -9.598844408820458085, 39.41250000216787441, -9.598844408820458085 ) ) ;
#4624 = LINE ( 'NONE', #13281, #3478 ) ;
#4625 = CARTESIAN_POINT ( 'NONE',  ( 104.3262379212492590, 104.0454443415356991, -49.30000000000000426 ) ) ;
#4626 = CARTESIAN_POINT ( 'NONE',  ( 95.00472066334982912, 116.8754121666685393, -51.92499999726881299 ) ) ;
#4627 = EDGE_CURVE ( 'NONE', #11152, #4858, #10052, .T. ) ;
#4628 = ORIENTED_EDGE ( 'NONE', *, *, #9306, .T. ) ;
#4629 = CARTESIAN_POINT ( 'NONE',  ( -13.57481594606304753, 37.77539062499999289, -5.622872871577873077 ) ) ;
#4630 = CARTESIAN_POINT ( 'NONE',  ( 9.295050272127046043, 37.87460937608393152, -9.295050272127046043 ) ) ;
#4631 = EDGE_LOOP ( 'NONE', ( #23437, #20704, #27778, #22177 ) ) ;
#4632 = CARTESIAN_POINT ( 'NONE',  ( 135.4449143864723055, 37.32890625108393579, -13.14518615778179900 ) ) ;
#4633 = CARTESIAN_POINT ( 'NONE',  ( 74.29505027212704249, 35.29492187608393294, 9.295050272127046043 ) ) ;
#4634 = EDGE_CURVE ( 'NONE', #5134, #9259, #1528, .T. ) ;
#4635 = CARTESIAN_POINT ( 'NONE',  ( 204.2950502721270425, 36.48554687608393721, -9.295050272127046043 ) ) ;
#4636 = VERTEX_POINT ( 'NONE', #16891 ) ;
#4637 = FACE_OUTER_BOUND ( 'NONE', #3217, .T. ) ;
#4638 = CARTESIAN_POINT ( 'NONE',  ( -13.14518615778179544, 33.40976562608393863, 0.000000000000000000 ) ) ;
#4639 = CARTESIAN_POINT ( 'NONE',  ( 128.1078166429076646, 53.66387243068088964, -14.99999999999999822 ) ) ;
#4640 = CARTESIAN_POINT ( 'NONE',  ( 6.944426393311537993, 31.75150625057403175, -11.16113171639042356 ) ) ;
#4641 = CARTESIAN_POINT ( 'NONE',  ( 4.157286354961724939, 36.00000000000000000, -12.92256159328856135 ) ) ;
#4642 = DIRECTION ( 'NONE',  ( -0.000000000000000000, -1.000000000000000000, -0.000000000000000000 ) ) ;
#4643 =( BOUNDED_CURVE ( )  B_SPLINE_CURVE ( 2, ( #25666, #1884, #19390, #23813, #10408 ),
 .UNSPECIFIED., .F., .F. ) 
 B_SPLINE_CURVE_WITH_KNOTS ( ( 3, 2, 3 ),
 ( 0.4375000000000003331, 0.4479166666666667962, 0.4520580917964582834 ),
 .UNSPECIFIED. ) 
 CURVE ( )  GEOMETRIC_REPRESENTATION_ITEM ( )  RATIONAL_B_SPLINE_CURVE ( ( 0.9999999999999975575, 0.9238795325112891810, 1.000000000000000000, 0.9697362671728727568, 0.9635368512068458458 ) ) 
 REPRESENTATION_ITEM ( '' )  );
#4644 = CARTESIAN_POINT ( 'NONE',  ( 195.0000000000000000, 36.03906250000000000, -13.57481594606304576 ) ) ;
#4645 = CARTESIAN_POINT ( 'NONE',  ( 101.7677669529663547, 122.4000000021849530, -1.767766952966370209 ) ) ;
#4646 = CARTESIAN_POINT ( 'NONE',  ( 97.50000000000000000, 124.2000000000000028, -9.540979117872439019E-15 ) ) ;
#4647 = ORIENTED_EDGE ( 'NONE', *, *, #484, .T. ) ;
#4648 =( NAMED_UNIT ( * ) SI_UNIT ( $, .STERADIAN. ) SOLID_ANGLE_UNIT ( ) );
#4649 = CARTESIAN_POINT ( 'NONE',  ( 101.8468681455906903, -4.458734124999987891, 9.750000001365593860 ) ) ;
#4650 = ORIENTED_EDGE ( 'NONE', *, *, #15930, .T. ) ;
#4651 = CARTESIAN_POINT ( 'NONE',  ( 101.7677669529663547, 122.4000000021849530, -1.767766952966370209 ) ) ;
#4652 = CARTESIAN_POINT ( 'NONE',  ( 98.15313185440925281, 4.458734125000016313, 11.25000000136559031 ) ) ;
#4653 = CARTESIAN_POINT ( 'NONE',  ( 104.9999999999999574, 2.071067811865501263, 8.562499999999998224 ) ) ;
#4654 = CARTESIAN_POINT ( 'NONE',  ( 13.14518615778179900, 37.82500000108392868, -5.444914386472297529 ) ) ;
#4655 = CARTESIAN_POINT ( 'NONE',  ( 116.4251840539369596, 38.66835937716787441, -5.622872871577872189 ) ) ;
#4656 = FACE_OUTER_BOUND ( 'NONE', #27530, .T. ) ;
#4657 = CARTESIAN_POINT ( 'NONE',  ( 65.00000000000000000, 35.79101562608394005, -13.14518615778179544 ) ) ;
#4658 = CARTESIAN_POINT ( 'NONE',  ( 102.4976396683250925, 117.6869444889999841, -53.72500000273119980 ) ) ;
#4659 = CARTESIAN_POINT ( 'NONE',  ( -9.295050272127044266, 36.68398437608392726, 9.295050272127047819 ) ) ;
#4660 = CARTESIAN_POINT ( 'NONE',  ( -9.598844408820458085, 39.31328124999999574, -9.598844408820458085 ) ) ;
#4661 = DIRECTION ( 'NONE',  ( -0.000000000000000000, 1.000000000000000000, -0.000000000000000000 ) ) ;
#4662 = CARTESIAN_POINT ( 'NONE',  ( 102.1631189606246295, 103.3426043859339103, -55.89999999453763735 ) ) ;
#4663 = CARTESIAN_POINT ( 'NONE',  ( 143.5748159460630404, 38.17226562499999432, 5.622872871577869525 ) ) ;
#4664 = ORIENTED_EDGE ( 'NONE', *, *, #1327, .T. ) ;
#4665 = ADVANCED_FACE ( 'NONE', ( #1802 ), #25589, .T. ) ;
#4666 = VERTEX_POINT ( 'NONE', #16755 ) ;
#4667 = CARTESIAN_POINT ( 'NONE',  ( 219.9999999999999716, 50.00000000000000000, -10.00000000000000000 ) ) ;
#4668 = CARTESIAN_POINT ( 'NONE',  ( 2.414731522848535132E-15, 36.18789062608393436, 13.14518615778179544 ) ) ;
#4669 = CARTESIAN_POINT ( 'NONE',  ( 13.57481594606304931, 35.89023437716787868, 5.622872871577869525 ) ) ;
#4670 = CARTESIAN_POINT ( 'NONE',  ( 97.92893218813451028, 5.000000000000018652, 9.937500002731184168 ) ) ;
#4671 = CARTESIAN_POINT ( 'NONE',  ( 116.8548138422182205, 38.17226562608393436, 0.000000000000000000 ) ) ;
#4672 = CARTESIAN_POINT ( 'NONE',  ( 70.62287287157786864, 35.29492187716788720, -13.57481594606304753 ) ) ;
#4673 = ORIENTED_EDGE ( 'NONE', *, *, #24988, .F. ) ;
#4674 = CARTESIAN_POINT ( 'NONE',  ( 13.40642364673445819, 36.00000000000001421, 1.227293221035465454 ) ) ;
#4675 = CARTESIAN_POINT ( 'NONE',  ( -9.598844408820454532, 34.05468750216788010, 9.598844408820459861 ) ) ;
#4676 = CARTESIAN_POINT ( 'NONE',  ( 99.99999999999998579, 124.1000000021849416, -2.499999999999997780 ) ) ;
#4677 = CARTESIAN_POINT ( 'NONE',  ( 97.50236033167490746, 117.6869444889999841, -48.27499999726882152 ) ) ;
#4678 = CARTESIAN_POINT ( 'NONE',  ( 208.1451861577817795, 33.85625000108393579, -5.444914386472297529 ) ) ;
#4679 = CYLINDRICAL_SURFACE ( 'NONE', #11062, 13.57481594606304398 ) ;
#4680 = VECTOR ( 'NONE', #7226, 1000.000000000000000 ) ;
#4681 = CARTESIAN_POINT ( 'NONE',  ( 143.1451861577818363, 36.23750000108393010, -5.444914386472297529 ) ) ;
#4683 = EDGE_LOOP ( 'NONE', ( #3093, #27484, #23816, #13395, #7616, #6409, #19558, #3230, #10808, #14475, #6143, #20661, #26578, #15872, #10954, #10552, #12434, #22524, #24367, #1816, #14565, #11686, #25757, #16477, #5639, #937, #20308 ) ) ;
#4682 = CARTESIAN_POINT ( 'NONE',  ( 181.4251840539369596, 40.20624999999999005, 0.000000000000000000 ) ) ;
#4684 = CARTESIAN_POINT ( 'NONE',  ( 214.9999999999999716, 75.00000000000000000, 9.999999999999946709 ) ) ;
#4685 = CARTESIAN_POINT ( 'NONE',  ( 208.5748159460630688, 39.16445312716788152, -5.622872871577873966 ) ) ;
#4686 = CARTESIAN_POINT ( 'NONE',  ( -8.312177448680279460E-16, 36.83281249999999574, -13.57481594606304576 ) ) ;
#4687 = CARTESIAN_POINT ( 'NONE',  ( 102.1631189606246295, 116.6573956140660897, -54.60000000000000853 ) ) ;
#4688 = CARTESIAN_POINT ( 'NONE',  ( -9.295050272127044266, 38.46992187608393721, 9.295050272127047819 ) ) ;
#4689 = CARTESIAN_POINT ( 'NONE',  ( 9.295050272127047819, 35.29492187608393294, 9.295050272127046043 ) ) ;
#4690 = CARTESIAN_POINT ( 'NONE',  ( 208.5748159460630120, 34.20351562499999432, 5.622872871577869525 ) ) ;
#4691 = ITEM_DEFINED_TRANSFORMATION ( 'NONE', 'NONE', #10367,  #26844 ) ;
#4692 = CARTESIAN_POINT ( 'NONE',  ( 51.42518405393695957, 40.25585937499999289, 5.622872871577880183 ) ) ;
#4693 = CARTESIAN_POINT ( 'NONE',  ( 78.14518615778179367, 35.44375000108393436, -5.444914386472297529 ) ) ;
#4694 = CARTESIAN_POINT ( 'NONE',  ( 103.1528011352953342, -3.152801135295355106, 2.812500001365592528 ) ) ;
#4695 = CARTESIAN_POINT ( 'NONE',  ( 98.57518772780328220, 123.0000000000000284, -2.059818896815785561 ) ) ;
#4696 = ORIENTED_EDGE ( 'NONE', *, *, #20337, .T. ) ;
#4697 = DIRECTION ( 'NONE',  ( 0.000000000000000000, 0.000000000000000000, -1.000000000000000000 ) ) ;
#4698 = CARTESIAN_POINT ( 'NONE',  ( -9.598844408820458085, 36.13828124999999147, -9.598844408820458085 ) ) ;
#4699 = CARTESIAN_POINT ( 'NONE',  ( 116.8548138422182063, 38.32109375108394289, -5.444914386472297529 ) ) ;
#4700 = EDGE_LOOP ( 'NONE', ( #16748, #15031, #19357, #25768 ) ) ;
#4701 = CARTESIAN_POINT ( 'NONE',  ( 101.8468681455906903, 81.00000000136560629, 4.458734124999987891 ) ) ;
#4702 = CARTESIAN_POINT ( 'NONE',  ( 100.0000000000000000, 110.0000000000000000, -55.00000000000000711 ) ) ;
#4703 = CARTESIAN_POINT ( 'NONE',  ( 94.99999999999995737, 82.18750000273121259, 2.071067811865466624 ) ) ;
#4704 = CARTESIAN_POINT ( 'NONE',  ( 99.99999999999998579, 93.56249999863440792, -4.458734124999994997 ) ) ;
#4705 = CARTESIAN_POINT ( 'NONE',  ( 69.15728635496172672, 36.00000000000000000, -12.92256159328856135 ) ) ;
#4706 = CIRCLE ( 'NONE', #1519, 15.57481594606304576 ) ;
#4707 = CARTESIAN_POINT ( 'NONE',  ( 102.1631189606246295, 103.3426043859339103, -52.40000000000001279 ) ) ;
#4708 = CARTESIAN_POINT ( 'NONE',  ( 78.57481594606305464, 39.80937499999999574, -1.662435489736055892E-15 ) ) ;
#4709 = VERTEX_POINT ( 'NONE', #16621 ) ;
#4710 = CARTESIAN_POINT ( 'NONE',  ( 99.99999999999998579, 95.62499999726881583, 4.999999999999984013 ) ) ;
#4711 = CARTESIAN_POINT ( 'NONE',  ( 102.0710678118654329, 5.000000000000018652, 11.68750000000000000 ) ) ;
#4712 = ORIENTED_EDGE ( 'NONE', *, *, #3607, .F. ) ;
#4713 = CARTESIAN_POINT ( 'NONE',  ( -8.049105076161786076E-16, 31.82226562608393650, -13.14518615778179544 ) ) ;
#4714 = CARTESIAN_POINT ( 'NONE',  ( 13.14518615778179900, 38.81718750108393579, -5.444914386472297529 ) ) ;
#4715 = UNCERTAINTY_MEASURE_WITH_UNIT (LENGTH_MEASURE( 1.000000000000000082E-05 ), #4934, 'distance_accuracy_value', 'NONE');
#4716 = CARTESIAN_POINT ( 'NONE',  ( 208.5748159460630120, 33.50898437716787015, 5.622872871577869525 ) ) ;
#4717 = ORIENTED_EDGE ( 'NONE', *, *, #9121, .F. ) ;
#4718 = CARTESIAN_POINT ( 'NONE',  ( -13.14518615778179544, 36.58476562608393579, 0.000000000000000000 ) ) ;
#4719 = DIRECTION ( 'NONE',  ( -1.000000000000000000, -0.000000000000000000, -0.000000000000000000 ) ) ;
#4720 = CARTESIAN_POINT ( 'NONE',  ( 139.2950502721270425, 36.48554687608393721, -9.295050272127046043 ) ) ;
#4721 = CARTESIAN_POINT ( 'NONE',  ( -5.444914386472297529, 34.25312500108393010, -13.14518615778179900 ) ) ;
#4722 = CARTESIAN_POINT ( 'NONE',  ( 139.2950502721270425, 33.90585937608393152, -9.295050272127046043 ) ) ;
#4723 = CARTESIAN_POINT ( 'NONE',  ( 65.00000000000000000, 36.03906250000000000, -13.57481594606304576 ) ) ;
#4724 = CARTESIAN_POINT ( 'NONE',  ( 99.14382582708707048, 124.6000000010924822, -2.066987299999999195 ) ) ;
#4725 = CARTESIAN_POINT ( 'NONE',  ( 104.4587341249999639, 1.442382525525748735E-14, 11.18750000136559208 ) ) ;
#4727 = FACE_OUTER_BOUND ( 'NONE', #13614, .T. ) ;
#4726 = VECTOR ( 'NONE', #8630, 1000.000000000000000 ) ;
#4728 = CARTESIAN_POINT ( 'NONE',  ( 95.54126587499996504, 1.846868145590750077, 12.37500000136559208 ) ) ;
#4729 = CARTESIAN_POINT ( 'NONE',  ( 106.5389055433251002, 114.7507929638356785, -47.92500000273120264 ) ) ;
#4730 = CARTESIAN_POINT ( 'NONE',  ( 99.99999999999995737, 80.00000000000000000, -1.387778780781445676E-14 ) ) ;
#4731 = CARTESIAN_POINT ( 'NONE',  ( 99.99999999999995737, 83.87500000273119838, -5.000000000000018652 ) ) ;
#4732 = CARTESIAN_POINT ( 'NONE',  ( 93.46109445667489979, 114.7507929638356785, -49.82499999726882578 ) ) ;
#4733 = CARTESIAN_POINT ( 'NONE',  ( 13.14518615778179900, 35.64218750108393152, -5.444914386472297529 ) ) ;
#4734 = CARTESIAN_POINT ( 'NONE',  ( 102.4976396683250783, 117.6869444889999841, -52.47499999726882436 ) ) ;
#4735 = EDGE_LOOP ( 'NONE', ( #23153, #27580, #17982, #2378 ) ) ;
#4736 = CARTESIAN_POINT ( 'NONE',  ( 97.93301270000000613, 124.7000000010924765, -0.8561741729129506151 ) ) ;
#4737 =( BOUNDED_CURVE ( )  B_SPLINE_CURVE ( 2, ( #5623, #6037, #14703, #27703, #27422, #18587, #23287, #27292, #12556 ),
 .UNSPECIFIED., .F., .F. ) 
 B_SPLINE_CURVE_WITH_KNOTS ( ( 3, 2, 2, 2, 3 ),
 ( 0.6500000000000005773, 0.6750000000000005995, 0.7000000000000006217, 0.7250000000000006439, 0.7500000000000006661 ),
 .UNSPECIFIED. ) 
 CURVE ( )  GEOMETRIC_REPRESENTATION_ITEM ( )  RATIONAL_B_SPLINE_CURVE ( ( 0.9999999999999983347, 0.9238795325112884038, 1.000000000000000000, 0.9238795325112867385, 1.000000000000000000, 0.9238795325112867385, 1.000000000000000000, 0.9238795325112847401, 1.000000000000001998 ) ) 
 REPRESENTATION_ITEM ( '' )  );
#4738 = CARTESIAN_POINT ( 'NONE',  ( 102.0710678118654329, -4.999999999999989342, 12.43750000273118950 ) ) ;
#4739 = LINE ( 'NONE', #2460, #20699 ) ;
#4740 = CARTESIAN_POINT ( 'NONE',  ( 204.2950502721270425, 35.49335937608393010, -9.295050272127046043 ) ) ;
#4741 = VERTEX_POINT ( 'NONE', #12324 ) ;
#4742 = CARTESIAN_POINT ( 'NONE',  ( 2.493653234604083739E-15, 32.46718749999999432, 13.57481594606304576 ) ) ;
#4743 = CARTESIAN_POINT ( 'NONE',  ( 135.6228728715777549, 39.66054687500000142, 13.57481594606318076 ) ) ;
#4744 = EDGE_CURVE ( 'NONE', #18339, #13739, #10180, .T. ) ;
#4745 = ORIENTED_EDGE ( 'NONE', *, *, #2536, .F. ) ;
#4746 = CARTESIAN_POINT ( 'NONE',  ( 97.50236033167492167, 102.3130555110000159, -50.97500000273119980 ) ) ;
#4747 = CARTESIAN_POINT ( 'NONE',  ( 13.14518615778179544, 38.56914062608393579, -1.609821015232357215E-15 ) ) ;
#4748 = CARTESIAN_POINT ( 'NONE',  ( 97.50000000000000000, 123.3499999999999943, -1.035533905932742416 ) ) ;
#4749 = CARTESIAN_POINT ( 'NONE',  ( 130.0000000000000000, 32.16953125216787157, -13.57481594606304576 ) ) ;
#4750 = DIRECTION ( 'NONE',  ( -0.000000000000000000, -1.000000000000000000, -0.000000000000000000 ) ) ;
#4751 = ORIENTED_EDGE ( 'NONE', *, *, #11675, .T. ) ;
#4752 = CARTESIAN_POINT ( 'NONE',  ( 104.9999999999999858, 93.87499999726881583, -6.938893903907228378E-15 ) ) ;
#4753 = CARTESIAN_POINT ( 'NONE',  ( 55.70494972787295751, 37.47773437608393010, -9.295050272127046043 ) ) ;
#4754 = CARTESIAN_POINT ( 'NONE',  ( 58.12649175642295063, 51.14166184781131363, -15.00000000000130917 ) ) ;
#4755 = CARTESIAN_POINT ( 'NONE',  ( 200.6228728715778686, 39.66054687500000142, 13.57481594606304576 ) ) ;
#4756 = DIRECTION ( 'NONE',  ( -0.000000000000000000, 1.000000000000000000, 0.000000000000000000 ) ) ;
#4757 = ORIENTED_EDGE ( 'NONE', *, *, #3586, .F. ) ;
#4758 = ORIENTED_EDGE ( 'NONE', *, *, #25461, .T. ) ;
#4759 = CARTESIAN_POINT ( 'NONE',  ( 5.444914386472302859, 35.44375000108393436, 13.14518615778179189 ) ) ;
#4760 = CARTESIAN_POINT ( 'NONE',  ( 95.54126587499996504, 1.387778780781445676E-14, 12.68750000136559208 ) ) ;
#4761 = CARTESIAN_POINT ( 'NONE',  ( 55.70494972787295751, 36.68398437608392726, 9.295050272127047819 ) ) ;
#4762 = CARTESIAN_POINT ( 'NONE',  ( 104.9999999999999716, 90.93749999726880162, -2.071067811865478170 ) ) ;
#4763 = CARTESIAN_POINT ( 'NONE',  ( 189.5550856135277229, 39.11484375108393863, 13.14518615778179722 ) ) ;
#4764 = CARTESIAN_POINT ( 'NONE',  ( -13.14518615778179189, 36.83281250108393579, 5.444914386472304635 ) ) ;
#4765 = CARTESIAN_POINT ( 'NONE',  ( 104.4587341249999781, 91.56249999863440792, -6.938893903907228378E-15 ) ) ;
#4766 = CARTESIAN_POINT ( 'NONE',  ( 208.1451861577818079, 38.76757812608393294, -1.609821015232357215E-15 ) ) ;
#4767 = CARTESIAN_POINT ( 'NONE',  ( 97.50236033167490746, 102.3130555110000159, -51.22499999726882436 ) ) ;
#4768 = ORIENTED_EDGE ( 'NONE', *, *, #13826, .T. ) ;
#4769 = EDGE_CURVE ( 'NONE', #15330, #13131, #27478, .T. ) ;
#4770 = AXIS2_PLACEMENT_3D ( 'NONE', #19877, #26300, #15445 ) ;
#4771 = CARTESIAN_POINT ( 'NONE',  ( 9.598844408820456309, 35.14609374999999858, -9.598844408820458085 ) ) ;
#4772 = CARTESIAN_POINT ( 'NONE',  ( -9.295050272127044266, 38.27148437608393294, 9.295050272127047819 ) ) ;
#4773 = ORIENTED_EDGE ( 'NONE', *, *, #368, .T. ) ;
#4774 = CARTESIAN_POINT ( 'NONE',  ( 124.5550856135277087, 34.55078125108393294, 13.14518615778179722 ) ) ;
#4775 = CARTESIAN_POINT ( 'NONE',  ( 65.00000000000000000, 34.00507812608393721, -13.14518615778179544 ) ) ;
#4776 = CARTESIAN_POINT ( 'NONE',  ( 208.1451861577817795, 37.92421875108392726, 5.444914386472293977 ) ) ;
#4777 =( BOUNDED_CURVE ( )  B_SPLINE_CURVE ( 2, ( #12305, #25574, #1509, #18745, #21161, #18873, #17007, #8043, #16601 ),
 .UNSPECIFIED., .F., .F. ) 
 B_SPLINE_CURVE_WITH_KNOTS ( ( 3, 2, 2, 2, 3 ),
 ( 0.6874999999999997780, 0.6979166666666665186, 0.7083333333333333703, 0.7187500000000001110, 0.7291666666666668517 ),
 .UNSPECIFIED. ) 
 CURVE ( )  GEOMETRIC_REPRESENTATION_ITEM ( )  RATIONAL_B_SPLINE_CURVE ( ( 1.000000000000001554, 0.9238795325112850731, 1.000000000000000000, 0.9238795325112867385, 1.000000000000000000, 0.9238795325112867385, 1.000000000000000000, 0.9238795325112850731, 1.000000000000001554 ) ) 
 REPRESENTATION_ITEM ( '' )  );
#4778 = ORIENTED_EDGE ( 'NONE', *, *, #12329, .T. ) ;
#4779 = CARTESIAN_POINT ( 'NONE',  ( 98.24769277278620905, 123.0259891538152743, 1.170854245699148866 ) ) ;
#4780 = CARTESIAN_POINT ( 'NONE',  ( 13.14518615778179544, 33.80664062608393294, -1.609821015232357215E-15 ) ) ;
#4781 = CARTESIAN_POINT ( 'NONE',  ( 102.4999999999999858, 123.9500000021849502, -1.035533905932742638 ) ) ;
#4782 = EDGE_CURVE ( 'NONE', #9459, #3810, #28017, .T. ) ;
#4783 = CARTESIAN_POINT ( 'NONE',  ( 195.0000000000000000, 36.13828125216787157, -13.57481594606304576 ) ) ;
#4784 = CARTESIAN_POINT ( 'NONE',  ( 1.662435489736055892E-15, 40.99999999999999289, 13.57481594606304576 ) ) ;
#4785 = EDGE_CURVE ( 'NONE', #13739, #24582, #9050, .T. ) ;
#4786 = DIRECTION ( 'NONE',  ( 0.000000000000000000, 1.000000000000000000, 0.000000000000000000 ) ) ;
#4787 = CARTESIAN_POINT ( 'NONE',  ( -8.312177448680279460E-16, 36.83281249999999574, -13.57481594606304576 ) ) ;
#4788 = CARTESIAN_POINT ( 'NONE',  ( 195.0000000000000000, 39.75976562608394005, -13.14518615778179544 ) ) ;
#4789 = VECTOR ( 'NONE', #16854, 1000.000000000000000 ) ;
#4790 = VERTEX_POINT ( 'NONE', #21600 ) ;
#4791 = CARTESIAN_POINT ( 'NONE',  ( 101.8468681455906903, -4.458734124999987891, 4.750000001365592084 ) ) ;
#4792 = ORIENTED_EDGE ( 'NONE', *, *, #10643, .T. ) ;
#4793 = CARTESIAN_POINT ( 'NONE',  ( 97.93301270000000613, 122.9500000010924765, -9.540979117872439019E-15 ) ) ;
#4794 = CARTESIAN_POINT ( 'NONE',  ( 104.4587341249999639, 1.442382525525748735E-14, 9.937500001365592084 ) ) ;
#4795 = CARTESIAN_POINT ( 'NONE',  ( 128.0526740779191073, 51.47162402671428794, 14.99999999999996803 ) ) ;
#4796 = EDGE_CURVE ( 'NONE', #923, #7889, #3573, .T. ) ;
#4797 = CARTESIAN_POINT ( 'NONE',  ( 13.14518615778179900, 34.65000000108393152, -5.444914386472297529 ) ) ;
#4798 = CARTESIAN_POINT ( 'NONE',  ( 9.598844408820459861, 32.56640625000000000, 9.598844408820456309 ) ) ;
#4799 = CARTESIAN_POINT ( 'NONE',  ( 101.8468681455906903, 83.00000000136559208, 4.458734124999987891 ) ) ;
#4800 = CARTESIAN_POINT ( 'NONE',  ( 51.85481384221820633, 36.03906250108394005, 5.444914386472304635 ) ) ;
#4801 = CARTESIAN_POINT ( 'NONE',  ( 185.4011555911795597, 37.92421874999999432, 9.598844408820459861 ) ) ;
#4802 = CARTESIAN_POINT ( 'NONE',  ( 5.444914386472302859, 39.21406250108392300, 13.14518615778179189 ) ) ;
#4803 = VECTOR ( 'NONE', #27473, 1000.000000000000000 ) ;
#4804 = CARTESIAN_POINT ( 'NONE',  ( 103.5355339059327093, 80.50000000273119838, 3.535533905932726206 ) ) ;
#4805 = CARTESIAN_POINT ( 'NONE',  ( 104.9999999999999716, 1.449011120738813565E-14, 11.62500000273118417 ) ) ;
#4806 = CARTESIAN_POINT ( 'NONE',  ( 99.99999999999998579, 136.0000000000000000, -5.204170427930421283E-15 ) ) ;
#4807 = CARTESIAN_POINT ( 'NONE',  ( 143.5748159460630688, 38.22187499999999716, -1.662435489736055892E-15 ) ) ;
#4808 = ORIENTED_EDGE ( 'NONE', *, *, #4442, .T. ) ;
#4809 = CARTESIAN_POINT ( 'NONE',  ( 105.6631189606246153, 114.1144967660473242, -51.80000000000001137 ) ) ;
#4810 = CARTESIAN_POINT ( 'NONE',  ( 13.14518615778179544, 35.59257812608393579, -1.609821015232357215E-15 ) ) ;
#4811 = CARTESIAN_POINT ( 'NONE',  ( -5.622872871577873077, 38.86679687716788578, 13.57481594606304753 ) ) ;
#4812 = CARTESIAN_POINT ( 'NONE',  ( 102.0710678118654329, -4.999999999999989342, 9.437500002731182391 ) ) ;
#4813 = CARTESIAN_POINT ( 'NONE',  ( 139.2950502721270425, 32.31835937608393294, -9.295050272127046043 ) ) ;
#4814 = CARTESIAN_POINT ( 'NONE',  ( 74.59884440882045453, 32.86406250216787583, -9.598844408820458085 ) ) ;
#4815 = ADVANCED_FACE ( 'NONE', ( #10609 ), #2078, .F. ) ;
#4816 = VERTEX_POINT ( 'NONE', #6762 ) ;
#4817 = AXIS2_PLACEMENT_3D ( 'NONE', #25573, #21160, #14722 ) ;
#4818 = CARTESIAN_POINT ( 'NONE',  ( 7.065634988761035906, 35.99999999999999289, 11.21307450592191124 ) ) ;
#4819 = CARTESIAN_POINT ( 'NONE',  ( 5.622872871577871301, 32.11992187716787583, -13.57481594606304753 ) ) ;
#4820 =( BOUNDED_CURVE ( )  B_SPLINE_CURVE ( 2, ( #1806, #10056, #1533, #18767, #1944, #1395, #27882, #23599, #3667 ),
 .UNSPECIFIED., .F., .F. ) 
 B_SPLINE_CURVE_WITH_KNOTS ( ( 3, 2, 2, 2, 3 ),
 ( 0.5500000000000004885, 0.5750000000000003997, 0.6000000000000005329, 0.6250000000000005551, 0.6500000000000005773 ),
 .UNSPECIFIED. ) 
 CURVE ( )  GEOMETRIC_REPRESENTATION_ITEM ( )  RATIONAL_B_SPLINE_CURVE ( ( 0.9999999999999986677, 0.9238795325112880708, 1.000000000000000000, 0.9238795325112867385, 1.000000000000000000, 0.9238795325112867385, 1.000000000000000000, 0.9238795325112850731, 1.000000000000001776 ) ) 
 REPRESENTATION_ITEM ( '' )  );
#4821 = CARTESIAN_POINT ( 'NONE',  ( 65.00000000000000000, 38.02343749999999289, 13.57481594606304576 ) ) ;
#4822 = CARTESIAN_POINT ( 'NONE',  ( 95.00472066334981491, 116.8754121666685393, -50.17499999726882010 ) ) ;
#4823 = CARTESIAN_POINT ( 'NONE',  ( -9.598844408820458085, 37.82500000216787583, -9.598844408820458085 ) ) ;
#4824 = CARTESIAN_POINT ( 'NONE',  ( 195.0000000000000000, 33.21132812608393436, -13.14518615778179544 ) ) ;
#4825 = AXIS2_PLACEMENT_3D ( 'NONE', #13822, #19094, #10386 ) ;
#4826 = CARTESIAN_POINT ( 'NONE',  ( 217.9999999999999716, 80.00000000000000000, 12.99999999999994316 ) ) ;
#4827 = LINE ( 'NONE', #23679, #11706 ) ;
#4828 = ADVANCED_FACE ( 'NONE', ( #17742 ), #11162, .F. ) ;
#4829 = CARTESIAN_POINT ( 'NONE',  ( 99.99999999999995737, 81.25000000000000000, 4.999999999999990230 ) ) ;
#4830 = CARTESIAN_POINT ( 'NONE',  ( 99.99999999999998579, 94.12499999726881583, -4.999999999999997335 ) ) ;
#4831 = CYLINDRICAL_SURFACE ( 'NONE', #4506, 13.57481594606304576 ) ;
#4832 = CARTESIAN_POINT ( 'NONE',  ( 208.5748159460630688, 36.68398437500000142, -5.622872871577873966 ) ) ;
#4833 = CARTESIAN_POINT ( 'NONE',  ( 9.598844408820459861, 36.53515624999999289, 9.598844408820456309 ) ) ;
#4834 = DIRECTION ( 'NONE',  ( -0.000000000000000000, 1.000000000000000000, -0.000000000000000000 ) ) ;
#4835 = CARTESIAN_POINT ( 'NONE',  ( 5.444914386472297529, 33.36015625108393579, -13.14518615778179900 ) ) ;
#4836 = CARTESIAN_POINT ( 'NONE',  ( -13.14518615778179544, 35.79101562608393294, 0.000000000000000000 ) ) ;
#4837 = CARTESIAN_POINT ( 'NONE',  ( 204.5988444088204403, 33.55859375000000000, -9.598844408820458085 ) ) ;
#4838 = CARTESIAN_POINT ( 'NONE',  ( 5.622872871577878406, 36.58476562716787583, 13.57481594606304576 ) ) ;
#4839 = DIRECTION ( 'NONE',  ( 0.000000000000000000, -1.000000000000000000, 0.000000000000000000 ) ) ;
#4840 = DIRECTION ( 'NONE',  ( 1.000000000000000000, 0.000000000000000000, 0.000000000000000000 ) ) ;
#4841 = CARTESIAN_POINT ( 'NONE',  ( 51.85481384221820633, 36.63437500108393152, 5.444914386472304635 ) ) ;
#4842 = CARTESIAN_POINT ( 'NONE',  ( 95.54126587499996504, 1.846868145590750077, 2.375000001365592084 ) ) ;
#4843 = CARTESIAN_POINT ( 'NONE',  ( 99.91426332765584561, 123.0000000000000142, -2.514867278806395490 ) ) ;
#4844 = CARTESIAN_POINT ( 'NONE',  ( 9.598844408820459861, 37.32890624999999574, 9.598844408820456309 ) ) ;
#4845 = CARTESIAN_POINT ( 'NONE',  ( 139.2950502721270425, 38.07304687608393579, -9.295050272127046043 ) ) ;
#4846 = ORIENTED_EDGE ( 'NONE', *, *, #11204, .T. ) ;
#4847 = DIRECTION ( 'NONE',  ( 0.8660254037844407060, 0.4999999999999963363, 0.000000000000000000 ) ) ;
#4848 = CARTESIAN_POINT ( 'NONE',  ( 98.54104284345754650, 123.0000000000000426, 1.608754092638752242 ) ) ;
#4849 = CARTESIAN_POINT ( 'NONE',  ( 102.0710678118654329, 81.43750000273121259, 4.999999999999989342 ) ) ;
#4850 = CARTESIAN_POINT ( 'NONE',  ( 99.99999999999998579, 94.56249999863440792, -4.458734124999994997 ) ) ;
#4851 = CARTESIAN_POINT ( 'NONE',  ( 68.08926091379791501, 35.99999999999998579, -13.21136010216353540 ) ) ;
#4852 = CARTESIAN_POINT ( 'NONE',  ( 107.0000000000000000, 110.0000000000000000, -48.00000000000001421 ) ) ;
#4853 = CARTESIAN_POINT ( 'NONE',  ( 74.59884440882045453, 40.50390624999999289, 9.598844408820456309 ) ) ;
#4854 = EDGE_LOOP ( 'NONE', ( #25979, #27722, #23942, #15444 ) ) ;
#4855 = FACE_OUTER_BOUND ( 'NONE', #14463, .T. ) ;
#4856 = CARTESIAN_POINT ( 'NONE',  ( 96.46446609406721961, 3.535533905932755072, 12.87500000000000000 ) ) ;
#4857 = ADVANCED_FACE ( 'NONE', ( #2365 ), #23885, .T. ) ;
#4858 = VERTEX_POINT ( 'NONE', #4353 ) ;
#4859 = CARTESIAN_POINT ( 'NONE',  ( 13.14518615778179544, 37.18007812608393436, -1.609821015232357215E-15 ) ) ;
#4860 = CARTESIAN_POINT ( 'NONE',  ( 181.4251840539369596, 34.79882812716787299, 5.622872871577880183 ) ) ;
#4861 = CIRCLE ( 'NONE', #10749, 5.000000000000004441 ) ;
#4862 = ORIENTED_EDGE ( 'NONE', *, *, #6865, .F. ) ;
#4863 = CARTESIAN_POINT ( 'NONE',  ( -9.295050272127044266, 33.50898437608393010, 9.295050272127047819 ) ) ;
#4864 = CARTESIAN_POINT ( 'NONE',  ( -13.57481594606304753, 32.21914062499999432, -5.622872871577872189 ) ) ;
#4865 = CARTESIAN_POINT ( 'NONE',  ( 116.8548138422182205, 36.73359375108393010, -5.444914386472297529 ) ) ;
#4866 = EDGE_LOOP ( 'NONE', ( #20799, #4696, #17094, #281 ) ) ;
#4867 = CARTESIAN_POINT ( 'NONE',  ( -9.295050272127046043, 34.30273437608393294, -9.295050272127046043 ) ) ;
#4868 = CARTESIAN_POINT ( 'NONE',  ( 124.5550856135277087, 33.26093750108393721, -13.14518615778179900 ) ) ;
#4869 = CARTESIAN_POINT ( 'NONE',  ( 51.42518405393695957, 36.18789062499999432, -5.622872871577873077 ) ) ;
#4870 = AXIS2_PLACEMENT_3D ( 'NONE', #16199, #16481, #27470 ) ;
#4871 = DIRECTION ( 'NONE',  ( 0.000000000000000000, 0.000000000000000000, 1.000000000000000000 ) ) ;
#4872 = CARTESIAN_POINT ( 'NONE',  ( 95.54126587499996504, 1.387778780781445676E-14, 11.68750000136559208 ) ) ;
#4873 = CYLINDRICAL_SURFACE ( 'NONE', #321, 5.000000000000004441 ) ;
#4874 = CARTESIAN_POINT ( 'NONE',  ( 96.84719886470459471, -3.152801135295355994, 1.562500001365591418 ) ) ;
#4875 = CARTESIAN_POINT ( 'NONE',  ( 106.5389055433251002, 105.2492070361643215, -44.32500000273119412 ) ) ;
#4876 = FACE_OUTER_BOUND ( 'NONE', #23451, .T. ) ;
#4877 = CARTESIAN_POINT ( 'NONE',  ( 99.99999999999995737, 1.387778780781445676E-14, 34.79898987322334136 ) ) ;
#4878 = CARTESIAN_POINT ( 'NONE',  ( 106.5389055433250860, 114.7507929638356785, -50.42499999726882010 ) ) ;
#4879 = CARTESIAN_POINT ( 'NONE',  ( 2.414731522848535132E-15, 37.77539062608393294, 13.14518615778179544 ) ) ;
#4880 = CARTESIAN_POINT ( 'NONE',  ( 95.00472066334982912, 103.1245878333314323, -55.57499999726881157 ) ) ;
#4881 = EDGE_LOOP ( 'NONE', ( #7112, #20946, #1430, #23796, #19657, #22088 ) ) ;
#4882 = CARTESIAN_POINT ( 'NONE',  ( 97.93301270000000613, 124.0000000010924879, 0.8561741729129328515 ) ) ;
#4883 = VECTOR ( 'NONE', #14865, 1000.000000000000114 ) ;
#4884 = CARTESIAN_POINT ( 'NONE',  ( 0.000000000000000000, 36.00000000000000000, 0.000000000000000000 ) ) ;
#4885 = CARTESIAN_POINT ( 'NONE',  ( 99.99999999999998579, 123.3000000021849587, -2.499999999999997780 ) ) ;
#4886 = CARTESIAN_POINT ( 'NONE',  ( 195.0000000000000000, 37.18007812608393436, -13.14518615778179544 ) ) ;
#4887 = VERTEX_POINT ( 'NONE', #4077 ) ;
#4888 = CARTESIAN_POINT ( 'NONE',  ( 196.6052718765765803, 53.60388944777320575, -15.00000000000000000 ) ) ;
#4889 = CARTESIAN_POINT ( 'NONE',  ( 103.1528011352953342, 3.152801135295383084, 9.312500001365593860 ) ) ;
#4890 = EDGE_LOOP ( 'NONE', ( #19676, #17943 ) ) ;
#4891 = CARTESIAN_POINT ( 'NONE',  ( 108.0825317500000011, 107.3738262389971538, -52.47500000273118559 ) ) ;
#4892 = CARTESIAN_POINT ( 'NONE',  ( -13.14518615778179900, 35.74140625108393721, -5.444914386472297529 ) ) ;
#4893 = CARTESIAN_POINT ( 'NONE',  ( 102.0669872999999797, 122.7500000010924737, -9.794112055954760458E-15 ) ) ;
#4894 = CARTESIAN_POINT ( 'NONE',  ( 116.8548138422182063, 39.71015625108393010, -5.444914386472297529 ) ) ;
#4895 = CARTESIAN_POINT ( 'NONE',  ( 1.662435489736055498E-15, -7.395377635281828788, -13.57481594606304398 ) ) ;
#4896 = CARTESIAN_POINT ( 'NONE',  ( -13.14518615778179189, 35.84062500108394289, 5.444914386472304635 ) ) ;
#4897 = CARTESIAN_POINT ( 'NONE',  ( 99.99999999999998579, 94.12499999726881583, -4.999999999999997335 ) ) ;
#4898 = VECTOR ( 'NONE', #27472, 1000.000000000000000 ) ;
#4899 = CARTESIAN_POINT ( 'NONE',  ( 70.44491438647230552, 38.61875000108393152, 13.14518615778179189 ) ) ;
#4900 = AXIS2_PLACEMENT_3D ( 'NONE', #13801, #26807, #14470 ) ;
#4901 = CARTESIAN_POINT ( 'NONE',  ( 56.23061032792084291, 50.37710889401579806, -14.99999999999737632 ) ) ;
#4902 = CARTESIAN_POINT ( 'NONE',  ( 102.4976396683250925, 117.6869444889999841, -53.97500000273119980 ) ) ;
#4903 = CARTESIAN_POINT ( 'NONE',  ( 185.4011555911795313, 40.90078124999999432, -9.598844408820458085 ) ) ;
#4904 = CARTESIAN_POINT ( 'NONE',  ( 71.10665865494748061, 36.00000000000002132, 11.74215035806574825 ) ) ;
#4905 = CARTESIAN_POINT ( 'NONE',  ( 5.444914386472297529, 36.53515625108393294, -13.14518615778179900 ) ) ;
#4906 = CARTESIAN_POINT ( 'NONE',  ( 104.4587341249999781, 1.846868145590750521, 7.250000001365592084 ) ) ;
#4907 =( BOUNDED_CURVE ( )  B_SPLINE_CURVE ( 2, ( #9815, #13793, #15937, #24788, #14363, #11513, #2981, #11801, #9389 ),
 .UNSPECIFIED., .F., .F. ) 
 B_SPLINE_CURVE_WITH_KNOTS ( ( 3, 2, 2, 2, 3 ),
 ( 0.8500000000000007550, 0.8750000000000008882, 0.9000000000000009104, 0.9250000000000009326, 0.9500000000000009548 ),
 .UNSPECIFIED. ) 
 CURVE ( )  GEOMETRIC_REPRESENTATION_ITEM ( )  RATIONAL_B_SPLINE_CURVE ( ( 0.9999999999999976685, 0.9238795325112890700, 1.000000000000000000, 0.9238795325112867385, 1.000000000000000000, 0.9238795325112867385, 1.000000000000000000, 0.9238795325112837409, 1.000000000000003109 ) ) 
 REPRESENTATION_ITEM ( '' )  );
#4908 = CARTESIAN_POINT ( 'NONE',  ( 70.44491438647229131, 37.92421875108393436, -13.14518615778179722 ) ) ;
#4909 = CARTESIAN_POINT ( 'NONE',  ( 59.37712712842203189, 38.46992187499999005, -13.57481594606295339 ) ) ;
#4910 = CARTESIAN_POINT ( 'NONE',  ( 104.9999999999999716, 1.449011120738813565E-14, 0.6250000027311856110 ) ) ;
#4911 = CARTESIAN_POINT ( 'NONE',  ( -5.444914386472299306, 36.93203125108394147, 13.14518615778179722 ) ) ;
#4912 = ADVANCED_FACE ( 'NONE', ( #4637 ), #25873, .T. ) ;
#4913 = ORIENTED_EDGE ( 'NONE', *, *, #20584, .F. ) ;
#4914 = CARTESIAN_POINT ( 'NONE',  ( -13.57481594606304576, 36.23749999999999005, 0.000000000000000000 ) ) ;
#4915 = CARTESIAN_POINT ( 'NONE',  ( 189.5550856135277229, 36.93203125108394147, 13.14518615778179722 ) ) ;
#4916 = CARTESIAN_POINT ( 'NONE',  ( 106.5389055433250860, 105.2492070361643215, -50.82499999726882578 ) ) ;
#4917 = ORIENTED_EDGE ( 'NONE', *, *, #16163, .T. ) ;
#4918 = CARTESIAN_POINT ( 'NONE',  ( 9.598844408820459861, 34.94765624999999432, 9.598844408820456309 ) ) ;
#4919 = CARTESIAN_POINT ( 'NONE',  ( 13.14518615778179900, 35.34453125108392868, 5.444914386472293977 ) ) ;
#4920 = ORIENTED_EDGE ( 'NONE', *, *, #608, .F. ) ;
#4921 = CARTESIAN_POINT ( 'NONE',  ( 135.4449143864723055, 34.65000000108393863, 13.14518615778179189 ) ) ;
#4922 = CARTESIAN_POINT ( 'NONE',  ( 74.29505027212704249, 40.45429687608393721, -9.295050272127046043 ) ) ;
#4923 = CARTESIAN_POINT ( 'NONE',  ( 185.7049497278729575, 35.29492187608393294, 9.295050272127047819 ) ) ;
#4924 = VERTEX_POINT ( 'NONE', #11021 ) ;
#4925 = CARTESIAN_POINT ( 'NONE',  ( 102.0669873000000081, 123.3000000010924850, 0.8561741729129311862 ) ) ;
#4926 = CARTESIAN_POINT ( 'NONE',  ( -5.444914386472297529, 32.46718750108393436, -13.14518615778179900 ) ) ;
#4927 = DIRECTION ( 'NONE',  ( -1.000000000000000000, 0.000000000000000000, 0.000000000000000000 ) ) ;
#4928 = LINE ( 'NONE', #7179, #1331 ) ;
#4929 = CARTESIAN_POINT ( 'NONE',  ( 102.4976396683250925, 117.6869444889999841, -47.72500000273119269 ) ) ;
#4930 = CARTESIAN_POINT ( 'NONE',  ( 2.354566838718444278E-15, 10.00000000000000000, -19.22649730810373470 ) ) ;
#4931 = CARTESIAN_POINT ( 'NONE',  ( 109.0000000000000142, 110.0000000000000000, -45.00000000000000711 ) ) ;
#4932 = CARTESIAN_POINT ( 'NONE',  ( 7.020079488845731852, 31.83418857360491216, -11.28272815150820563 ) ) ;
#4933 = VERTEX_POINT ( 'NONE', #26150 ) ;
#4934 =( LENGTH_UNIT ( ) NAMED_UNIT ( * ) SI_UNIT ( .MILLI., .METRE. ) );
#4935 = CARTESIAN_POINT ( 'NONE',  ( 104.4587341249999639, 1.442382525525748735E-14, 5.937500001365592084 ) ) ;
#4936 = ORIENTED_EDGE ( 'NONE', *, *, #6390, .T. ) ;
#4937 = CARTESIAN_POINT ( 'NONE',  ( 102.4999999999999716, 122.3500000021849701, -1.035533905932742638 ) ) ;
#4938 = CARTESIAN_POINT ( 'NONE',  ( 104.4587341249999781, -1.846868145590721655, 7.875000001365591196 ) ) ;
#4939 = CARTESIAN_POINT ( 'NONE',  ( 200.6228728715777834, 38.07304687499999574, 13.57481594606313813 ) ) ;
#4940 = CARTESIAN_POINT ( 'NONE',  ( -5.444914386472297529, 34.84843750108393579, -13.14518615778179900 ) ) ;
#4941 = CARTESIAN_POINT ( 'NONE',  ( -12.99948823019060384, 36.00000000000000000, 1.999176114741853194 ) ) ;
#4942 = CARTESIAN_POINT ( 'NONE',  ( 55.70494972787295751, 31.92148437608393508, -9.295050272127046043 ) ) ;
#4943 = CARTESIAN_POINT ( 'NONE',  ( 93.46109445667491400, 114.7507929638356785, -45.32500000273119412 ) ) ;
#4944 = CARTESIAN_POINT ( 'NONE',  ( 2.414731522848535132E-15, 36.78320312608393294, 13.14518615778179544 ) ) ;
#4945 = CARTESIAN_POINT ( 'NONE',  ( 96.84719886470463734, 91.93749999863440792, 3.152801135295351997 ) ) ;
#4946 = CARTESIAN_POINT ( 'NONE',  ( 97.83688103937538472, 116.6573956140660897, -48.90000000546238113 ) ) ;
#4947 = CARTESIAN_POINT ( 'NONE',  ( 7.621963534195377754, 54.91641323977498956, 14.99999999999999289 ) ) ;
#4948 = CARTESIAN_POINT ( 'NONE',  ( 96.46446609406726225, 91.49999999726880162, 3.535533905932723986 ) ) ;
#4949 = CARTESIAN_POINT ( 'NONE',  ( 124.3771271284221314, 36.38632812499999858, 13.57481594606304753 ) ) ;
#4950 = VERTEX_POINT ( 'NONE', #2501 ) ;
#4951 = ORIENTED_EDGE ( 'NONE', *, *, #4782, .T. ) ;
#4952 = CARTESIAN_POINT ( 'NONE',  ( 13.57481594606304576, 33.45937499999999432, -1.662435489736055892E-15 ) ) ;
#4953 = EDGE_CURVE ( 'NONE', #12988, #18339, #9315, .T. ) ;
#4954 =( BOUNDED_CURVE ( )  B_SPLINE_CURVE ( 2, ( #8009, #14559, #11994, #23274, #23689, #19826, #16977, #17114, #6435 ),
 .UNSPECIFIED., .F., .F. ) 
 B_SPLINE_CURVE_WITH_KNOTS ( ( 3, 2, 2, 2, 3 ),
 ( 0.7142857142857141906, 0.7232142857142855874, 0.7321428571428569843, 0.7410714285714286031, 0.7500000000000000000 ),
 .UNSPECIFIED. ) 
 CURVE ( )  GEOMETRIC_REPRESENTATION_ITEM ( )  RATIONAL_B_SPLINE_CURVE ( ( 1.000000000000000888, 0.9238795325112857393, 1.000000000000000000, 0.9238795325112867385, 1.000000000000000000, 0.9238795325112867385, 1.000000000000000000, 0.9238795325112867385, 1.000000000000000000 ) ) 
 REPRESENTATION_ITEM ( '' )  );
#4955 = CARTESIAN_POINT ( 'NONE',  ( 5.444914386472297529, 34.94765625108394147, -13.14518615778179900 ) ) ;
#4956 = CARTESIAN_POINT ( 'NONE',  ( 13.57481594606304931, 34.30273437716787299, 5.622872871577869525 ) ) ;
#4957 = CARTESIAN_POINT ( 'NONE',  ( 102.0710678118654329, -4.999999999999989342, 11.43750000273118772 ) ) ;
#4958 = CARTESIAN_POINT ( 'NONE',  ( 135.4449143864723055, 33.65781250108393152, 13.14518615778179189 ) ) ;
#4959 = CARTESIAN_POINT ( 'NONE',  ( 78.57481594606304043, 32.81445312716787299, -5.622872871577873077 ) ) ;
#4960 = VERTEX_POINT ( 'NONE', #6342 ) ;
#4961 = CARTESIAN_POINT ( 'NONE',  ( 13.57481594606304931, 37.47773437716787015, 5.622872871577868636 ) ) ;
#4962 = CARTESIAN_POINT ( 'NONE',  ( -13.57481594606304576, 32.41757812716787157, 5.622872871577880183 ) ) ;
#4963 = VECTOR ( 'NONE', #27904, 1000.000000000000000 ) ;
#4964 = CARTESIAN_POINT ( 'NONE',  ( 55.40115559117954547, 37.92421874999999432, 9.598844408820459861 ) ) ;
#4965 = CARTESIAN_POINT ( 'NONE',  ( 106.5389055433250860, 114.7507929638356785, -48.67499999726882010 ) ) ;
#4966 = CARTESIAN_POINT ( 'NONE',  ( -9.598844408820458085, 38.61875000216787157, -9.598844408820458085 ) ) ;
#4967 = CIRCLE ( 'NONE', #12217, 10.50000000000001599 ) ;
#4968 = CARTESIAN_POINT ( 'NONE',  ( 200.4449143864723055, 35.24531250108393010, 13.14518615778179189 ) ) ;
#4969 = LINE ( 'NONE', #18209, #2002 ) ;
#4970 = CARTESIAN_POINT ( 'NONE',  ( -13.57481594606304576, 33.16171875216787868, 0.000000000000000000 ) ) ;
#4971 = FACE_OUTER_BOUND ( 'NONE', #16611, .T. ) ;
#4972 = CARTESIAN_POINT ( 'NONE',  ( 116.4251840539369596, 36.28710937716787299, -5.622872871577872189 ) ) ;
#4973 = CARTESIAN_POINT ( 'NONE',  ( -13.57481594606304576, 33.06249999999999289, 0.000000000000000000 ) ) ;
#4974 = APPLICATION_CONTEXT ( 'automotive_design' ) ;
#4975 = CARTESIAN_POINT ( 'NONE',  ( 13.14518615778179900, 35.54296875108394715, 5.444914386472293977 ) ) ;
#4976 = CARTESIAN_POINT ( 'NONE',  ( -9.295050272127044266, 37.47773437608393010, 9.295050272127047819 ) ) ;
#4977 = CARTESIAN_POINT ( 'NONE',  ( 9.295050272127047819, 35.29492187608393294, 9.295050272127046043 ) ) ;
#4978 = CARTESIAN_POINT ( 'NONE',  ( -5.622872871577873077, 35.39414062716787157, -13.57481594606304753 ) ) ;
#4979 = DIRECTION ( 'NONE',  ( -0.8660254037844418162, -0.4999999999999947264, 0.000000000000000000 ) ) ;
#4980 = CARTESIAN_POINT ( 'NONE',  ( 101.8468681455906903, 83.75000000136560629, 4.458734124999987891 ) ) ;
#4981 = CARTESIAN_POINT ( 'NONE',  ( 74.29505027212704249, 34.50117187608393010, 9.295050272127046043 ) ) ;
#4982 = CARTESIAN_POINT ( 'NONE',  ( 93.46109445667491400, 114.7507929638356785, -53.57500000273119412 ) ) ;
#4983 = CARTESIAN_POINT ( 'NONE',  ( 101.4086053019245099, 123.0000000000000000, -2.070951898149314907 ) ) ;
#4984 = ORIENTED_EDGE ( 'NONE', *, *, #26043, .T. ) ;
#4985 = EDGE_CURVE ( 'NONE', #7822, #24826, #6464, .T. ) ;
#4986 = CARTESIAN_POINT ( 'NONE',  ( 5.622872871577870413, 37.57695312499999574, -13.57481594606304753 ) ) ;
#4987 = CARTESIAN_POINT ( 'NONE',  ( 2.493653234604083739E-15, 33.26093749999999716, 13.57481594606304576 ) ) ;
#4988 = CARTESIAN_POINT ( 'NONE',  ( 135.4449143864723055, 37.32890625108393579, -13.14518615778179900 ) ) ;
#4989 = ORIENTED_EDGE ( 'NONE', *, *, #21359, .F. ) ;
#4990 = CARTESIAN_POINT ( 'NONE',  ( 99.99999999999995737, 80.25000000000000000, 4.999999999999990230 ) ) ;
#4991 = PRESENTATION_LAYER_ASSIGNMENT (  '', '', ( #6771 ) ) ;
#4992 = CARTESIAN_POINT ( 'NONE',  ( 96.46446609406721961, 3.535533905932755072, 5.875000000000000000 ) ) ;
#4993 = CARTESIAN_POINT ( 'NONE',  ( 96.46446609406721961, 81.00000000273119838, -3.535533905932755072 ) ) ;
#4994 = CARTESIAN_POINT ( 'NONE',  ( 97.92893218813452449, 93.68750000000000000, 4.999999999999983125 ) ) ;
#4995 = AXIS2_PLACEMENT_3D ( 'NONE', #17155, #21165, #17295 ) ;
#4996 = CARTESIAN_POINT ( 'NONE',  ( 101.8468681455907330, 94.74999999863440792, -4.458734124999994997 ) ) ;
#4997 = ADVANCED_FACE ( 'NONE', ( #8762, #24018 ), #15302, .T. ) ;
#4998 = CARTESIAN_POINT ( 'NONE',  ( 93.00000000000000000, 107.7255621263696526, -54.90000000000001279 ) ) ;
#4999 = CARTESIAN_POINT ( 'NONE',  ( 59.55508561352770158, 32.66562500108393863, -13.14518615778179900 ) ) ;
#5000 = ORIENTED_EDGE ( 'NONE', *, *, #2221, .T. ) ;
#5001 = FACE_OUTER_BOUND ( 'NONE', #18248, .T. ) ;
#5002 = CARTESIAN_POINT ( 'NONE',  ( 104.9999999999999574, 2.071067811865491937, 11.56249999999999822 ) ) ;
#5003 = EDGE_CURVE ( 'NONE', #6030, #10914, #12276, .T. ) ;
#5004 = ORIENTED_EDGE ( 'NONE', *, *, #3446, .T. ) ;
#5005 = CARTESIAN_POINT ( 'NONE',  ( -13.14518615778179544, 36.78320312608393294, 0.000000000000000000 ) ) ;
#5006 = CARTESIAN_POINT ( 'NONE',  ( 189.3771271284221314, 35.39414062716787157, -13.57481594606304753 ) ) ;
#5007 = CARTESIAN_POINT ( 'NONE',  ( 9.295050272127046043, 33.11210937608393579, -9.295050272127046043 ) ) ;
#5008 = FACE_OUTER_BOUND ( 'NONE', #10724, .T. ) ;
#5009 = CARTESIAN_POINT ( 'NONE',  ( 5.444914386472302859, 33.85625000108393579, 13.14518615778179189 ) ) ;
#5010 = CARTESIAN_POINT ( 'NONE',  ( 135.4449143864723055, 32.86406250108392868, 13.14518615778179189 ) ) ;
#5011 = CARTESIAN_POINT ( 'NONE',  ( 98.15313185440923860, 91.99999999863439371, 4.458734124999980786 ) ) ;
#5012 = CARTESIAN_POINT ( 'NONE',  ( -13.57481594606304753, 34.60039062499999574, -5.622872871577872189 ) ) ;
#5013 = CARTESIAN_POINT ( 'NONE',  ( 74.59884440882045453, 36.63437500216787157, 9.598844408820456309 ) ) ;
#5014 = CARTESIAN_POINT ( 'NONE',  ( 99.99999999999995737, -4.458734124999988779, 9.937500001365593860 ) ) ;
#5015 = CARTESIAN_POINT ( 'NONE',  ( 132.1298106584280561, 36.02027164734403897, -13.57481594606306174 ) ) ;
#5016 = CARTESIAN_POINT ( 'NONE',  ( 95.54126587499996504, 1.387778780781445676E-14, 8.437500001365592084 ) ) ;
#5017 = CARTESIAN_POINT ( 'NONE',  ( 107.0000000000000142, 110.0000000000000000, -53.50000000546238255 ) ) ;
#5018 = CARTESIAN_POINT ( 'NONE',  ( 101.8468681455907330, 92.37499999863440792, 4.458734124999979898 ) ) ;
#5019 = CYLINDRICAL_SURFACE ( 'NONE', #260, 5.000000000000004441 ) ;
#5020 = CARTESIAN_POINT ( 'NONE',  ( 102.4976396683250783, 102.3130555110000159, -47.02499999726882152 ) ) ;
#5021 = CARTESIAN_POINT ( 'NONE',  ( -9.295050272127044266, 37.67617187608393436, 9.295050272127047819 ) ) ;
#5022 = AXIS2_PLACEMENT_3D ( 'NONE', #13815, #3430, #9272 ) ;
#5023 = EDGE_LOOP ( 'NONE', ( #20899, #645, #28162, #17386 ) ) ;
#5024 = CARTESIAN_POINT ( 'NONE',  ( 96.46446609406726225, 91.62500000000000000, 3.535533905932723986 ) ) ;
#5025 = CARTESIAN_POINT ( 'NONE',  ( -9.598844408820454532, 36.33671874999999574, 9.598844408820459861 ) ) ;
#5026 = EDGE_CURVE ( 'NONE', #17053, #13106, #26884, .T. ) ;
#5027 = CARTESIAN_POINT ( 'NONE',  ( 189.5550856135277229, 36.73359375108393010, 13.14518615778179722 ) ) ;
#5028 = ORIENTED_EDGE ( 'NONE', *, *, #18718, .F. ) ;
#5029 = CARTESIAN_POINT ( 'NONE',  ( 198.8654143754131951, 54.10683252460147941, -15.00000000000000178 ) ) ;
#5030 = CARTESIAN_POINT ( 'NONE',  ( 103.1528011352953342, -3.152801135295355106, 9.062500001365592084 ) ) ;
#5031 = ORIENTED_EDGE ( 'NONE', *, *, #18246, .F. ) ;
#5032 = CARTESIAN_POINT ( 'NONE',  ( 102.4976396683250925, 102.3130555110000159, -52.77500000273119696 ) ) ;
#5033 = CARTESIAN_POINT ( 'NONE',  ( 5.444914386472297529, 36.33671875108394289, -13.14518615778179900 ) ) ;
#5034 = CARTESIAN_POINT ( 'NONE',  ( 94.99999999999995737, 79.12500000273118417, -1.387778780781445676E-14 ) ) ;
#5035 = CARTESIAN_POINT ( 'NONE',  ( 124.5550856135277087, 37.52734375108393294, 13.14518615778179722 ) ) ;
#5036 = CARTESIAN_POINT ( 'NONE',  ( 2.414731522848535132E-15, 40.15664062608393436, 13.14518615778179544 ) ) ;
#5037 = CARTESIAN_POINT ( 'NONE',  ( -5.444914386472297529, 34.84843750108393579, -13.14518615778179900 ) ) ;
#5038 = VECTOR ( 'NONE', #5954, 1000.000000000000000 ) ;
#5039 = CARTESIAN_POINT ( 'NONE',  ( 96.46446609406726225, 93.49999999726881583, 3.535533905932723986 ) ) ;
#5040 = CARTESIAN_POINT ( 'NONE',  ( 59.55508561352770158, 38.22187500108393010, -13.14518615778179900 ) ) ;
#5041 = CARTESIAN_POINT ( 'NONE',  ( 66.60253313061534186, 53.60343507247940664, -15.00000000000000000 ) ) ;
#5042 = CARTESIAN_POINT ( 'NONE',  ( 99.99999999999998579, 118.4984768113314146, -49.87500000273118417 ) ) ;
#5043 = CARTESIAN_POINT ( 'NONE',  ( 181.8548138422181921, 32.86406250108393579, 5.444914386472304635 ) ) ;
#5044 = CARTESIAN_POINT ( 'NONE',  ( 101.0355339059327235, 123.2500000021849615, -2.499999999999998668 ) ) ;
#5045 = CARTESIAN_POINT ( 'NONE',  ( -13.14518615778179189, 36.03906250108394005, 5.444914386472304635 ) ) ;
#5046 = CARTESIAN_POINT ( 'NONE',  ( 104.4587341249999781, 1.846868145590750521, 8.250000001365592084 ) ) ;
#5047 = CARTESIAN_POINT ( 'NONE',  ( 51.85481384221820633, 38.91640625108393436, -5.444914386472297529 ) ) ;
#5048 = CARTESIAN_POINT ( 'NONE',  ( 84.99999999999998579, 95.00000000000000000, 14.99999999999999467 ) ) ;
#5049 = DIRECTION ( 'NONE',  ( 0.000000000000000000, 0.000000000000000000, -1.000000000000000000 ) ) ;
#5050 = CARTESIAN_POINT ( 'NONE',  ( -9.295050272127044266, 34.50117187608393721, 9.295050272127047819 ) ) ;
#5051 = ORIENTED_EDGE ( 'NONE', *, *, #17246, .F. ) ;
#5052 = CARTESIAN_POINT ( 'NONE',  ( 99.99999999999998579, 123.5500000010924850, -2.066987299999998751 ) ) ;
#5053 = CARTESIAN_POINT ( 'NONE',  ( 2.493653234604083739E-15, 34.05468749999999289, 13.57481594606304576 ) ) ;
#5054 = CARTESIAN_POINT ( 'NONE',  ( 181.8548138422182205, 37.52734375108393294, -5.444914386472297529 ) ) ;
#5055 = CARTESIAN_POINT ( 'NONE',  ( 102.4976396683250783, 117.6869444889999841, -48.47499999726882436 ) ) ;
#5056 = ORIENTED_EDGE ( 'NONE', *, *, #71, .T. ) ;
#5057 = AXIS2_PLACEMENT_3D ( 'NONE', #25147, #10028, #12020 ) ;
#5058 = CARTESIAN_POINT ( 'NONE',  ( 13.57481594606304931, 34.20351562499999432, 5.622872871577869525 ) ) ;
#5059 = CARTESIAN_POINT ( 'NONE',  ( -5.444914386472299306, 33.55859375108393294, 13.14518615778179722 ) ) ;
#5060 = ORIENTED_EDGE ( 'NONE', *, *, #14583, .F. ) ;
#5061 = CARTESIAN_POINT ( 'NONE',  ( 143.1451861577818079, 33.26093750108393721, -5.444914386472297529 ) ) ;
#5062 = CARTESIAN_POINT ( 'NONE',  ( 71.94442379715272295, 31.55306878032414986, -11.16113333171310451 ) ) ;
#5063 = CARTESIAN_POINT ( 'NONE',  ( 189.5550856135277229, 32.66562500108393863, -13.14518615778179900 ) ) ;
#5064 = ORIENTED_EDGE ( 'NONE', *, *, #15621, .T. ) ;
#5065 = CARTESIAN_POINT ( 'NONE',  ( 97.93301270000000613, 124.5500000010924850, -9.540979117872439019E-15 ) ) ;
#5066 = CARTESIAN_POINT ( 'NONE',  ( 8.402315781223892444, 54.99999999485618929, -15.00000000000000000 ) ) ;
#5067 = CIRCLE ( 'NONE', #27815, 5.000000000000000888 ) ;
#5068 = CARTESIAN_POINT ( 'NONE',  ( 120.4011555911795455, 38.61875000216787157, -9.598844408820458085 ) ) ;
#5069 = CARTESIAN_POINT ( 'NONE',  ( 99.99999999999998579, 101.5015231886685712, -46.62500000273119838 ) ) ;
#5070 = EDGE_CURVE ( 'NONE', #11095, #14819, #20169, .T. ) ;
#5071 =( BOUNDED_CURVE ( )  B_SPLINE_CURVE ( 2, ( #11165, #18133, #9434, #12532, #6147, #14676, #27542, #6012, #12258, #5602, #20848 ),
 .UNSPECIFIED., .F., .F. ) 
 B_SPLINE_CURVE_WITH_KNOTS ( ( 3, 2, 2, 2, 2, 3 ),
 ( 0.8000000000000000444, 0.8199999999999999512, 0.8399999999999999689, 0.8599999999999999867, 0.8800000000000000044, 0.9000000000000000222 ),
 .UNSPECIFIED. ) 
 CURVE ( )  GEOMETRIC_REPRESENTATION_ITEM ( )  RATIONAL_B_SPLINE_CURVE ( ( 1.000000000000000000, 0.9510565162951535312, 1.000000000000000000, 0.9510565162951535312, 1.000000000000000000, 0.9510565162951535312, 1.000000000000000000, 0.9510565162951535312, 1.000000000000000000, 0.9510565162951535312, 1.000000000000000000 ) ) 
 REPRESENTATION_ITEM ( '' )  );
#5072 = CARTESIAN_POINT ( 'NONE',  ( 102.0710678118654329, -4.999999999999989342, 2.437500002731185056 ) ) ;
#5073 = CARTESIAN_POINT ( 'NONE',  ( 2.493653234604083739E-15, 34.94765625216787441, 13.57481594606304576 ) ) ;
#5074 = CARTESIAN_POINT ( 'NONE',  ( 66.50549218155768472, 53.60078691996477573, 14.99999999999997868 ) ) ;
#5075 = ORIENTED_EDGE ( 'NONE', *, *, #15588, .F. ) ;
#5076 = PRESENTATION_STYLE_ASSIGNMENT (( #24597 ) ) ;
#5077 = CARTESIAN_POINT ( 'NONE',  ( 98.15313185440925281, -4.458734124999987891, 3.625000001365591640 ) ) ;
#5078 = ORIENTED_EDGE ( 'NONE', *, *, #17322, .T. ) ;
#5079 = CARTESIAN_POINT ( 'NONE',  ( 101.8468681455906903, -4.458734124999987891, 7.750000001365592084 ) ) ;
#5080 = CARTESIAN_POINT ( 'NONE',  ( 133.9798144458084721, 50.00000000123269928, 13.01613927312840779 ) ) ;
#5081 = CARTESIAN_POINT ( 'NONE',  ( 2.414731522848535132E-15, 35.19570312608392726, 13.14518615778179544 ) ) ;
#5082 = CARTESIAN_POINT ( 'NONE',  ( 99.99999999999995737, 1.387778780781445676E-14, 34.79898987322334136 ) ) ;
#5083 = CARTESIAN_POINT ( 'NONE',  ( 59.55508561352770158, 33.45937500108394147, -13.14518615778179900 ) ) ;
#5084 = CARTESIAN_POINT ( 'NONE',  ( 95.54126587499999346, 92.87499999863440792, 1.846868145590722543 ) ) ;
#5085 = CARTESIAN_POINT ( 'NONE',  ( 91.91746824999998466, 112.6261737610028320, -47.22500000273119269 ) ) ;
#5086 = CARTESIAN_POINT ( 'NONE',  ( 13.14518615778179722, 37.82500000108392868, -5.444914386472297529 ) ) ;
#5087 = CARTESIAN_POINT ( 'NONE',  ( 107.0000000000000142, 110.0000000000000000, -49.50000000546238255 ) ) ;
#5088 = CARTESIAN_POINT ( 'NONE',  ( -3.114697745540297547, 53.90847045361019951, 15.00000000000000000 ) ) ;
#5089 = DIRECTION ( 'NONE',  ( 0.000000000000000000, 0.000000000000000000, 1.000000000000000000 ) ) ;
#5090 = CARTESIAN_POINT ( 'NONE',  ( 116.4251840539369596, 35.44374999999999432, 0.000000000000000000 ) ) ;
#5091 = ORIENTED_EDGE ( 'NONE', *, *, #18034, .T. ) ;
#5092 = FACE_BOUND ( 'NONE', #17419, .T. ) ;
#5093 = CARTESIAN_POINT ( 'NONE',  ( -8.049105076161786076E-16, 34.99726562608393721, -13.14518615778179544 ) ) ;
#5094 = CARTESIAN_POINT ( 'NONE',  ( 2.493653234604083739E-15, 34.94765625216787441, 13.57481594606304576 ) ) ;
#5095 = CARTESIAN_POINT ( 'NONE',  ( 104.9999999999999574, -2.071067811865462627, 9.562500002731184168 ) ) ;
#5096 = CARTESIAN_POINT ( 'NONE',  ( 124.5550856135277087, 33.26093750108393721, -13.14518615778179900 ) ) ;
#5097 = CARTESIAN_POINT ( 'NONE',  ( 51.42518405393695957, 31.57421875216786944, 0.000000000000000000 ) ) ;
#5098 = CARTESIAN_POINT ( 'NONE',  ( 51.42518405393695957, 37.08085937716787583, -5.622872871577872189 ) ) ;
#5099 = CARTESIAN_POINT ( 'NONE',  ( 13.14518615778179900, 40.10703125108393152, 5.444914386472293977 ) ) ;
#5100 = CARTESIAN_POINT ( 'NONE',  ( 99.99999999999995737, -4.999999999999990230, 1.249999999999999334 ) ) ;
#5101 = CARTESIAN_POINT ( 'NONE',  ( 106.5389055433250860, 105.2492070361643215, -53.07499999726881867 ) ) ;
#5102 = EDGE_CURVE ( 'NONE', #4419, #23118, #1580, .T. ) ;
#5103 = CARTESIAN_POINT ( 'NONE',  ( -8.312177448680279460E-16, 40.10703125216787157, -13.57481594606304576 ) ) ;
#5104 = CARTESIAN_POINT ( 'NONE',  ( 204.2950502721270425, 32.31835937608393294, -9.295050272127046043 ) ) ;
#5105 = DIRECTION ( 'NONE',  ( 0.000000000000000000, 0.000000000000000000, 1.000000000000000000 ) ) ;
#5106 = CARTESIAN_POINT ( 'NONE',  ( -9.598844408820454532, 33.26093750216787726, 9.598844408820459861 ) ) ;
#5107 = CARTESIAN_POINT ( 'NONE',  ( 99.99999999999998579, 89.99899999999999523, 2.499999999999985789 ) ) ;
#5108 = CARTESIAN_POINT ( 'NONE',  ( 96.46446609406726225, 94.49999999726881583, 3.535533905932723986 ) ) ;
#5109 = CARTESIAN_POINT ( 'NONE',  ( -8.312177448680279460E-16, 35.24531249999999716, -13.57481594606304576 ) ) ;
#5110 = CARTESIAN_POINT ( 'NONE',  ( -5.622872871577873077, 32.91367187499999858, -13.57481594606304753 ) ) ;
#5111 = DIRECTION ( 'NONE',  ( 5.782411586589357392E-17, -0.000000000000000000, 1.000000000000000000 ) ) ;
#5112 = CARTESIAN_POINT ( 'NONE',  ( -5.444914386472299306, 35.34453125108393579, 13.14518615778179722 ) ) ;
#5113 = CARTESIAN_POINT ( 'NONE',  ( 2.414731522848535132E-15, 35.98945312608393010, 13.14518615778179544 ) ) ;
#5114 = CARTESIAN_POINT ( 'NONE',  ( -13.14518615778179189, 35.04687500108393294, 5.444914386472304635 ) ) ;
#5115 = CARTESIAN_POINT ( 'NONE',  ( -13.57481594606304753, 37.08085937716786873, -5.622872871577873077 ) ) ;
#5116 = DIRECTION ( 'NONE',  ( -0.000000000000000000, 1.000000000000000000, -0.000000000000000000 ) ) ;
#5117 = CARTESIAN_POINT ( 'NONE',  ( 74.29505027212704249, 40.25585937608393294, 9.295050272127046043 ) ) ;
#5118 =( BOUNDED_CURVE ( )  B_SPLINE_CURVE ( 2, ( #8648, #21206, #10348, #19055, #3962, #25752, #12622, #4099, #21348, #1826, #12762, #21482, #1962, #10631, #2099, #28039, #8506, #17191, #25898, #6368, #15040, #12893, #10767, #19478, #20048, #17613, #13461, #4802, #2522, #26467, #15892, #26753, #11183, #15325, #15614, #7196, #22186, #527, #17471, #20188, #24181, #22332, #6921, #15467, #17902, #24316, #13748, #2666, #13321, #24608, #26321, #24460, #672, #24038, #2388, #5086, #11327, #22473, #6782, #4517, #20330, #21913, #9346, #19756, #18039, #9208, #26611, #2802, #7057, #2936, #26173, #15756, #13609, #13174, #11607, #22046, #4944, #8925, #4659, #11046, #385, #11469, #8784, #238, #6640, #19901, #9069, #17764, #11754, #9767, #14311, #22617, #18476 ),
 .UNSPECIFIED., .F., .F. ) 
 B_SPLINE_CURVE_WITH_KNOTS ( ( 3, 2, 2, 2, 2, 2, 2, 2, 2, 2, 2, 2, 2, 2, 2, 2, 2, 2, 2, 2, 2, 2, 2, 2, 2, 2, 2, 2, 2, 2, 2, 2, 2, 2, 2, 2, 2, 2, 2, 2, 2, 2, 2, 2, 2, 2, 3 ),
 ( 0.000000000000000000, 0.01041666666666666609, 0.02083333333333333218, 0.03125000000000000000, 0.04166666666666666435, 0.05208333333333333565, 0.06250000000000000000, 0.07291666666666667129, 0.08333333333333332871, 0.09375000000000000000, 0.1041666666666666713, 0.1145833333333333287, 0.1250000000000000000, 0.1354166666666666574, 0.1458333333333333426, 0.1562500000000000000, 0.1666666666666666574, 0.1770833333333333426, 0.1875000000000000000, 0.1979166666666666574, 0.2083333333333333426, 0.2187500000000000000, 0.2291666666666666574, 0.2395833333333333426, 0.2500000000000000000, 0.2604166666666666852, 0.2708333333333333148, 0.2812500000000000000, 0.2916666666666666852, 0.3020833333333333148, 0.3125000000000000000, 0.3229166666666666852, 0.3333333333333333148, 0.3437500000000000000, 0.3541666666666666852, 0.3645833333333333148, 0.3750000000000000000, 0.3854166666666666852, 0.3958333333333333148, 0.4062500000000000000, 0.4166666666666666852, 0.4270833333333333148, 0.4375000000000000000, 0.4479166666666666852, 0.4583333333333333148, 0.4687500000000000000, 0.4779971559588572227 ),
 .UNSPECIFIED. ) 
 CURVE ( )  GEOMETRIC_REPRESENTATION_ITEM ( )  RATIONAL_B_SPLINE_CURVE ( ( 1.000000000000000000, 0.9238795325112867385, 1.000000000000000000, 0.9238795325112867385, 1.000000000000000000, 0.9238795325112867385, 1.000000000000000000, 0.9238795325112867385, 1.000000000000000000, 0.9238795325112867385, 1.000000000000000000, 0.9238795325112867385, 1.000000000000000000, 0.9238795325112867385, 1.000000000000000000, 0.9238795325112867385, 1.000000000000000000, 0.9238795325112867385, 1.000000000000000000, 0.9238795325112867385, 1.000000000000000000, 0.9238795325112867385, 1.000000000000000000, 0.9238795325112867385, 1.000000000000000000, 0.9238795325112867385, 1.000000000000000000, 0.9238795325112867385, 1.000000000000000000, 0.9238795325112867385, 1.000000000000000000, 0.9238795325112867385, 1.000000000000000000, 0.9238795325112867385, 1.000000000000000000, 0.9238795325112867385, 1.000000000000000000, 0.9238795325112867385, 1.000000000000000000, 0.9238795325112867385, 1.000000000000000000, 0.9238795325112867385, 1.000000000000000000, 0.9238795325112867385, 1.000000000000000000, 0.9238795325112867385, 1.000000000000000000, 0.9238795325112867385, 1.000000000000000000, 0.9238795325112867385, 1.000000000000000000, 0.9238795325112867385, 1.000000000000000000, 0.9238795325112867385, 1.000000000000000000, 0.9238795325112867385, 1.000000000000000000, 0.9238795325112867385, 1.000000000000000000, 0.9238795325112867385, 1.000000000000000000, 0.9238795325112867385, 1.000000000000000000, 0.9238795325112867385, 1.000000000000000000, 0.9238795325112867385, 1.000000000000000000, 0.9238795325112867385, 1.000000000000000000, 0.9238795325112867385, 1.000000000000000000, 0.9238795325112867385, 1.000000000000000000, 0.9238795325112867385, 1.000000000000000000, 0.9238795325112867385, 1.000000000000000000, 0.9238795325112867385, 1.000000000000000000, 0.9238795325112867385, 1.000000000000000000, 0.9238795325112867385, 1.000000000000000000, 0.9238795325112867385, 1.000000000000000000, 0.9238795325112867385, 1.000000000000000000, 0.9238795325112867385, 1.000000000000000000, 0.9238795325112867385, 1.000000000000000000, 0.9324258078851919151, 0.9848264816800302857 ) ) 
 REPRESENTATION_ITEM ( '' )  );
#5119 = CARTESIAN_POINT ( 'NONE',  ( 102.4976396683250925, 117.6869444889999841, -51.97500000273119980 ) ) ;
#5120 = CARTESIAN_POINT ( 'NONE',  ( -9.598844408820458085, 35.44375000216787441, -9.598844408820458085 ) ) ;
#5121 = CARTESIAN_POINT ( 'NONE',  ( 99.99999999999998579, 123.1500000010924794, 2.066987299999980099 ) ) ;
#5122 = CARTESIAN_POINT ( 'NONE',  ( 5.622872871577871301, 32.81445312499999289, -13.57481594606304753 ) ) ;
#5123 = CARTESIAN_POINT ( 'NONE',  ( 139.2950502721270425, 34.69960937608393436, 9.295050272127046043 ) ) ;
#5124 = EDGE_LOOP ( 'NONE', ( #18452, #7101 ) ) ;
#5125 = CARTESIAN_POINT ( 'NONE',  ( 103.5355339059327093, 81.62500000000000000, -3.535533905932755072 ) ) ;
#5126 = CARTESIAN_POINT ( 'NONE',  ( 70.62287287157791127, 38.17226562716787441, 13.57481594606301023 ) ) ;
#5127 = CARTESIAN_POINT ( 'NONE',  ( 104.4587341249999639, 82.93750000136560629, -1.442382525525748735E-14 ) ) ;
#5128 = CARTESIAN_POINT ( 'NONE',  ( 103.5355339059327235, 92.12500000000000000, -3.535533905932738197 ) ) ;
#5129 = CARTESIAN_POINT ( 'NONE',  ( 78.57481594606304043, 39.16445312716788152, -5.622872871577873077 ) ) ;
#5130 = EDGE_CURVE ( 'NONE', #14907, #1287, #938, .T. ) ;
#5131 = CARTESIAN_POINT ( 'NONE',  ( 95.00472066334982912, 116.8754121666685393, -47.92499999726882010 ) ) ;
#5132 = CARTESIAN_POINT ( 'NONE',  ( 55.70494972787295751, 32.71523437608393436, -9.295050272127046043 ) ) ;
#5133 = CARTESIAN_POINT ( 'NONE',  ( 74.29505027212704249, 36.28710937608393294, 9.295050272127046043 ) ) ;
#5134 = VERTEX_POINT ( 'NONE', #27021 ) ;
#5135 = CARTESIAN_POINT ( 'NONE',  ( 96.46446609406721961, -3.535533905932727539, 9.250000002731184168 ) ) ;
#5136 = VECTOR ( 'NONE', #14065, 1000.000000000000000 ) ;
#5137 = CARTESIAN_POINT ( 'NONE',  ( 102.0710678118654329, -4.999999999999989342, 14.31249999999999822 ) ) ;
#5138 = ORIENTED_EDGE ( 'NONE', *, *, #22744, .F. ) ;
#5139 = CARTESIAN_POINT ( 'NONE',  ( -13.14518615778179900, 35.93984375108393436, -5.444914386472297529 ) ) ;
#5140 = CARTESIAN_POINT ( 'NONE',  ( 181.4251840539369596, 35.59257812716788294, 5.622872871577880183 ) ) ;
#5141 = EDGE_CURVE ( 'NONE', #15733, #506, #16161, .T. ) ;
#5142 = CARTESIAN_POINT ( 'NONE',  ( -13.14518615778179189, 33.45937500108393436, 5.444914386472304635 ) ) ;
#5143 = PRODUCT_DEFINITION_SHAPE ( 'NONE', 'NONE',  #28210 ) ;
#5144 = LINE ( 'NONE', #301, #14401 ) ;
#5145 = CARTESIAN_POINT ( 'NONE',  ( 96.46446609406721961, -3.535533905932727539, 3.124999999999999112 ) ) ;
#5146 = CARTESIAN_POINT ( 'NONE',  ( 13.14518615778179900, 35.54296875108394715, 5.444914386472293977 ) ) ;
#5147 = EDGE_CURVE ( 'NONE', #22018, #747, #14312, .T. ) ;
#5148 = CARTESIAN_POINT ( 'NONE',  ( 84.99999999999998579, 120.0000000000000000, -43.00000000000000000 ) ) ;
#5149 = CARTESIAN_POINT ( 'NONE',  ( 103.1528011352953484, 92.43749999863440792, -3.152801135295366208 ) ) ;
#5150 = DIRECTION ( 'NONE',  ( 0.000000000000000000, 0.000000000000000000, -1.000000000000000000 ) ) ;
#5151 = EDGE_CURVE ( 'NONE', #2199, #27806, #4479, .T. ) ;
#5152 = DIRECTION ( 'NONE',  ( 1.000000000000000000, 0.000000000000000000, 0.000000000000000000 ) ) ;
#5153 = FACE_OUTER_BOUND ( 'NONE', #3404, .T. ) ;
#5154 = CARTESIAN_POINT ( 'NONE',  ( 95.54126587499996504, 1.387778780781445676E-14, 6.687500001365592084 ) ) ;
#5155 = CARTESIAN_POINT ( 'NONE',  ( 103.1528011352953342, -3.152801135295355106, 8.812500001365592084 ) ) ;
#5156 = CARTESIAN_POINT ( 'NONE',  ( 91.91746824999999887, 110.0000000000000000, -45.12500000273119838 ) ) ;
#5157 = CARTESIAN_POINT ( 'NONE',  ( 95.54126587500000767, 92.06249999863440792, -7.484931351350258973E-15 ) ) ;
#5158 = DIRECTION ( 'NONE',  ( 0.000000000000000000, 0.000000000000000000, -1.000000000000000000 ) ) ;
#5159 = CARTESIAN_POINT ( 'NONE',  ( 93.46109445667489979, 114.7507929638356785, -53.82499999726881867 ) ) ;
#5160 = CARTESIAN_POINT ( 'NONE',  ( 13.14518615778179900, 34.74921875108395142, 5.444914386472293977 ) ) ;
#5161 = VECTOR ( 'NONE', #22435, 1000.000000000000000 ) ;
#5162 = EDGE_CURVE ( 'NONE', #5134, #18802, #7382, .T. ) ;
#5163 = ORIENTED_EDGE ( 'NONE', *, *, #24104, .T. ) ;
#5164 = CARTESIAN_POINT ( 'NONE',  ( -8.312177448680279460E-16, 40.10703125216787157, -13.57481594606304576 ) ) ;
#5165 = FACE_OUTER_BOUND ( 'NONE', #25670, .T. ) ;
#5166 = CARTESIAN_POINT ( 'NONE',  ( 181.8548138422182205, 37.37851562608393863, 0.000000000000000000 ) ) ;
#5167 = ORIENTED_EDGE ( 'NONE', *, *, #7425, .T. ) ;
#5168 = CARTESIAN_POINT ( 'NONE',  ( 5.622872871577863307, 39.75976562716787299, 13.57481594606306174 ) ) ;
#5169 = CARTESIAN_POINT ( 'NONE',  ( 101.8468681455906903, 4.458734125000016313, 11.37500000136559386 ) ) ;
#5170 = EDGE_CURVE ( 'NONE', #21081, #21036, #490, .T. ) ;
#5171 = ORIENTED_EDGE ( 'NONE', *, *, #3048, .F. ) ;
#5172 = CARTESIAN_POINT ( 'NONE',  ( 105.6631189606246295, 114.1144967660473242, -46.80000000000001137 ) ) ;
#5173 = CARTESIAN_POINT ( 'NONE',  ( -5.444914386472299306, 37.52734375108393294, 13.14518615778179722 ) ) ;
#5174 = CARTESIAN_POINT ( 'NONE',  ( 98.96446609406727646, 124.3499999999999943, 2.499999999999977796 ) ) ;
#5175 = DIRECTION ( 'NONE',  ( -1.000000000000000000, 0.000000000000000000, 2.385244779468110248E-16 ) ) ;
#5176 = CARTESIAN_POINT ( 'NONE',  ( 120.7049497278729575, 39.06523437608392868, 9.295050272127047819 ) ) ;
#5177 = CARTESIAN_POINT ( 'NONE',  ( -5.444914386472299306, 36.93203125108394147, 13.14518615778179722 ) ) ;
#5178 = CIRCLE ( 'NONE', #27037, 5.000000000000004441 ) ;
#5179 = CARTESIAN_POINT ( 'NONE',  ( 9.295050272127047819, 36.88242187608393152, 9.295050272127046043 ) ) ;
#5180 = EDGE_CURVE ( 'NONE', #5426, #15725, #17035, .T. ) ;
#5181 = CARTESIAN_POINT ( 'NONE',  ( 96.84719886470463734, 94.18749999863440792, 3.152801135295351997 ) ) ;
#5182 = CARTESIAN_POINT ( 'NONE',  ( -13.57481594606304576, 36.33671875216787583, 0.000000000000000000 ) ) ;
#5183 = CARTESIAN_POINT ( 'NONE',  ( 95.00472066334981491, 103.1245878333314465, -49.07500000273119412 ) ) ;
#5184 = ADVANCED_FACE ( 'NONE', ( #21147 ), #5911, .T. ) ;
#5185 = CARTESIAN_POINT ( 'NONE',  ( 77.00957333851108899, 35.99999999999999289, 5.901833544882738813 ) ) ;
#5186 = CARTESIAN_POINT ( 'NONE',  ( -5.444914386472297529, 35.84062500108394289, -13.14518615778179900 ) ) ;
#5187 = CARTESIAN_POINT ( 'NONE',  ( 101.8468681455907046, -4.458734124999987891, 8.000000001365592084 ) ) ;
#5188 = CARTESIAN_POINT ( 'NONE',  ( 51.85481384221821344, 38.22187500108393721, 5.444914386472304635 ) ) ;
#5189 = CARTESIAN_POINT ( 'NONE',  ( 102.4999999999999858, 124.6500000000000057, -1.035533905932742638 ) ) ;
#5190 = CARTESIAN_POINT ( 'NONE',  ( 200.9085077471931413, 36.04503594658366694, 12.68159279706094367 ) ) ;
#5191 = CARTESIAN_POINT ( 'NONE',  ( -9.295050272127046043, 35.09648437608393579, -9.295050272127046043 ) ) ;
#5192 = VERTEX_POINT ( 'NONE', #7617 ) ;
#5193 = CARTESIAN_POINT ( 'NONE',  ( 99.14382582708707048, 123.9000000010924794, 2.066987299999979211 ) ) ;
#5194 = CARTESIAN_POINT ( 'NONE',  ( -13.57481594606304753, 36.18789062499999432, -5.622872871577872189 ) ) ;
#5195 = CARTESIAN_POINT ( 'NONE',  ( 189.5550856135277229, 37.72578125108394431, 13.14518615778179722 ) ) ;
#5196 = CARTESIAN_POINT ( 'NONE',  ( 95.00472066334982912, 116.8754121666685393, -50.17499999726882010 ) ) ;
#5197 = ORIENTED_EDGE ( 'NONE', *, *, #27168, .T. ) ;
#5198 = CARTESIAN_POINT ( 'NONE',  ( 9.598844408820459861, 33.36015624999999574, 9.598844408820456309 ) ) ;
#5199 = CARTESIAN_POINT ( 'NONE',  ( -5.444914386472299306, 32.76484375108393010, 13.14518615778179722 ) ) ;
#5200 = ORIENTED_EDGE ( 'NONE', *, *, #16341, .F. ) ;
#5201 = CARTESIAN_POINT ( 'NONE',  ( 130.0000000000000000, 33.01289062608393721, 13.14518615778179544 ) ) ;
#5202 = CARTESIAN_POINT ( 'NONE',  ( 70.44491438647229131, 40.50390625108394005, -13.14518615778179722 ) ) ;
#5203 = ORIENTED_EDGE ( 'NONE', *, *, #26645, .T. ) ;
#5204 = CARTESIAN_POINT ( 'NONE',  ( 181.8548138422181921, 34.35234375108393579, -5.444914386472297529 ) ) ;
#5205 = EDGE_LOOP ( 'NONE', ( #2807, #11369, #18826, #27889 ) ) ;
#5206 = CARTESIAN_POINT ( 'NONE',  ( 104.9999999999999858, -2.071067811865457298, 13.43749999999999822 ) ) ;
#5207 = CARTESIAN_POINT ( 'NONE',  ( 3.863925265119776853, 54.10645156200111927, -15.00000000000000000 ) ) ;
#5208 = CARTESIAN_POINT ( 'NONE',  ( 99.99999999999998579, 89.99899999999999523, -2.500000000000004885 ) ) ;
#5209 = EDGE_CURVE ( 'NONE', #24544, #3701, #12014, .T. ) ;
#5210 = CARTESIAN_POINT ( 'NONE',  ( 116.4251840539369454, 37.87460937716787868, -5.622872871577873077 ) ) ;
#5211 = CARTESIAN_POINT ( 'NONE',  ( 97.50236033167492167, 102.3130555110000159, -44.72500000273119980 ) ) ;
#5212 = DIRECTION ( 'NONE',  ( 0.000000000000000000, -1.000000000000000000, 3.469446951953611231E-16 ) ) ;
#5213 = CARTESIAN_POINT ( 'NONE',  ( 5.622872871577832221, 36.48554687499999716, 13.57481594606309194 ) ) ;
#5214 = CARTESIAN_POINT ( 'NONE',  ( 185.7049497278729575, 40.05742187608393579, 9.295050272127047819 ) ) ;
#5215 = ORIENTED_EDGE ( 'NONE', *, *, #1492, .T. ) ;
#5216 = SURFACE_STYLE_FILL_AREA ( #19890 ) ;
#5217 = CARTESIAN_POINT ( 'NONE',  ( 96.84719886470459471, -3.152801135295355994, 5.562500001365591196 ) ) ;
#5218 = ORIENTED_EDGE ( 'NONE', *, *, #2230, .F. ) ;
#5219 = CARTESIAN_POINT ( 'NONE',  ( -11.93524237669063126, 36.00000000000001421, -5.809862729998008568 ) ) ;
#5220 = CARTESIAN_POINT ( 'NONE',  ( 103.1528011352953342, -3.152801135295355106, 6.812500001365592084 ) ) ;
#5221 = CARTESIAN_POINT ( 'NONE',  ( 133.6364962467980035, 51.46815297079191254, 14.99999999999789857 ) ) ;
#5222 = CARTESIAN_POINT ( 'NONE',  ( 0.000000000000000000, 23.00000000000000000, 0.000000000000000000 ) ) ;
#5223 = CARTESIAN_POINT ( 'NONE',  ( 59.55508561352770158, 32.96328125108393436, 13.14518615778179722 ) ) ;
#5224 = CARTESIAN_POINT ( 'NONE',  ( 107.0000000000000000, 110.0000000000000000, -47.49999999453763877 ) ) ;
#5225 = FACE_OUTER_BOUND ( 'NONE', #26873, .T. ) ;
#5226 = CARTESIAN_POINT ( 'NONE',  ( 2.493653234604083739E-15, 40.40468749999999432, 13.57481594606304576 ) ) ;
#5227 = CARTESIAN_POINT ( 'NONE',  ( 65.00000000000000000, -7.395377635281828788, -7.517135062566165128E-15 ) ) ;
#5228 = CARTESIAN_POINT ( 'NONE',  ( -9.180175813647988292, 50.00000000000000711, 15.00000000000000355 ) ) ;
#5229 = CARTESIAN_POINT ( 'NONE',  ( 51.42518405393695957, 40.95039062499999005, -5.622872871577872189 ) ) ;
#5230 = CARTESIAN_POINT ( 'NONE',  ( 116.4251840539369596, 33.11210937499999574, 5.622872871577880183 ) ) ;
#5231 = ORIENTED_EDGE ( 'NONE', *, *, #20288, .T. ) ;
#5232 = CARTESIAN_POINT ( 'NONE',  ( -15.00000000000000178, 75.00000000000000000, 1.734723475976807489E-15 ) ) ;
#5233 = CARTESIAN_POINT ( 'NONE',  ( 13.14518615778179900, 34.05468750108394005, -5.444914386472297529 ) ) ;
#5234 = CARTESIAN_POINT ( 'NONE',  ( 9.598844408820456309, 33.65781250216787157, -9.598844408820458085 ) ) ;
#5235 =( BOUNDED_SURFACE ( )  B_SPLINE_SURFACE ( 1, 2, ( 
 ( #21520, #19517, #27664, #28078, #15217, #16822, #4416, #8126, #25518, #12799, #5997, #4136, #14662, #10666, #27938, #21245, #10388, #8260, #8397, #16947, #17086, #19374, #25648, #6132, #14797, #23521, #25789, #14939, #8542, #17228, #22087, #2426, #11227, #15656, #13214, #26652, #15933, #19943, #2564, #568, #422, #13508, #9108, #26214, #2841, #17802, #15798, #26506, #24356, #4699, #6962, #9385, #13653, #24501, #4845, #24650, #22229, #2708, #4554, #11368, #13070, #20090, #17654, #9250, #10943, #13360, #8823, #18082, #19655, #4988, #280, #21807, #2285, #17942, #7100, #11086, #21948, #22368, #20228, #24220, #11509, #710, #26795, #6675, #137, #7241, #17513, #15362, #24076, #19796, #8966, #26362, #6820, #15510, #16077, #16513, #11938, #1145, #27362, #5557, #25206, #13790, #12073, #9943, #860, #3551, #18658, #11652, #25070, #7821, #16369, #16650, #22940, #16227, #18230, #20375, #9532, #14081, #5692, #24927, #14222, #24785, #5123, #27079, #26940, #7384, #5413, #9812, #12208, #22801, #22659, #3270, #7677, #5266, #14359, #7952, #20660, #18518, #20798, #27223, #3403, #1278, #13932, #23075, #20935, #1419, #10078, #18790, #27497, #22511, #2977, #3131, #11797, #20520, #1002, #9671, #18374, #7531, #25485, #1695, #10497, #23627, #10213, #14631, #21072, #19341, #10635, #14767, #23486, #12483, #8651, #8091, #16786, #27769, #8512, #12898, #25617, #12627, #28181, #25345, #3967, #10352, #8367 ),
 ( #25756, #18923, #12354, #27906, #6100, #1967, #17052, #28045, #21353, #5830, #14498, #25902, #5963, #17195, #1833, #19204, #6372, #6238, #15045, #23215, #4103, #23762, #1560, #4239, #21629, #3690, #14906, #2104, #12768, #27631, #21486, #8227, #23350, #3823, #21210, #10772, #19483, #16917, #19061, #105, #17340, #11051, #2251, #23901, #243, #13325, #15760, #26326, #6643, #15471, #19907, #17476, #2670, #20192, #24185, #6786, #4807, #4663, #17768, #22052, #10912, #7063, #2526, #20053, #11188, #390, #8929, #9072, #13613, #17906, #531, #26471, #677, #15183, #24466, #6925, #26177, #21917, #15619, #24321, #19622, #15329, #13037, #11331, #9212, #13465, #22190, #4520, #26037, #8788, #24044, #19760, #26616, #4949, #17618, #22336, #6507, #4381, #2806, #2392, #11473, #13178, #21773, #1105, #822, #18481, #12169, #20619, #13895, #7491, #7200, #962, #5090, #5652, #15895, #20757, #24749, #20898, #18043, #16187, #14041, #7347, #9490, #1242, #14181, #9772, #22898, #18337, #9352, #26758, #9905, #20335, #18618, #24893, #5374, #3362, #27188, #27323, #24612, #16333, #12034, #13752, #7780, #16467, #22477, #7639, #25161, #25031, #2941, #5514, #20483, #11612, #18191, #26901, #27044, #14315, #9632, #23037, #16038, #5230, #3091, #22621, #11758, #22764, #3229, #3508, #11896, #18881, #27732, #3927, #1517, #14870, #4203, #8192, #10311, #17014, #19018, #1794, #16882, #14457, #19308, #25581, #4068 ) ),
 .UNSPECIFIED., .F., .F., .T. ) 
 B_SPLINE_SURFACE_WITH_KNOTS ( ( 2, 2 ),
 ( 3, 2, 2, 2, 2, 2, 2, 2, 2, 2, 2, 2, 2, 2, 2, 2, 2, 2, 2, 2, 2, 2, 2, 2, 2, 2, 2, 2, 2, 2, 2, 2, 2, 2, 2, 2, 2, 2, 2, 2, 2, 2, 2, 2, 2, 2, 2, 2, 2, 2, 2, 2, 2, 2, 2, 2, 2, 2, 2, 2, 2, 2, 2, 2, 2, 2, 2, 2, 2, 2, 2, 2, 2, 2, 2, 2, 2, 2, 2, 2, 2, 2, 2, 2, 2, 2, 2, 2, 2, 2, 2, 3 ),
 ( 0.000000000000000000, 1.000000000000000000 ),
 ( 0.000000000000000000, 0.01041666666666666609, 0.02083333333333333218, 0.03125000000000000000, 0.04166666666666666435, 0.05208333333333333565, 0.06250000000000000000, 0.07291666666666667129, 0.08333333333333332871, 0.09375000000000000000, 0.1041666666666666713, 0.1145833333333333287, 0.1250000000000000000, 0.1354166666666666574, 0.1458333333333333426, 0.1562500000000000000, 0.1666666666666666574, 0.1770833333333333426, 0.1875000000000000000, 0.1979166666666666574, 0.2083333333333333426, 0.2187500000000000000, 0.2291666666666666574, 0.2395833333333333426, 0.2500000000000000000, 0.2604166666666666852, 0.2708333333333333148, 0.2812500000000000000, 0.2916666666666666852, 0.3020833333333333148, 0.3125000000000000000, 0.3229166666666666852, 0.3333333333333333148, 0.3437500000000000000, 0.3541666666666666852, 0.3645833333333333148, 0.3750000000000000000, 0.3854166666666666852, 0.3958333333333333148, 0.4062500000000000000, 0.4166666666666666852, 0.4270833333333333148, 0.4375000000000000000, 0.4479166666666666852, 0.4583333333333333148, 0.4687500000000000000, 0.4791666666666666852, 0.4895833333333333148, 0.5000000000000000000, 0.5104166666666666297, 0.5208333333333333703, 0.5312500000000000000, 0.5416666666666666297, 0.5520833333333333703, 0.5625000000000000000, 0.5729166666666666297, 0.5833333333333333703, 0.5937500000000000000, 0.6041666666666666297, 0.6145833333333333703, 0.6250000000000000000, 0.6354166666666666297, 0.6458333333333333703, 0.6562500000000000000, 0.6666666666666666297, 0.6770833333333333703, 0.6875000000000000000, 0.6979166666666666297, 0.7083333333333333703, 0.7187500000000000000, 0.7291666666666666297, 0.7395833333333333703, 0.7500000000000000000, 0.7604166666666666297, 0.7708333333333333703, 0.7812500000000000000, 0.7916666666666666297, 0.8020833333333333703, 0.8125000000000000000, 0.8229166666666666297, 0.8333333333333333703, 0.8437500000000000000, 0.8541666666666666297, 0.8645833333333333703, 0.8750000000000000000, 0.8854166666666666297, 0.8958333333333333703, 0.9062500000000000000, 0.9166666666666666297, 0.9270833333333333703, 0.9375000000000000000, 0.9448586968893691873 ),
 .UNSPECIFIED. ) 
 GEOMETRIC_REPRESENTATION_ITEM ( )  RATIONAL_B_SPLINE_SURFACE ( (
 ( 1.000000000000000000, 0.9238795325112867385, 1.000000000000000000, 0.9238795325112867385, 1.000000000000000000, 0.9238795325112867385, 1.000000000000000000, 0.9238795325112867385, 1.000000000000000000, 0.9238795325112867385, 1.000000000000000000, 0.9238795325112867385, 1.000000000000000000, 0.9238795325112867385, 1.000000000000000000, 0.9238795325112867385, 1.000000000000000000, 0.9238795325112867385, 1.000000000000000000, 0.9238795325112867385, 1.000000000000000000, 0.9238795325112867385, 1.000000000000000000, 0.9238795325112867385, 1.000000000000000000, 0.9238795325112867385, 1.000000000000000000, 0.9238795325112867385, 1.000000000000000000, 0.9238795325112867385, 1.000000000000000000, 0.9238795325112867385, 1.000000000000000000, 0.9238795325112867385, 1.000000000000000000, 0.9238795325112867385, 1.000000000000000000, 0.9238795325112867385, 1.000000000000000000, 0.9238795325112867385, 1.000000000000000000, 0.9238795325112867385, 1.000000000000000000, 0.9238795325112867385, 1.000000000000000000, 0.9238795325112867385, 1.000000000000000000, 0.9238795325112867385, 1.000000000000000000, 0.9238795325112867385, 1.000000000000000000, 0.9238795325112867385, 1.000000000000000000, 0.9238795325112867385, 1.000000000000000000, 0.9238795325112867385, 1.000000000000000000, 0.9238795325112867385, 1.000000000000000000, 0.9238795325112867385, 1.000000000000000000, 0.9238795325112867385, 1.000000000000000000, 0.9238795325112867385, 1.000000000000000000, 0.9238795325112867385, 1.000000000000000000, 0.9238795325112867385, 1.000000000000000000, 0.9238795325112867385, 1.000000000000000000, 0.9238795325112867385, 1.000000000000000000, 0.9238795325112867385, 1.000000000000000000, 0.9238795325112867385, 1.000000000000000000, 0.9238795325112867385, 1.000000000000000000, 0.9238795325112867385, 1.000000000000000000, 0.9238795325112867385, 1.000000000000000000, 0.9238795325112867385, 1.000000000000000000, 0.9238795325112867385, 1.000000000000000000, 0.9238795325112867385, 1.000000000000000000, 0.9238795325112867385, 1.000000000000000000, 0.9238795325112867385, 1.000000000000000000, 0.9238795325112867385, 1.000000000000000000, 0.9238795325112867385, 1.000000000000000000, 0.9238795325112867385, 1.000000000000000000, 0.9238795325112867385, 1.000000000000000000, 0.9238795325112867385, 1.000000000000000000, 0.9238795325112867385, 1.000000000000000000, 0.9238795325112867385, 1.000000000000000000, 0.9238795325112867385, 1.000000000000000000, 0.9238795325112867385, 1.000000000000000000, 0.9238795325112867385, 1.000000000000000000, 0.9238795325112867385, 1.000000000000000000, 0.9238795325112867385, 1.000000000000000000, 0.9238795325112867385, 1.000000000000000000, 0.9238795325112867385, 1.000000000000000000, 0.9238795325112867385, 1.000000000000000000, 0.9238795325112867385, 1.000000000000000000, 0.9238795325112867385, 1.000000000000000000, 0.9238795325112867385, 1.000000000000000000, 0.9238795325112867385, 1.000000000000000000, 0.9238795325112867385, 1.000000000000000000, 0.9238795325112867385, 1.000000000000000000, 0.9238795325112867385, 1.000000000000000000, 0.9238795325112867385, 1.000000000000000000, 0.9238795325112867385, 1.000000000000000000, 0.9238795325112867385, 1.000000000000000000, 0.9238795325112867385, 1.000000000000000000, 0.9238795325112867385, 1.000000000000000000, 0.9238795325112867385, 1.000000000000000000, 0.9238795325112867385, 1.000000000000000000, 0.9238795325112867385, 1.000000000000000000, 0.9238795325112867385, 1.000000000000000000, 0.9238795325112867385, 1.000000000000000000, 0.9238795325112867385, 1.000000000000000000, 0.9238795325112867385, 1.000000000000000000, 0.9238795325112867385, 1.000000000000000000, 0.9238795325112867385, 1.000000000000000000, 0.9238795325112867385, 1.000000000000000000, 0.9238795325112867385, 1.000000000000000000, 0.9238795325112867385, 1.000000000000000000, 0.9238795325112867385, 1.000000000000000000, 0.9238795325112867385, 1.000000000000000000, 0.9238795325112867385, 1.000000000000000000, 0.9238795325112867385, 1.000000000000000000, 0.9238795325112867385, 1.000000000000000000, 0.9462258450566536361, 0.9684275698016389100),
 ( 1.000000000000000000, 0.9238795325112867385, 1.000000000000000000, 0.9238795325112867385, 1.000000000000000000, 0.9238795325112867385, 1.000000000000000000, 0.9238795325112867385, 1.000000000000000000, 0.9238795325112867385, 1.000000000000000000, 0.9238795325112867385, 1.000000000000000000, 0.9238795325112867385, 1.000000000000000000, 0.9238795325112867385, 1.000000000000000000, 0.9238795325112867385, 1.000000000000000000, 0.9238795325112867385, 1.000000000000000000, 0.9238795325112867385, 1.000000000000000000, 0.9238795325112867385, 1.000000000000000000, 0.9238795325112867385, 1.000000000000000000, 0.9238795325112867385, 1.000000000000000000, 0.9238795325112867385, 1.000000000000000000, 0.9238795325112867385, 1.000000000000000000, 0.9238795325112867385, 1.000000000000000000, 0.9238795325112867385, 1.000000000000000000, 0.9238795325112867385, 1.000000000000000000, 0.9238795325112867385, 1.000000000000000000, 0.9238795325112867385, 1.000000000000000000, 0.9238795325112867385, 1.000000000000000000, 0.9238795325112867385, 1.000000000000000000, 0.9238795325112867385, 1.000000000000000000, 0.9238795325112867385, 1.000000000000000000, 0.9238795325112867385, 1.000000000000000000, 0.9238795325112867385, 1.000000000000000000, 0.9238795325112867385, 1.000000000000000000, 0.9238795325112867385, 1.000000000000000000, 0.9238795325112867385, 1.000000000000000000, 0.9238795325112867385, 1.000000000000000000, 0.9238795325112867385, 1.000000000000000000, 0.9238795325112867385, 1.000000000000000000, 0.9238795325112867385, 1.000000000000000000, 0.9238795325112867385, 1.000000000000000000, 0.9238795325112867385, 1.000000000000000000, 0.9238795325112867385, 1.000000000000000000, 0.9238795325112867385, 1.000000000000000000, 0.9238795325112867385, 1.000000000000000000, 0.9238795325112867385, 1.000000000000000000, 0.9238795325112867385, 1.000000000000000000, 0.9238795325112867385, 1.000000000000000000, 0.9238795325112867385, 1.000000000000000000, 0.9238795325112867385, 1.000000000000000000, 0.9238795325112867385, 1.000000000000000000, 0.9238795325112867385, 1.000000000000000000, 0.9238795325112867385, 1.000000000000000000, 0.9238795325112867385, 1.000000000000000000, 0.9238795325112867385, 1.000000000000000000, 0.9238795325112867385, 1.000000000000000000, 0.9238795325112867385, 1.000000000000000000, 0.9238795325112867385, 1.000000000000000000, 0.9238795325112867385, 1.000000000000000000, 0.9238795325112867385, 1.000000000000000000, 0.9238795325112867385, 1.000000000000000000, 0.9238795325112867385, 1.000000000000000000, 0.9238795325112867385, 1.000000000000000000, 0.9238795325112867385, 1.000000000000000000, 0.9238795325112867385, 1.000000000000000000, 0.9238795325112867385, 1.000000000000000000, 0.9238795325112867385, 1.000000000000000000, 0.9238795325112867385, 1.000000000000000000, 0.9238795325112867385, 1.000000000000000000, 0.9238795325112867385, 1.000000000000000000, 0.9238795325112867385, 1.000000000000000000, 0.9238795325112867385, 1.000000000000000000, 0.9238795325112867385, 1.000000000000000000, 0.9238795325112867385, 1.000000000000000000, 0.9238795325112867385, 1.000000000000000000, 0.9238795325112867385, 1.000000000000000000, 0.9238795325112867385, 1.000000000000000000, 0.9238795325112867385, 1.000000000000000000, 0.9238795325112867385, 1.000000000000000000, 0.9238795325112867385, 1.000000000000000000, 0.9238795325112867385, 1.000000000000000000, 0.9238795325112867385, 1.000000000000000000, 0.9238795325112867385, 1.000000000000000000, 0.9238795325112867385, 1.000000000000000000, 0.9238795325112867385, 1.000000000000000000, 0.9238795325112867385, 1.000000000000000000, 0.9238795325112867385, 1.000000000000000000, 0.9238795325112867385, 1.000000000000000000, 0.9238795325112867385, 1.000000000000000000, 0.9238795325112867385, 1.000000000000000000, 0.9238795325112867385, 1.000000000000000000, 0.9238795325112867385, 1.000000000000000000, 0.9238795325112867385, 1.000000000000000000, 0.9238795325112867385, 1.000000000000000000, 0.9238795325112867385, 1.000000000000000000, 0.9238795325112867385, 1.000000000000000000, 0.9462258450566536361, 0.9684275698016389100) ) ) 
 REPRESENTATION_ITEM ( '' )  SURFACE ( )  );
#5236 = CARTESIAN_POINT ( 'NONE',  ( 104.9999999999999716, 1.449011120738813565E-14, 11.62500000273118417 ) ) ;
#5237 = CARTESIAN_POINT ( 'NONE',  ( 116.8548138422182063, 32.56640625108394005, -5.444914386472297529 ) ) ;
#5238 = CARTESIAN_POINT ( 'NONE',  ( 65.00000000000000000, 31.37578125216787583, -13.57481594606304576 ) ) ;
#5239 = DIRECTION ( 'NONE',  ( -0.000000000000000000, 1.000000000000000000, -0.000000000000000000 ) ) ;
#5240 = CARTESIAN_POINT ( 'NONE',  ( -5.444914386472299306, 37.52734375108393294, 13.14518615778179722 ) ) ;
#5241 = DIRECTION ( 'NONE',  ( -0.000000000000000000, -0.000000000000000000, -1.000000000000000000 ) ) ;
#5242 = CARTESIAN_POINT ( 'NONE',  ( 104.9999999999999716, 1.449011120738813565E-14, 1.499999999999999556 ) ) ;
#5243 = CARTESIAN_POINT ( 'NONE',  ( 102.4976396683250783, 117.6869444889999841, -54.47499999726881725 ) ) ;
#5244 = VECTOR ( 'NONE', #10779, 1000.000000000000000 ) ;
#5245 = PLANE ( 'NONE',  #22570 ) ;
#5246 = CARTESIAN_POINT ( 'NONE',  ( 181.8548138422181921, 32.56640625108394005, -5.444914386472297529 ) ) ;
#5247 = CARTESIAN_POINT ( 'NONE',  ( 96.46446609406721961, 3.535533905932755072, 6.000000002731185056 ) ) ;
#5248 = CARTESIAN_POINT ( 'NONE',  ( 98.96446609406727646, 124.0569999999781459, -2.499999999999997780 ) ) ;
#5249 = CARTESIAN_POINT ( 'NONE',  ( 97.93301269999999192, 123.7000000010924765, -0.8561741729129505041 ) ) ;
#5250 = CARTESIAN_POINT ( 'NONE',  ( 129.8277102352230656, 36.00000000000000000, -13.51468191220836523 ) ) ;
#5251 = CYLINDRICAL_SURFACE ( 'NONE', #19521, 23.00000000000001421 ) ;
#5252 = CARTESIAN_POINT ( 'NONE',  ( 84.99999999999998579, 100.0000000000000000, -15.00000000000000533 ) ) ;
#5253 = CARTESIAN_POINT ( 'NONE',  ( 5.622872871577871301, 33.60820312499998863, -13.57481594606304753 ) ) ;
#5254 = CARTESIAN_POINT ( 'NONE',  ( 13.57481594606304931, 40.55351562499999574, 5.622872871577868636 ) ) ;
#5255 = CARTESIAN_POINT ( 'NONE',  ( -13.14518615778179544, 32.81445312608393294, 0.000000000000000000 ) ) ;
#5256 = CARTESIAN_POINT ( 'NONE',  ( -5.444914386472297529, 34.05468750108393294, -13.14518615778179900 ) ) ;
#5257 = CARTESIAN_POINT ( 'NONE',  ( -5.444914386472297529, 34.84843750108393579, -13.14518615778179722 ) ) ;
#5258 = CARTESIAN_POINT ( 'NONE',  ( 2.493653234604083739E-15, 37.32890625216786873, 13.57481594606304576 ) ) ;
#5259 = CARTESIAN_POINT ( 'NONE',  ( -8.312177448680279460E-16, 37.62656249999999858, -13.57481594606304576 ) ) ;
#5260 = CARTESIAN_POINT ( 'NONE',  ( 95.54126587499995082, 82.37500000136562051, -1.846868145590750077 ) ) ;
#5261 = CARTESIAN_POINT ( 'NONE',  ( 59.55508561352770158, 32.76484375108393010, 13.14518615778179722 ) ) ;
#5262 = CARTESIAN_POINT ( 'NONE',  ( 0.000000000000000000, 40.99999999999999289, -13.57481594606304576 ) ) ;
#5263 = CARTESIAN_POINT ( 'NONE',  ( -13.36000105192242060, 40.42949218912590936, 0.000000000000000000 ) ) ;
#5264 = CARTESIAN_POINT ( 'NONE',  ( 13.57481594606304753, 37.47773437500001137, -5.622872871577873966 ) ) ;
#5265 = CARTESIAN_POINT ( 'NONE',  ( -8.312177448680279460E-16, 32.86406249999999574, -13.57481594606304576 ) ) ;
#5266 = CARTESIAN_POINT ( 'NONE',  ( 135.4449143864723055, 34.15390625108393863, -13.14518615778179900 ) ) ;
#5267 = ORIENTED_EDGE ( 'NONE', *, *, #12792, .T. ) ;
#5268 = CARTESIAN_POINT ( 'NONE',  ( 99.99999999999998579, 110.0000000000000000, -145.0000000000000284 ) ) ;
#5269 = EDGE_CURVE ( 'NONE', #18860, #22175, #2047, .T. ) ;
#5270 = CARTESIAN_POINT ( 'NONE',  ( 105.6631189606246153, 114.1144967660473242, -47.80000000000001137 ) ) ;
#5271 = CARTESIAN_POINT ( 'NONE',  ( 98.15313185440925281, 83.25000000136560629, -4.458734125000016313 ) ) ;
#5272 = CARTESIAN_POINT ( 'NONE',  ( 102.0710678118654613, 93.18749999999998579, -4.999999999999997335 ) ) ;
#5273 = CARTESIAN_POINT ( 'NONE',  ( 204.5988444088204403, 37.52734375000000000, -9.598844408820458085 ) ) ;
#5274 = CARTESIAN_POINT ( 'NONE',  ( 102.4976396683250783, 117.6869444889999841, -46.22499999726882436 ) ) ;
#5275 = CARTESIAN_POINT ( 'NONE',  ( 189.5550856135277229, 39.80937500108392868, -13.14518615778179900 ) ) ;
#5276 = CARTESIAN_POINT ( 'NONE',  ( 2.493653234604083739E-15, 38.91640625216786731, 13.57481594606304576 ) ) ;
#5277 = VECTOR ( 'NONE', #18537, 1000.000000000000000 ) ;
#5278 = AXIS2_PLACEMENT_3D ( 'NONE', #4877, #9563, #13541 ) ;
#5279 = ORIENTED_EDGE ( 'NONE', *, *, #899, .T. ) ;
#5280 = CARTESIAN_POINT ( 'NONE',  ( 193.1834995827137504, 36.00000000000001421, -13.35830014193466653 ) ) ;
#5281 = CARTESIAN_POINT ( 'NONE',  ( 99.99999999999995737, -4.999999999999990230, 13.25000000000000000 ) ) ;
#5282 = ORIENTED_EDGE ( 'NONE', *, *, #14339, .T. ) ;
#5283 = CARTESIAN_POINT ( 'NONE',  ( 13.14518615778179544, 34.79882812608394005, -1.609821015232357215E-15 ) ) ;
#5284 = CARTESIAN_POINT ( 'NONE',  ( 189.5550856135277229, 39.90859375108393436, 13.14518615778179722 ) ) ;
#5285 = CARTESIAN_POINT ( 'NONE',  ( 5.444914386472297529, 33.95546875108394147, -13.14518615778179722 ) ) ;
#5286 = CARTESIAN_POINT ( 'NONE',  ( 97.92893218813451028, 5.000000000000018652, 12.93750000273118772 ) ) ;
#5287 = CARTESIAN_POINT ( 'NONE',  ( 104.9999999999999716, 1.449011120738813565E-14, 34.79898987322334136 ) ) ;
#5288 = CARTESIAN_POINT ( 'NONE',  ( 9.295050272127046043, 33.31054687608394005, -9.295050272127046043 ) ) ;
#5289 =( BOUNDED_CURVE ( )  B_SPLINE_CURVE ( 2, ( #22354, #26783, #267, #26639, #17500, #19642, #24207, #412, #7086 ),
 .UNSPECIFIED., .F., .T. ) 
 B_SPLINE_CURVE_WITH_KNOTS ( ( 3, 2, 2, 2, 3 ),
 ( 0.2708333333333330928, 0.2812499999999998890, 0.2916666666666666852, 0.3020833333333334259, 0.3125000000000002220 ),
 .UNSPECIFIED. ) 
 CURVE ( )  GEOMETRIC_REPRESENTATION_ITEM ( )  RATIONAL_B_SPLINE_CURVE ( ( 1.000000000000001554, 0.9238795325112850731, 1.000000000000000000, 0.9238795325112867385, 1.000000000000000000, 0.9238795325112867385, 1.000000000000000000, 0.9238795325112850731, 1.000000000000001554 ) ) 
 REPRESENTATION_ITEM ( '' )  );
#5290 = CARTESIAN_POINT ( 'NONE',  ( 139.2950502721270425, 32.11992187608393579, 9.295050272127046043 ) ) ;
#5291 = CARTESIAN_POINT ( 'NONE',  ( 95.54126587500000767, 91.81249999863440792, -7.484931351350258973E-15 ) ) ;
#5292 = CARTESIAN_POINT ( 'NONE',  ( 97.50000000000000000, 125.0000000000000000, -9.540979117872439019E-15 ) ) ;
#5293 = CARTESIAN_POINT ( 'NONE',  ( 0.000000000000000000, 0.000000000000000000, 0.000000000000000000 ) ) ;
#5294 = CARTESIAN_POINT ( 'NONE',  ( -13.36000105192242060, 40.87597656304196647, 0.000000000000000000 ) ) ;
#5295 = CARTESIAN_POINT ( 'NONE',  ( 101.8468681455906903, -4.458734124999987891, 6.000000001365591196 ) ) ;
#5296 = CARTESIAN_POINT ( 'NONE',  ( 97.50000000000000000, 123.3999999999999915, -9.540979117872439019E-15 ) ) ;
#5297 = CARTESIAN_POINT ( 'NONE',  ( 95.54126587499996504, 1.387778780781445676E-14, 11.43750000136559208 ) ) ;
#5298 = CARTESIAN_POINT ( 'NONE',  ( 106.5389055433251002, 105.2492070361643215, -48.32500000273119412 ) ) ;
#5299 = CARTESIAN_POINT ( 'NONE',  ( 103.1528011352953484, 92.68749999863440792, -3.152801135295366208 ) ) ;
#5300 = VECTOR ( 'NONE', #5371, 1000.000000000000000 ) ;
#5301 = DIRECTION ( 'NONE',  ( -0.000000000000000000, 1.000000000000000000, 0.000000000000000000 ) ) ;
#5302 = CARTESIAN_POINT ( 'NONE',  ( 102.4976396683250783, 102.3130555110000159, -53.02499999726882862 ) ) ;
#5303 = CARTESIAN_POINT ( 'NONE',  ( 2.414731522848535132E-15, 34.60039062608393579, 13.14518615778179544 ) ) ;
#5304 = ORIENTED_EDGE ( 'NONE', *, *, #17554, .T. ) ;
#5305 = DIRECTION ( 'NONE',  ( 0.000000000000000000, 0.000000000000000000, 1.000000000000000000 ) ) ;
#5307 = EDGE_CURVE ( 'NONE', #9633, #9529, #10293, .T. ) ;
#5306 = CARTESIAN_POINT ( 'NONE',  ( 13.57481594606304931, 39.85898437716787157, 5.622872871577868636 ) ) ;
#5308 = FACE_OUTER_BOUND ( 'NONE', #1978, .T. ) ;
#5309 = ADVANCED_FACE ( 'NONE', ( #21289 ), #19030, .T. ) ;
#5310 = CARTESIAN_POINT ( 'NONE',  ( 200.4449143864723055, 35.54296875108393294, -13.14518615778179900 ) ) ;
#5311 = VERTEX_POINT ( 'NONE', #18832 ) ;
#5312 = CARTESIAN_POINT ( 'NONE',  ( 193.1078166429076077, 53.66387243067951829, -15.00000000000000178 ) ) ;
#5313 = CARTESIAN_POINT ( 'NONE',  ( 103.1528011352953342, 3.152801135295383084, 11.31250000136559386 ) ) ;
#5314 = ORIENTED_EDGE ( 'NONE', *, *, #24130, .T. ) ;
#5315 = CARTESIAN_POINT ( 'NONE',  ( 97.83688103937537051, 103.3426043859339103, -45.60000000000000853 ) ) ;
#5316 = CARTESIAN_POINT ( 'NONE',  ( -9.295050272127044266, 35.09648437608392868, 9.295050272127047819 ) ) ;
#5317 = VECTOR ( 'NONE', #20065, 1000.000000000000000 ) ;
#5318 = CARTESIAN_POINT ( 'NONE',  ( 195.0000000000000000, 38.51953125216787299, -13.57481594606304576 ) ) ;
#5319 = CARTESIAN_POINT ( 'NONE',  ( 130.0000000000000000, -7.395377635281828788, -13.57481594606305997 ) ) ;
#5320 = EDGE_CURVE ( 'NONE', #5488, #3371, #21257, .T. ) ;
#5321 = CARTESIAN_POINT ( 'NONE',  ( 130.0000000000000000, 37.97382812608393721, -13.14518615778179544 ) ) ;
#5322 = CARTESIAN_POINT ( 'NONE',  ( 13.14518615778179722, 36.43593750108394147, -5.444914386472297529 ) ) ;
#5323 = CARTESIAN_POINT ( 'NONE',  ( 5.444914386472302859, 35.24531250108393010, 13.14518615778179189 ) ) ;
#5324 = CARTESIAN_POINT ( 'NONE',  ( 95.54126587500000767, 92.06249999863440792, -7.484931351350258973E-15 ) ) ;
#5325 = CARTESIAN_POINT ( 'NONE',  ( 73.21131401517213533, 50.68678854790645261, -15.00000000000000000 ) ) ;
#5326 = ORIENTED_EDGE ( 'NONE', *, *, #7051, .F. ) ;
#5327 = CARTESIAN_POINT ( 'NONE',  ( -13.14518615778179544, 34.40195312608393152, 0.000000000000000000 ) ) ;
#5328 = CARTESIAN_POINT ( 'NONE',  ( 104.4587341249999639, 1.442382525525748735E-14, 7.187500001365592972 ) ) ;
#5329 = CONICAL_SURFACE ( 'NONE', #11688, 11.50000000000001776, 0.7853981633974473908 ) ;
#5330 = CARTESIAN_POINT ( 'NONE',  ( 59.55508561352770158, 36.73359375108393010, 13.14518615778179722 ) ) ;
#5331 = CARTESIAN_POINT ( 'NONE',  ( 103.5355339059327093, 3.535533905932755072, 6.750000002731185056 ) ) ;
#5332 = CARTESIAN_POINT ( 'NONE',  ( 51.42518405393695957, 38.66835937499999432, 5.622872871577880183 ) ) ;
#5333 = CARTESIAN_POINT ( 'NONE',  ( 185.7049497278729575, 37.27929687608393294, -9.295050272127046043 ) ) ;
#5334 = CARTESIAN_POINT ( 'NONE',  ( -13.14518615778179189, 36.03906250108393294, 5.444914386472304635 ) ) ;
#5336 = EDGE_CURVE ( 'NONE', #12117, #8914, #3398, .T. ) ;
#5335 = CARTESIAN_POINT ( 'NONE',  ( 102.0669872999999939, 124.2000000010924907, -0.8561741729129507261 ) ) ;
#5337 = CARTESIAN_POINT ( 'NONE',  ( 95.54126587499999346, 92.12499999863440792, 1.846868145590722543 ) ) ;
#5338 = CARTESIAN_POINT ( 'NONE',  ( 200.4449143864723055, 37.03125000108393294, 13.14518615778179189 ) ) ;
#5339 = CARTESIAN_POINT ( 'NONE',  ( 108.0825317499999869, 107.3738262389971538, -46.97499999726881015 ) ) ;
#5340 = CARTESIAN_POINT ( 'NONE',  ( -9.598844408820454532, 32.36796874999999574, 9.598844408820459861 ) ) ;
#5341 = CARTESIAN_POINT ( 'NONE',  ( 13.14518615778179544, 35.39414062608393152, -1.609821015232357215E-15 ) ) ;
#5342 = ORIENTED_EDGE ( 'NONE', *, *, #24287, .F. ) ;
#5343 = CARTESIAN_POINT ( 'NONE',  ( 120.7049497278729575, 32.91367187608393152, 9.295050272127047819 ) ) ;
#5344 = CARTESIAN_POINT ( 'NONE',  ( 7.095734625815413921, 31.38770419771516629, -11.40432331644931629 ) ) ;
#5345 = ADVANCED_FACE ( 'NONE', ( #4010 ), #28091, .T. ) ;
#5346 = FACE_OUTER_BOUND ( 'NONE', #663, .T. ) ;
#5347 = CARTESIAN_POINT ( 'NONE',  ( 208.1451861577817795, 34.05468750108394005, -5.444914386472297529 ) ) ;
#5348 = ORIENTED_EDGE ( 'NONE', *, *, #7139, .T. ) ;
#5349 = CARTESIAN_POINT ( 'NONE',  ( 98.53841926354351699, 123.8500000010924680, 1.461580736456455920 ) ) ;
#5350 = CARTESIAN_POINT ( 'NONE',  ( 94.99999999999995737, 2.071067811865500818, 9.062500002731182391 ) ) ;
#5351 = CARTESIAN_POINT ( 'NONE',  ( 120.8198241863519939, 49.99999999999998579, -14.99999999999999645 ) ) ;
#5352 = VECTOR ( 'NONE', #24906, 1000.000000000000000 ) ;
#5353 = EDGE_CURVE ( 'NONE', #20971, #22337, #12113, .T. ) ;
#5354 = CARTESIAN_POINT ( 'NONE',  ( 130.0000000000000000, 37.72578125216787726, -13.57481594606304576 ) ) ;
#5355 = CARTESIAN_POINT ( 'NONE',  ( 106.5389055433251002, 114.7507929638356785, -47.92500000273120264 ) ) ;
#5356 = DIRECTION ( 'NONE',  ( 0.000000000000000000, 1.000000000000000000, -1.156482317317871478E-16 ) ) ;
#5357 = CARTESIAN_POINT ( 'NONE',  ( 68.97981444581395749, 50.00000000123263533, 13.01613927312710040 ) ) ;
#5358 = ORIENTED_EDGE ( 'NONE', *, *, #16341, .T. ) ;
#5359 = CARTESIAN_POINT ( 'NONE',  ( 101.8468681455906903, 4.458734125000016313, 5.125000001365592972 ) ) ;
#5360 = VERTEX_POINT ( 'NONE', #1254 ) ;
#5361 = CARTESIAN_POINT ( 'NONE',  ( -3.420220812170877700, 35.99999999999999289, -13.02105590829194348 ) ) ;
#5362 = CARTESIAN_POINT ( 'NONE',  ( 103.1528011352953342, 3.152801135295383084, 8.062500001365592084 ) ) ;
#5363 = CARTESIAN_POINT ( 'NONE',  ( 139.1801758136480203, 55.00000000000000711, 14.99999999999996092 ) ) ;
#5364 = CARTESIAN_POINT ( 'NONE',  ( 103.5355339059327235, 94.74999999726881583, 3.535533905932724874 ) ) ;
#5365 = CARTESIAN_POINT ( 'NONE',  ( 51.85481384221819923, 32.76484375108393010, -5.444914386472297529 ) ) ;
#5366 = CARTESIAN_POINT ( 'NONE',  ( 94.99999999999997158, -2.071067811865486608, 5.062499999999999112 ) ) ;
#5367 = CARTESIAN_POINT ( 'NONE',  ( 104.9952793366501851, 116.8754121666685393, -47.82500000273119412 ) ) ;
#5368 = CARTESIAN_POINT ( 'NONE',  ( -5.622872871577839327, 38.76757812499998579, 13.57481594606308128 ) ) ;
#5369 = AXIS2_PLACEMENT_3D ( 'NONE', #13301, #17455, #11028 ) ;
#5370 = VECTOR ( 'NONE', #7859, 1000.000000000000000 ) ;
#5371 = DIRECTION ( 'NONE',  ( 0.000000000000000000, -1.000000000000000000, 0.000000000000000000 ) ) ;
#5372 = CARTESIAN_POINT ( 'NONE',  ( -6.450879342660423177, 50.00000000106947340, 11.97362904075749235 ) ) ;
#5373 = DIRECTION ( 'NONE',  ( 1.000000000000000000, 0.000000000000000000, -0.000000000000000000 ) ) ;
#5374 = CARTESIAN_POINT ( 'NONE',  ( 139.5988444088204403, 34.35234374999999574, -9.598844408820458085 ) ) ;
#5375 = ORIENTED_EDGE ( 'NONE', *, *, #22515, .T. ) ;
#5376 = CARTESIAN_POINT ( 'NONE',  ( -8.312177448680279460E-16, 40.10703125216787157, -13.57481594606304576 ) ) ;
#5377 = CARTESIAN_POINT ( 'NONE',  ( -8.049105076161786076E-16, 34.20351562608394147, -13.14518615778179544 ) ) ;
#5378 = CARTESIAN_POINT ( 'NONE',  ( -13.57481594606304753, 35.49335937716787015, -5.622872871577873077 ) ) ;
#5379 = CARTESIAN_POINT ( 'NONE',  ( 96.46446609406721961, -3.535533905932727539, 6.250000002731185056 ) ) ;
#5380 = CARTESIAN_POINT ( 'NONE',  ( 116.8548138422182063, 33.36015625108393579, -5.444914386472297529 ) ) ;
#5381 = CARTESIAN_POINT ( 'NONE',  ( 55.40115559117954547, 31.47500000216787441, -9.598844408820458085 ) ) ;
#5382 = EDGE_CURVE ( 'NONE', #25436, #23888, #22103, .T. ) ;
#5383 = CARTESIAN_POINT ( 'NONE',  ( -13.14518615778179189, 39.80937500108392868, 5.444914386472304635 ) ) ;
#5384 = CARTESIAN_POINT ( 'NONE',  ( 87.00000000000000000, 102.0000000000000142, -13.00000000000000533 ) ) ;
#5385 = CARTESIAN_POINT ( 'NONE',  ( 195.0000000000000000, -7.395377635281828788, 13.57481594606302266 ) ) ;
#5386 = CARTESIAN_POINT ( 'NONE',  ( 108.0825317499999869, 112.6261737610028320, -54.77499999726881441 ) ) ;
#5387 = ORIENTED_EDGE ( 'NONE', *, *, #24994, .F. ) ;
#5388 = CARTESIAN_POINT ( 'NONE',  ( -5.622872871577873077, 38.07304687716787583, 13.57481594606304753 ) ) ;
#5389 = CARTESIAN_POINT ( 'NONE',  ( 189.5550856135277229, 31.97109375108393436, 13.14518615778179722 ) ) ;
#5390 = CARTESIAN_POINT ( 'NONE',  ( 139.0314404224549207, 36.00000000000000000, 9.765766397118452957 ) ) ;
#5391 = CARTESIAN_POINT ( 'NONE',  ( 97.50000000000000000, 124.9569999999781658, -1.035533905932742416 ) ) ;
#5392 = AXIS2_PLACEMENT_3D ( 'NONE', #15036, #15174, #17609 ) ;
#5393 = CARTESIAN_POINT ( 'NONE',  ( 98.53841926354351699, 123.0500000010924850, 1.461580736456455920 ) ) ;
#5394 = CARTESIAN_POINT ( 'NONE',  ( 118.3096217544866704, 36.00000000000001421, -6.307928093363107891 ) ) ;
#5395 = CARTESIAN_POINT ( 'NONE',  ( 93.00000000000000000, 110.0000000000000000, -48.00000000000000711 ) ) ;
#5396 = DIRECTION ( 'NONE',  ( 5.782411586589358625E-17, -0.000000000000000000, 1.000000000000000000 ) ) ;
#5397 = CARTESIAN_POINT ( 'NONE',  ( -13.57481594606304576, 33.90585937500000568, 5.622872871577880183 ) ) ;
#5398 = CARTESIAN_POINT ( 'NONE',  ( -12.85950995607747949, 36.00000000000000711, -3.245221471867173246 ) ) ;
#5399 = CARTESIAN_POINT ( 'NONE',  ( -5.444914386472297529, 34.25312500108393010, -13.14518615778179900 ) ) ;
#5400 = CARTESIAN_POINT ( 'NONE',  ( -13.14518615778179189, 31.87187500108393223, 5.444914386472304635 ) ) ;
#5401 = CARTESIAN_POINT ( 'NONE',  ( 204.5988444088204687, 32.56640625000000000, 9.598844408820456309 ) ) ;
#5402 = CARTESIAN_POINT ( 'NONE',  ( 2.493653234604083739E-15, 35.74140625216787015, 13.57481594606304576 ) ) ;
#5403 = CARTESIAN_POINT ( 'NONE',  ( 2.493653234604083739E-15, 37.32890625216786873, 13.57481594606304576 ) ) ;
#5404 = CARTESIAN_POINT ( 'NONE',  ( 104.4587341249999639, 83.93750000136560629, -1.442382525525748735E-14 ) ) ;
#5405 = CARTESIAN_POINT ( 'NONE',  ( 78.14518615778179367, 32.21914062608393436, -1.609821015232357215E-15 ) ) ;
#5406 = FACE_OUTER_BOUND ( 'NONE', #26194, .T. ) ;
#5407 = CARTESIAN_POINT ( 'NONE',  ( 105.6631189606246295, 105.8855032339526758, -46.20000000000000995 ) ) ;
#5408 =( BOUNDED_CURVE ( )  B_SPLINE_CURVE ( 2, ( #27891, #8352, #23611, #4088, #12752, #18776, #14485, #21475, #1951, #16495, #25189 ),
 .UNSPECIFIED., .F., .F. ) 
 B_SPLINE_CURVE_WITH_KNOTS ( ( 3, 2, 2, 2, 2, 3 ),
 ( 0.4999999999999996669, 0.5199999999999996847, 0.5399999999999998135, 0.5599999999999998312, 0.5799999999999998490, 0.5999999999999998668 ),
 .UNSPECIFIED. ) 
 CURVE ( )  GEOMETRIC_REPRESENTATION_ITEM ( )  RATIONAL_B_SPLINE_CURVE ( ( 1.000000000000000888, 0.9510565162951527540, 1.000000000000000000, 0.9510565162951535312, 1.000000000000000000, 0.9510565162951535312, 1.000000000000000000, 0.9510565162951535312, 1.000000000000000000, 0.9510565162951537532, 0.9999999999999997780 ) ) 
 REPRESENTATION_ITEM ( '' )  );
#5409 = ORIENTED_EDGE ( 'NONE', *, *, #25699, .F. ) ;
#5410 = CARTESIAN_POINT ( 'NONE',  ( 99.14382582708707048, 123.6000000010924680, -2.066987299999999195 ) ) ;
#5411 = CARTESIAN_POINT ( 'NONE',  ( 214.9999999999999716, 80.00000000000000000, 9.999999999999946709 ) ) ;
#5412 = CARTESIAN_POINT ( 'NONE',  ( 93.46109445667489979, 105.2492070361643215, -53.67499999726882720 ) ) ;
#5413 = CARTESIAN_POINT ( 'NONE',  ( 120.7049497278729575, 34.50117187608393721, 9.295050272127047819 ) ) ;
#5414 = VERTEX_POINT ( 'NONE', #24904 ) ;
#5415 = CARTESIAN_POINT ( 'NONE',  ( 94.99999999999995737, 81.00000000000000000, -1.387778780781445676E-14 ) ) ;
#5416 = CARTESIAN_POINT ( 'NONE',  ( 1.662435489736055892E-15, 36.00000000000000000, 13.57481594606304576 ) ) ;
#5417 = CARTESIAN_POINT ( 'NONE',  ( 97.92893218813451028, 79.31250000273121259, 4.999999999999989342 ) ) ;
#5418 = CARTESIAN_POINT ( 'NONE',  ( 102.0710678118654613, 91.18749999999998579, -4.999999999999997335 ) ) ;
#5419 = CARTESIAN_POINT ( 'NONE',  ( 78.57481594606305464, 39.90859375216787441, -1.662435489736055892E-15 ) ) ;
#5420 = CIRCLE ( 'NONE', #21330, 13.57481594606304576 ) ;
#5421 = CARTESIAN_POINT ( 'NONE',  ( 97.50236033167490746, 102.3130555110000159, -47.22499999726881725 ) ) ;
#5422 = CARTESIAN_POINT ( 'NONE',  ( 204.2950502721270425, 40.45429687608393721, -9.295050272127046043 ) ) ;
#5423 = CARTESIAN_POINT ( 'NONE',  ( -13.57481594606304576, 37.92421875216787441, 0.000000000000000000 ) ) ;
#5424 = VERTEX_POINT ( 'NONE', #5384 ) ;
#5425 = CARTESIAN_POINT ( 'NONE',  ( 96.46446609406721961, 3.535533905932755072, 9.874999999999998224 ) ) ;
#5426 = VERTEX_POINT ( 'NONE', #7652 ) ;
#5427 = CARTESIAN_POINT ( 'NONE',  ( -13.14518615778179544, 37.57695312608393579, 0.000000000000000000 ) ) ;
#5428 = CARTESIAN_POINT ( 'NONE',  ( 208.5748159460630120, 32.81445312716787299, -5.622872871577873077 ) ) ;
#5429 = CARTESIAN_POINT ( 'NONE',  ( -13.14518615778179544, 31.82226562608393650, 0.000000000000000000 ) ) ;
#5430 = CARTESIAN_POINT ( 'NONE',  ( 103.5355339059327093, 3.535533905932755072, 11.75000000273118594 ) ) ;
#5431 = CARTESIAN_POINT ( 'NONE',  ( 124.5550856135277087, 39.90859375108392726, 13.14518615778179722 ) ) ;
#5432 = CARTESIAN_POINT ( 'NONE',  ( 9.295050272127047819, 32.31835937608393294, 9.295050272127046043 ) ) ;
#5433 = EDGE_CURVE ( 'NONE', #1189, #15184, #1608, .T. ) ;
#5434 = CARTESIAN_POINT ( 'NONE',  ( 102.1631189606246295, 103.3426043859339103, -49.90000000546238113 ) ) ;
#5435 = CARTESIAN_POINT ( 'NONE',  ( 104.4587341249999923, 90.37499999863440792, -1.846868145590737198 ) ) ;
#5436 = CARTESIAN_POINT ( 'NONE',  ( 102.0669872999999939, 123.6000000010924680, -0.8561741729129507261 ) ) ;
#5437 = FACE_OUTER_BOUND ( 'NONE', #780, .T. ) ;
#5438 = CARTESIAN_POINT ( 'NONE',  ( 104.4587341249999781, 1.846868145590750299, 7.250000001365591196 ) ) ;
#5439 = CARTESIAN_POINT ( 'NONE',  ( 107.0000000000000142, 110.0000000000000000, -53.50000000546238255 ) ) ;
#5440 = CARTESIAN_POINT ( 'NONE',  ( 104.4587341249999781, -1.846868145590721655, 8.875000001365592084 ) ) ;
#5441 = CARTESIAN_POINT ( 'NONE',  ( 107.0000000000000142, 110.0000000000000000, -51.50000000546237544 ) ) ;
#5442 = CARTESIAN_POINT ( 'NONE',  ( 97.50000000000000000, 124.3000000021849587, -9.540979117872439019E-15 ) ) ;
#5443 = CARTESIAN_POINT ( 'NONE',  ( 13.57481594606304753, 39.85898437499999858, -5.622872871577873966 ) ) ;
#5444 = AXIS2_PLACEMENT_3D ( 'NONE', #8711, #21840, #21976 ) ;
#5445 = CARTESIAN_POINT ( 'NONE',  ( 219.9999999999999716, 50.00000000000000000, -10.00000000000000000 ) ) ;
#5446 = CARTESIAN_POINT ( 'NONE',  ( -5.444914386472297529, 32.66562500108393863, -13.14518615778179900 ) ) ;
#5447 = ORIENTED_EDGE ( 'NONE', *, *, #15750, .F. ) ;
#5448 = FACE_OUTER_BOUND ( 'NONE', #6321, .T. ) ;
#5449 = DIRECTION ( 'NONE',  ( 0.000000000000000000, -1.000000000000000000, 0.000000000000000000 ) ) ;
#5450 = CARTESIAN_POINT ( 'NONE',  ( 208.1451861577817795, 33.75703125108393010, 5.444914386472293977 ) ) ;
#5451 = ORIENTED_EDGE ( 'NONE', *, *, #6166, .T. ) ;
#5452 = CARTESIAN_POINT ( 'NONE',  ( 185.8198241863519513, 50.00000000000000000, -9.999999999999960920 ) ) ;
#5453 = CARTESIAN_POINT ( 'NONE',  ( 103.1528011352953342, -3.152801135295355106, 12.06250000136559208 ) ) ;
#5454 = ORIENTED_EDGE ( 'NONE', *, *, #26500, .T. ) ;
#5455 = CARTESIAN_POINT ( 'NONE',  ( 108.0825317500000011, 107.3738262389971538, -46.47500000273117848 ) ) ;
#5456 =( BOUNDED_CURVE ( )  B_SPLINE_CURVE ( 2, ( #7067, #18046, #26474, #20339, #19910 ),
 .UNSPECIFIED., .F., .F. ) 
 B_SPLINE_CURVE_WITH_KNOTS ( ( 3, 2, 3 ),
 ( 0.000000000000000000, 0.01041666666666679446, 0.02083333333333358892 ),
 .UNSPECIFIED. ) 
 CURVE ( )  GEOMETRIC_REPRESENTATION_ITEM ( )  RATIONAL_B_SPLINE_CURVE ( ( 1.000000000000000000, 0.9238795325112867385, 1.000000000000000000, 0.9238795325112848511, 1.000000000000001776 ) ) 
 REPRESENTATION_ITEM ( '' )  );
#5457 = CARTESIAN_POINT ( 'NONE',  ( 9.295050272127047819, 37.67617187608393436, 9.295050272127046043 ) ) ;
#5458 = STYLED_ITEM ( 'NONE', ( #10864 ), #4607 ) ;
#5459 = CARTESIAN_POINT ( 'NONE',  ( 2.493653234604083739E-15, 38.81718749999999574, 13.57481594606304576 ) ) ;
#5460 = CARTESIAN_POINT ( 'NONE',  ( 116.8548138422182063, 38.12265625108393152, -5.444914386472297529 ) ) ;
#5461 = CARTESIAN_POINT ( 'NONE',  ( -13.14518615778179544, 37.57695312608393579, 0.000000000000000000 ) ) ;
#5462 = CARTESIAN_POINT ( 'NONE',  ( 13.14518615778179900, 40.30546875108393579, 5.444914386472293977 ) ) ;
#5463 = CARTESIAN_POINT ( 'NONE',  ( 99.99999999999998579, 92.31249999863440792, 4.458734124999981674 ) ) ;
#5464 = FACE_OUTER_BOUND ( 'NONE', #9049, .T. ) ;
#5465 = EDGE_CURVE ( 'NONE', #152, #5192, #1153, .T. ) ;
#5466 = CARTESIAN_POINT ( 'NONE',  ( 13.57481594606304576, 38.32109375216786873, -1.662435489736055892E-15 ) ) ;
#5467 = CYLINDRICAL_SURFACE ( 'NONE', #946, 5.000000000000004441 ) ;
#5468 = CARTESIAN_POINT ( 'NONE',  ( 104.4587341249999781, 1.846868145590750521, 6.250000001365592084 ) ) ;
#5469 = CARTESIAN_POINT ( 'NONE',  ( 96.84719886470459471, 82.81250000136560629, 3.152801135295355994 ) ) ;
#5470 = FACE_BOUND ( 'NONE', #18443, .T. ) ;
#5471 = CARTESIAN_POINT ( 'NONE',  ( 61.88340791953426390, 53.90895096933308395, 14.99999999999998046 ) ) ;
#5472 = CARTESIAN_POINT ( 'NONE',  ( 208.1451861577818079, 36.98164062608393010, -1.609821015232357215E-15 ) ) ;
#5473 = VERTEX_POINT ( 'NONE', #296 ) ;
#5474 = CARTESIAN_POINT ( 'NONE',  ( 9.295050272127047819, 35.49335937608393721, 9.295050272127046043 ) ) ;
#5475 = CARTESIAN_POINT ( 'NONE',  ( 98.53841926354351699, 123.8500000010924680, 1.461580736456455920 ) ) ;
#5476 = CARTESIAN_POINT ( 'NONE',  ( 195.0000000000000000, -7.395377635281828788, -2.255140518769849538E-14 ) ) ;
#5477 = CARTESIAN_POINT ( 'NONE',  ( 208.1451861577818079, 36.43593750108394147, -5.444914386472297529 ) ) ;
#5478 = CARTESIAN_POINT ( 'NONE',  ( 106.5389055433250860, 114.7507929638356785, -48.67499999726882010 ) ) ;
#5479 = AXIS2_PLACEMENT_3D ( 'NONE', #14592, #6197, #14867 ) ;
#5480 = CARTESIAN_POINT ( 'NONE',  ( 9.598844408820459861, 32.56640625000000000, 9.598844408820456309 ) ) ;
#5481 = CARTESIAN_POINT ( 'NONE',  ( 13.14518615778179544, 33.80664062608393294, -1.609821015232357215E-15 ) ) ;
#5482 = ORIENTED_EDGE ( 'NONE', *, *, #20131, .T. ) ;
#5483 = DIRECTION ( 'NONE',  ( -0.000000000000000000, -1.000000000000000000, -0.000000000000000000 ) ) ;
#5484 = CARTESIAN_POINT ( 'NONE',  ( 195.0000000000000000, 37.32890625216786873, 13.57481594606304576 ) ) ;
#5485 = DIRECTION ( 'NONE',  ( -0.000000000000000000, 1.000000000000000000, -0.000000000000000000 ) ) ;
#5486 = CARTESIAN_POINT ( 'NONE',  ( 200.4449143864723055, 34.94765625108394147, -13.14518615778179900 ) ) ;
#5487 = EDGE_CURVE ( 'NONE', #3022, #22301, #17987, .T. ) ;
#5488 = VERTEX_POINT ( 'NONE', #834 ) ;
#5489 = CARTESIAN_POINT ( 'NONE',  ( 107.0000000000000142, 110.0000000000000000, -55.00000000000000711 ) ) ;
#5490 = CARTESIAN_POINT ( 'NONE',  ( 6.161062174842293793, 51.27996893916987631, -14.99999999999999289 ) ) ;
#5491 = CARTESIAN_POINT ( 'NONE',  ( 195.7197605961091824, 53.51499872091921617, 14.99999999999995026 ) ) ;
#5492 =( BOUNDED_CURVE ( )  B_SPLINE_CURVE ( 2, ( #24043, #4238, #19759, #8928, #15182, #13464, #22051, #19482, #2525 ),
 .UNSPECIFIED., .F., .F. ) 
 B_SPLINE_CURVE_WITH_KNOTS ( ( 3, 2, 2, 2, 3 ),
 ( 0.4500000000000003997, 0.4750000000000003664, 0.5000000000000004441, 0.5250000000000004663, 0.5500000000000004885 ),
 .UNSPECIFIED. ) 
 CURVE ( )  GEOMETRIC_REPRESENTATION_ITEM ( )  RATIONAL_B_SPLINE_CURVE ( ( 0.9999999999999987788, 0.9238795325112879597, 1.000000000000000000, 0.9238795325112867385, 1.000000000000000000, 0.9238795325112867385, 1.000000000000000000, 0.9238795325112854062, 1.000000000000001332 ) ) 
 REPRESENTATION_ITEM ( '' )  );
#5493 = CARTESIAN_POINT ( 'NONE',  ( 116.4251840539369454, 37.08085937716786873, -5.622872871577873077 ) ) ;
#5494 = CARTESIAN_POINT ( 'NONE',  ( 104.9999999999999858, 90.00000000000000000, -6.938893903907228378E-15 ) ) ;
#5495 = EDGE_CURVE ( 'NONE', #27220, #23665, #9503, .T. ) ;
#5496 = FACE_OUTER_BOUND ( 'NONE', #10822, .T. ) ;
#5497 = CARTESIAN_POINT ( 'NONE',  ( 208.1451861577817795, 37.13046875108393863, 5.444914386472293977 ) ) ;
#5498 = ORIENTED_EDGE ( 'NONE', *, *, #10126, .T. ) ;
#5499 = VECTOR ( 'NONE', #8282, 1000.000000000000000 ) ;
#5500 = EDGE_CURVE ( 'NONE', #9895, #5976, #10183, .T. ) ;
#5501 = ORIENTED_EDGE ( 'NONE', *, *, #12587, .T. ) ;
#5502 = CARTESIAN_POINT ( 'NONE',  ( 104.4587341249999781, -1.846868145590721655, 13.12500000136559208 ) ) ;
#5503 = FACE_OUTER_BOUND ( 'NONE', #18514, .T. ) ;
#5504 = LINE ( 'NONE', #12577, #12122 ) ;
#5505 = EDGE_CURVE ( 'NONE', #8833, #9543, #18765, .T. ) ;
#5506 = CARTESIAN_POINT ( 'NONE',  ( -0.5932557025505245107, 35.99999999999998579, 13.13889047851773029 ) ) ;
#5507 = CARTESIAN_POINT ( 'NONE',  ( 59.55508561352770158, 32.16953125108393152, 13.14518615778179722 ) ) ;
#5508 = PRESENTATION_STYLE_ASSIGNMENT (( #3085 ) ) ;
#5509 = ADVANCED_FACE ( 'NONE', ( #23049 ), #15019, .T. ) ;
#5510 = CARTESIAN_POINT ( 'NONE',  ( -9.295050272127044266, 39.26367187608393294, 9.295050272127047819 ) ) ;
#5511 = CARTESIAN_POINT ( 'NONE',  ( 2.849501950123402202E-15, 1.000000000000000000, -23.26794919243112503 ) ) ;
#5512 = CARTESIAN_POINT ( 'NONE',  ( 106.9999999999999858, 112.2744378736303474, -53.39999999453764445 ) ) ;
#5513 = CARTESIAN_POINT ( 'NONE',  ( -5.365496568044598291, 54.48174559707608466, 14.99999999999999645 ) ) ;
#5514 = CARTESIAN_POINT ( 'NONE',  ( 135.6228728715778686, 33.60820312499998863, -13.57481594606304753 ) ) ;
#5515 = ADVANCED_FACE ( 'NONE', ( #28115 ), #25827, .T. ) ;
#5516 = VERTEX_POINT ( 'NONE', #23417 ) ;
#5517 = CARTESIAN_POINT ( 'NONE',  ( 2.849501950123402596E-15, 0.000000000000000000, -23.26794919243112858 ) ) ;
#5518 = CARTESIAN_POINT ( 'NONE',  ( 2.414731522848535132E-15, 34.60039062608393579, 13.14518615778179544 ) ) ;
#5519 = CARTESIAN_POINT ( 'NONE',  ( 5.622872871577871301, 35.29492187716788720, -13.57481594606304753 ) ) ;
#5520 = CARTESIAN_POINT ( 'NONE',  ( 102.0710678118654329, -4.999999999999989342, 4.437500002731185944 ) ) ;
#5521 = CARTESIAN_POINT ( 'NONE',  ( 143.1451861577818079, 40.35507812608393863, -1.609821015232357215E-15 ) ) ;
#5522 = CARTESIAN_POINT ( 'NONE',  ( 78.14518615778179367, 40.15664062608393436, -1.609821015232357215E-15 ) ) ;
#5523 = VECTOR ( 'NONE', #20594, 1000.000000000000000 ) ;
#5524 = CARTESIAN_POINT ( 'NONE',  ( 102.0710678118653760, 80.31250000000001421, 5.000000000000054179 ) ) ;
#5525 = CARTESIAN_POINT ( 'NONE',  ( 9.295050272127047819, 40.05742187608392868, 9.295050272127046043 ) ) ;
#5526 = CARTESIAN_POINT ( 'NONE',  ( 13.14518615778179544, 33.21132812608393436, -1.609821015232357215E-15 ) ) ;
#5527 = LINE ( 'NONE', #22913, #26698 ) ;
#5528 = ADVANCED_FACE ( 'NONE', ( #18851 ), #27559, .T. ) ;
#5529 = CARTESIAN_POINT ( 'NONE',  ( 108.0825317499999869, 107.3738262389971680, -50.97499999726881725 ) ) ;
#5530 = VECTOR ( 'NONE', #5854, 1000.000000000000000 ) ;
#5531 = ORIENTED_EDGE ( 'NONE', *, *, #20675, .T. ) ;
#5532 = SURFACE_SIDE_STYLE ('',( #6455 ) ) ;
#5533 = CARTESIAN_POINT ( 'NONE',  ( 9.295050272127046043, 40.25585937608393294, -9.295050272127046043 ) ) ;
#5534 = CARTESIAN_POINT ( 'NONE',  ( 138.1931556449105472, 36.00000000000000000, 10.45682415286355038 ) ) ;
#5535 = FACE_OUTER_BOUND ( 'NONE', #18126, .T. ) ;
#5536 = CARTESIAN_POINT ( 'NONE',  ( 94.33688103937534208, 114.1144967660473242, -50.69999999453764161 ) ) ;
#5537 =( BOUNDED_CURVE ( )  B_SPLINE_CURVE ( 2, ( #26699, #7148, #15842, #24552, #5034 ),
 .UNSPECIFIED., .F., .T. ) 
 B_SPLINE_CURVE_WITH_KNOTS ( ( 3, 2, 3 ),
 ( 0.9500000000000009548, 0.9750000000000005329, 1.000000000000000000 ),
 .UNSPECIFIED. ) 
 CURVE ( )  GEOMETRIC_REPRESENTATION_ITEM ( )  RATIONAL_B_SPLINE_CURVE ( ( 0.9999999999999970024, 0.9238795325112897361, 1.000000000000000000, 0.9238795325112867385, 1.000000000000000000 ) ) 
 REPRESENTATION_ITEM ( '' )  );
#5538 = EDGE_CURVE ( 'NONE', #2926, #21015, #20880, .T. ) ;
#5539 = CARTESIAN_POINT ( 'NONE',  ( 105.6631189606246295, 105.8855032339526758, -47.20000000000000284 ) ) ;
#5540 = CARTESIAN_POINT ( 'NONE',  ( 94.99999999999995737, 1.387778780781445676E-14, 13.00000000000000000 ) ) ;
#5541 = CARTESIAN_POINT ( 'NONE',  ( -13.57481594606304576, 34.64999999999999147, 0.000000000000000000 ) ) ;
#5542 = ORIENTED_EDGE ( 'NONE', *, *, #18415, .F. ) ;
#5543 = CARTESIAN_POINT ( 'NONE',  ( 2.493653234604083739E-15, 33.26093749999999716, 13.57481594606304576 ) ) ;
#5544 = CARTESIAN_POINT ( 'NONE',  ( -13.57481594606304576, 40.25585937499999289, 5.622872871577880183 ) ) ;
#5545 = CARTESIAN_POINT ( 'NONE',  ( -5.444914386472297529, 32.46718750108393436, -13.14518615778179900 ) ) ;
#5546 = CARTESIAN_POINT ( 'NONE',  ( -13.14518615778179722, 35.74140625108393721, -5.444914386472297529 ) ) ;
#5547 = EDGE_CURVE ( 'NONE', #11898, #8127, #6302, .T. ) ;
#5548 = CARTESIAN_POINT ( 'NONE',  ( 13.57481594606304931, 34.30273437716787299, 5.622872871577869525 ) ) ;
#5549 = CARTESIAN_POINT ( 'NONE',  ( 103.5355339059327093, 3.535533905932755072, 2.750000002731185944 ) ) ;
#5550 = CARTESIAN_POINT ( 'NONE',  ( 99.99999999999998579, 125.0000000000000000, -9.540979117872439019E-15 ) ) ;
#5551 = CARTESIAN_POINT ( 'NONE',  ( 70.44491438647230552, 40.50390625108394005, -13.14518615778179900 ) ) ;
#5552 = CARTESIAN_POINT ( 'NONE',  ( 96.46446609406726225, 90.62500000000000000, 3.535533905932723986 ) ) ;
#5553 = CARTESIAN_POINT ( 'NONE',  ( 101.3296865857814311, 123.0000000000000000, 2.137053098915790539 ) ) ;
#5554 = CARTESIAN_POINT ( 'NONE',  ( 130.0000000000000000, 38.12265625216787157, 13.57481594606304576 ) ) ;
#5555 = CARTESIAN_POINT ( 'NONE',  ( 5.622872871577878406, 32.51679687499999716, 13.57481594606304576 ) ) ;
#5556 = CARTESIAN_POINT ( 'NONE',  ( 106.5389055433250860, 105.2492070361643215, -55.07499999726882578 ) ) ;
#5557 = CARTESIAN_POINT ( 'NONE',  ( 124.5550856135277087, 35.84062500108394289, -13.14518615778179900 ) ) ;
#5558 = PRODUCT_DEFINITION_SHAPE ( 'NONE', 'NONE',  #28213 ) ;
#5559 = EDGE_LOOP ( 'NONE', ( #27877, #9683, #2537, #23662 ) ) ;
#5560 = CYLINDRICAL_SURFACE ( 'NONE', #6796, 5.000000000000000888 ) ;
#5561 = CARTESIAN_POINT ( 'NONE',  ( 104.9999999999999858, 90.43749999863440792, -6.938893903907228378E-15 ) ) ;
#5562 = CARTESIAN_POINT ( 'NONE',  ( 99.99999999999995737, 83.68750000136560629, 4.458734124999988779 ) ) ;
#5563 = CARTESIAN_POINT ( 'NONE',  ( 139.2950502721270425, 39.26367187608393294, 9.295050272127046043 ) ) ;
#5564 = CARTESIAN_POINT ( 'NONE',  ( 55.40115559117954547, 39.41250000216787441, -9.598844408820458085 ) ) ;
#5565 = CARTESIAN_POINT ( 'NONE',  ( 99.99999999999997158, 118.4984768113314004, -46.12499999726880873 ) ) ;
#5566 = CARTESIAN_POINT ( 'NONE',  ( 200.4449143864723055, 40.50390625108394005, -13.14518615778179900 ) ) ;
#5567 = CARTESIAN_POINT ( 'NONE',  ( 2.493653234604083739E-15, 39.71015625216787015, 13.57481594606304576 ) ) ;
#5568 = ORIENTED_EDGE ( 'NONE', *, *, #14474, .T. ) ;
#5569 = CARTESIAN_POINT ( 'NONE',  ( 94.99999999999995737, 1.387778780781445676E-14, 9.000000000000000000 ) ) ;
#5570 = VERTEX_POINT ( 'NONE', #12835 ) ;
#5571 = CARTESIAN_POINT ( 'NONE',  ( 13.14518615778179900, 33.95546875108393436, 5.444914386472293977 ) ) ;
#5572 = CARTESIAN_POINT ( 'NONE',  ( 208.5748159460630120, 32.02070312716787015, -5.622872871577873077 ) ) ;
#5573 = CARTESIAN_POINT ( 'NONE',  ( 2.493653234604083739E-15, 35.74140625216787015, 13.57481594606304576 ) ) ;
#5574 = CARTESIAN_POINT ( 'NONE',  ( 104.9999999999999574, 2.071067811865491937, 11.68750000273118772 ) ) ;
#5575 = DIRECTION ( 'NONE',  ( -0.000000000000000000, -0.000000000000000000, 1.000000000000000000 ) ) ;
#5576 = CARTESIAN_POINT ( 'NONE',  ( 3.061616997868383831E-15, 20.00000000000000000, -25.00000000000000711 ) ) ;
#5577 = CARTESIAN_POINT ( 'NONE',  ( 97.92893218813451028, -4.999999999999989342, 11.18750000000000000 ) ) ;
#5578 = CARTESIAN_POINT ( 'NONE',  ( 104.4587341249999923, 91.24999999863439371, 1.846868145590726318 ) ) ;
#5579 = CARTESIAN_POINT ( 'NONE',  ( 100.8561741729129153, 123.7000000010924765, -2.066987299999999195 ) ) ;
#5580 = CARTESIAN_POINT ( 'NONE',  ( 185.7049497278729575, 32.91367187608393152, 9.295050272127047819 ) ) ;
#5581 = CARTESIAN_POINT ( 'NONE',  ( 120.2864525059511180, 35.99999999999999289, 8.898183052316758435 ) ) ;
#5582 = CARTESIAN_POINT ( 'NONE',  ( 99.99999999999995737, 4.458734125000016313, 8.437500001365592084 ) ) ;
#5583 = CARTESIAN_POINT ( 'NONE',  ( -9.598844408820454532, 38.02343750216788010, 9.598844408820459861 ) ) ;
#5584 = CARTESIAN_POINT ( 'NONE',  ( 98.15313185440923860, 4.458734125000016313, 11.25000000136559208 ) ) ;
#5585 = CARTESIAN_POINT ( 'NONE',  ( 95.67376207875072680, 104.0454443415356991, -48.20000000546237828 ) ) ;
#5586 = CARTESIAN_POINT ( 'NONE',  ( 99.99999999999998579, 90.56249999863440792, -4.458734124999994997 ) ) ;
#5587 = DIRECTION ( 'NONE',  ( -1.000000000000000000, -0.000000000000000000, -0.000000000000000000 ) ) ;
#5588 = CARTESIAN_POINT ( 'NONE',  ( 104.9952793366501567, 103.1245878333314465, -54.92499999726882720 ) ) ;
#5589 = CARTESIAN_POINT ( 'NONE',  ( 13.14518615778179900, 32.36796875108393579, 5.444914386472293977 ) ) ;
#5590 = ORIENTED_EDGE ( 'NONE', *, *, #7501, .F. ) ;
#5591 = FILL_AREA_STYLE_COLOUR ( '', #9978 ) ;
#5592 = DIRECTION ( 'NONE',  ( -0.8660254037844407060, 0.4999999999999963363, 0.000000000000000000 ) ) ;
#5593 = AXIS2_PLACEMENT_3D ( 'NONE', #22743, #11878, #16449 ) ;
#5594 = CARTESIAN_POINT ( 'NONE',  ( 185.7049497278729575, 34.10429687608393579, -9.295050272127046043 ) ) ;
#5595 = ORIENTED_EDGE ( 'NONE', *, *, #6007, .F. ) ;
#5596 = CARTESIAN_POINT ( 'NONE',  ( 186.7403884711090143, 50.00000000056305538, -10.79618466885647265 ) ) ;
#5597 = CARTESIAN_POINT ( 'NONE',  ( 99.99999999999995737, -4.458734124999988779, 7.937500001365592084 ) ) ;
#5598 = ORIENTED_EDGE ( 'NONE', *, *, #23880, .T. ) ;
#5599 = CARTESIAN_POINT ( 'NONE',  ( 106.5389055433251002, 105.2492070361643215, -44.57500000273119412 ) ) ;
#5600 = CARTESIAN_POINT ( 'NONE',  ( -13.14518615778179900, 32.56640625108394005, -5.444914386472297529 ) ) ;
#5601 = CARTESIAN_POINT ( 'NONE',  ( 65.00000000000000000, 36.13828125216787157, -13.57481594606304576 ) ) ;
#5602 = CARTESIAN_POINT ( 'NONE',  ( 107.0000000000000000, 112.2744378736303190, -53.90000000000000568 ) ) ;
#5603 = CARTESIAN_POINT ( 'NONE',  ( 5.444914386472302859, 38.61875000108392442, 13.14518615778179189 ) ) ;
#5604 = CARTESIAN_POINT ( 'NONE',  ( 2.414731522848535132E-15, 40.15664062608393436, 13.14518615778179544 ) ) ;
#5605 = CARTESIAN_POINT ( 'NONE',  ( 95.54126587499999346, 93.12499999863439371, 1.846868145590722543 ) ) ;
#5606 = CARTESIAN_POINT ( 'NONE',  ( 84.99999999999998579, 100.0000000000000000, -15.00000000000000533 ) ) ;
#5607 = PRESENTATION_LAYER_ASSIGNMENT (  '', '', ( #17879 ) ) ;
#5608 = CARTESIAN_POINT ( 'NONE',  ( 105.6631189606246295, 105.8855032339526758, -50.20000000000001705 ) ) ;
#5609 = CARTESIAN_POINT ( 'NONE',  ( 9.295050272127046043, 32.51679687608393721, -9.295050272127046043 ) ) ;
#5610 = CARTESIAN_POINT ( 'NONE',  ( 96.84719886470459471, -3.152801135295355994, 4.812500001365592084 ) ) ;
#5611 = CARTESIAN_POINT ( 'NONE',  ( 104.4587341249999781, 83.12500000136560629, 1.846868145590721655 ) ) ;
#5612 = CARTESIAN_POINT ( 'NONE',  ( -5.444914386472299306, 36.73359375108393010, 13.14518615778179722 ) ) ;
#5613 = CARTESIAN_POINT ( 'NONE',  ( 65.00000000000000000, 38.91640625216786731, 13.57481594606304576 ) ) ;
#5614 = CARTESIAN_POINT ( 'NONE',  ( 64.15789240453534603, 53.50112910130382460, 14.99999999999998224 ) ) ;
#5615 = ORIENTED_EDGE ( 'NONE', *, *, #9353, .F. ) ;
#5616 = CARTESIAN_POINT ( 'NONE',  ( -13.14518615778179544, 35.98945312608393721, 0.000000000000000000 ) ) ;
#5617 = CARTESIAN_POINT ( 'NONE',  ( 100.8561741729129153, 124.3000000010924708, -2.066987299999999195 ) ) ;
#5618 = LINE ( 'NONE', #3472, #18498 ) ;
#5619 = CARTESIAN_POINT ( 'NONE',  ( 104.9999999999999716, 1.449011120738813565E-14, 3.625000002731184612 ) ) ;
#5620 = CARTESIAN_POINT ( 'NONE',  ( -8.312177448680279460E-16, 40.00781250000000000, -13.57481594606304576 ) ) ;
#5621 = PRODUCT_RELATED_PRODUCT_CATEGORY ( 'part', '', ( #16047 ) ) ;
#5622 = EDGE_CURVE ( 'NONE', #8262, #16552, #2037, .T. ) ;
#5623 = CARTESIAN_POINT ( 'NONE',  ( 99.99999999999998579, 93.25000000000000000, -4.999999999999997335 ) ) ;
#5624 = CARTESIAN_POINT ( 'NONE',  ( -8.049105076161786076E-16, 31.62382812608393579, -13.14518615778179544 ) ) ;
#5625 = ORIENTED_EDGE ( 'NONE', *, *, #10165, .F. ) ;
#5626 = DIRECTION ( 'NONE',  ( 0.000000000000000000, 0.000000000000000000, -1.000000000000000000 ) ) ;
#5627 = CARTESIAN_POINT ( 'NONE',  ( 59.55508561352770158, 39.31328125108392868, 13.14518615778179722 ) ) ;
#5628 = CARTESIAN_POINT ( 'NONE',  ( 196.1371678245420753, 35.99999999999999289, 13.09590655363592582 ) ) ;
#5629 = AXIS2_PLACEMENT_3D ( 'NONE', #9750, #16014, #939 ) ;
#5630 = CARTESIAN_POINT ( 'NONE',  ( 0.000000000000000000, 40.99999999999999289, -13.57481594606304576 ) ) ;
#5631 = ORIENTED_EDGE ( 'NONE', *, *, #23286, .F. ) ;
#5632 = DIRECTION ( 'NONE',  ( 0.000000000000000000, 4.625929269271485914E-16, 1.000000000000000000 ) ) ;
#5633 = CARTESIAN_POINT ( 'NONE',  ( -0.4460412567800353667, 49.99999999978076204, -13.57776691409236136 ) ) ;
#5634 = FACE_OUTER_BOUND ( 'NONE', #15713, .T. ) ;
#5635 = CARTESIAN_POINT ( 'NONE',  ( 130.0000000000000000, 38.51953125216787299, -13.57481594606304576 ) ) ;
#5636 = CARTESIAN_POINT ( 'NONE',  ( 102.0710678118654329, -4.999999999999989342, 7.312500000000000000 ) ) ;
#5637 = LINE ( 'NONE', #21297, #21902 ) ;
#5638 = CARTESIAN_POINT ( 'NONE',  ( 181.8548138422181921, 37.52734375108393294, -5.444914386472297529 ) ) ;
#5639 = ORIENTED_EDGE ( 'NONE', *, *, #22680, .T. ) ;
#5640 =( LENGTH_UNIT ( ) NAMED_UNIT ( * ) SI_UNIT ( .MILLI., .METRE. ) );
#5641 = CARTESIAN_POINT ( 'NONE',  ( 96.84719886470459471, -3.152801135295355994, 0.5625000013655921949 ) ) ;
#5642 = DIRECTION ( 'NONE',  ( 0.000000000000000000, 0.000000000000000000, -1.000000000000000000 ) ) ;
#5643 = CARTESIAN_POINT ( 'NONE',  ( -13.57481594606304398, 40.25585937499999289, 5.622872871577880183 ) ) ;
#5644 = CARTESIAN_POINT ( 'NONE',  ( 95.67376207875072680, 104.0454443415356991, -52.20000000546237828 ) ) ;
#5645 = CARTESIAN_POINT ( 'NONE',  ( 13.57481594606304576, 34.35234375216787583, -1.662435489736055892E-15 ) ) ;
#5646 = AXIS2_PLACEMENT_3D ( 'NONE', #2789, #9471, #11168 ) ;
#5647 = CARTESIAN_POINT ( 'NONE',  ( 0.000000000000000000, 36.00000000000000000, -11.57481594606304576 ) ) ;
#5648 = CARTESIAN_POINT ( 'NONE',  ( 9.295050272127046043, 40.45429687608393721, -9.295050272127046043 ) ) ;
#5649 = CARTESIAN_POINT ( 'NONE',  ( 99.99999999999995737, 81.25000000000000000, 4.999999999999990230 ) ) ;
#5650 = CARTESIAN_POINT ( 'NONE',  ( 0.000000000000000000, 1.000000000000000000, 0.000000000000000000 ) ) ;
#5651 = CARTESIAN_POINT ( 'NONE',  ( 94.99999999999995737, 83.06250000000001421, 2.071067811865466624 ) ) ;
#5652 = CARTESIAN_POINT ( 'NONE',  ( 116.4251840539369454, 35.39414062499999147, -5.622872871577873077 ) ) ;
#5653 = ORIENTED_EDGE ( 'NONE', *, *, #5170, .F. ) ;
#5654 = CARTESIAN_POINT ( 'NONE',  ( -8.312177448680279460E-16, 32.07031249999999289, -13.57481594606304576 ) ) ;
#5655 = CARTESIAN_POINT ( 'NONE',  ( 13.57481594606304931, 39.75976562499999289, 5.622872871577869525 ) ) ;
#5656 = CARTESIAN_POINT ( 'NONE',  ( -5.622872871577873077, 32.51679687716787726, 13.57481594606304753 ) ) ;
#5657 =( BOUNDED_CURVE ( )  B_SPLINE_CURVE ( 2, ( #17177, #6350, #15024, #21607, #2085, #11312, #7181, #26450, #8909 ),
 .UNSPECIFIED., .F., .F. ) 
 B_SPLINE_CURVE_WITH_KNOTS ( ( 3, 2, 2, 2, 3 ),
 ( 0.2857142857142856984, 0.2946428571428571508, 0.3035714285714284921, 0.3124999999999999445, 0.3214285714285713969 ),
 .UNSPECIFIED. ) 
 CURVE ( )  GEOMETRIC_REPRESENTATION_ITEM ( )  RATIONAL_B_SPLINE_CURVE ( ( 1.000000000000000000, 0.9238795325112867385, 1.000000000000000000, 0.9238795325112867385, 1.000000000000000000, 0.9238795325112867385, 1.000000000000000000, 0.9238795325112871826, 0.9999999999999995559 ) ) 
 REPRESENTATION_ITEM ( '' )  );
#5658 = CARTESIAN_POINT ( 'NONE',  ( 104.9999999999999574, -2.071067811865462627, 6.562500002731185056 ) ) ;
#5659 = CARTESIAN_POINT ( 'NONE',  ( 120.7049497278729575, 39.85898437608393152, -9.295050272127046043 ) ) ;
#5660 = EDGE_CURVE ( 'NONE', #17873, #27982, #19134, .T. ) ;
#5661 = CARTESIAN_POINT ( 'NONE',  ( 70.44491438647230552, 37.92421875108392726, -13.14518615778179900 ) ) ;
#5662 = ADVANCED_FACE ( 'NONE', ( #23142 ), #8579, .F. ) ;
#5663 = CARTESIAN_POINT ( 'NONE',  ( 116.8548138422182205, 40.75195312608393294, 0.000000000000000000 ) ) ;
#5664 = CARTESIAN_POINT ( 'NONE',  ( -9.295050272127044266, 39.06523437608392868, 9.295050272127047819 ) ) ;
#5665 = CARTESIAN_POINT ( 'NONE',  ( 97.50000000000000000, 123.5000000021849615, -9.540979117872439019E-15 ) ) ;
#5666 = CARTESIAN_POINT ( 'NONE',  ( 185.2864525059512459, 36.00000000000002132, 8.898183052316857911 ) ) ;
#5667 = CARTESIAN_POINT ( 'NONE',  ( 97.50236033167490746, 117.6869444889999841, -52.27499999726882862 ) ) ;
#5668 = CARTESIAN_POINT ( 'NONE',  ( -9.598844408820454532, 33.95546874999999432, 9.598844408820459861 ) ) ;
#5669 = CARTESIAN_POINT ( 'NONE',  ( 1.662435489736055892E-15, 40.99999999999999289, 13.57481594606304576 ) ) ;
#5670 = CARTESIAN_POINT ( 'NONE',  ( 135.3649479647156966, 36.00000000000000000, 12.09311862596028142 ) ) ;
#5671 = CARTESIAN_POINT ( 'NONE',  ( 97.50000000000000000, 123.4500000000000028, 1.035533905932725096 ) ) ;
#5672 = EDGE_CURVE ( 'NONE', #1781, #22301, #13879, .T. ) ;
#5673 = CARTESIAN_POINT ( 'NONE',  ( 102.0669872999999939, 124.4000000010924651, -0.8561741729129507261 ) ) ;
#5674 = DIRECTION ( 'NONE',  ( -0.000000000000000000, -0.000000000000000000, 1.000000000000000000 ) ) ;
#5675 = CYLINDRICAL_SURFACE ( 'NONE', #12667, 5.000000000000004441 ) ;
#5676 = CARTESIAN_POINT ( 'NONE',  ( 104.4587341249999639, 1.442382525525748735E-14, 12.93750000136559208 ) ) ;
#5677 = CARTESIAN_POINT ( 'NONE',  ( -9.598844408820454532, 32.36796874999999574, 9.598844408820459861 ) ) ;
#5678 = ORIENTED_EDGE ( 'NONE', *, *, #7373, .T. ) ;
#5679 = CARTESIAN_POINT ( 'NONE',  ( 13.57481594606304576, 40.60312499999999858, -1.662435489736055892E-15 ) ) ;
#5680 = CARTESIAN_POINT ( 'NONE',  ( -13.57481594606304576, 39.46210937499999005, 5.622872871577880183 ) ) ;
#5681 = CARTESIAN_POINT ( 'NONE',  ( 9.295050272127046043, 33.90585937608393152, -9.295050272127046043 ) ) ;
#5682 = CARTESIAN_POINT ( 'NONE',  ( -9.295050272127046043, 31.72304687608393081, -9.295050272127046043 ) ) ;
#5683 = CARTESIAN_POINT ( 'NONE',  ( -13.57481594606304576, 32.41757812716787157, 5.622872871577880183 ) ) ;
#5684 = CARTESIAN_POINT ( 'NONE',  ( 96.46446609406721961, 3.535533905932755072, 2.874999999999999112 ) ) ;
#5685 = CARTESIAN_POINT ( 'NONE',  ( 95.54126587499995082, 80.50000000136560629, 1.846868145590724986 ) ) ;
#5686 = CARTESIAN_POINT ( 'NONE',  ( 70.44491438647230552, 40.20625000108394431, 13.14518615778179189 ) ) ;
#5687 = CARTESIAN_POINT ( 'NONE',  ( 104.9952793366501851, 103.1245878333314323, -46.67500000273118843 ) ) ;
#5688 = CARTESIAN_POINT ( 'NONE',  ( 103.5355339059327235, 94.12500000000000000, -3.535533905932738197 ) ) ;
#5689 = CARTESIAN_POINT ( 'NONE',  ( 100.8561741729129295, 124.2000000010924907, 2.066987299999979211 ) ) ;
#5690 = CARTESIAN_POINT ( 'NONE',  ( 130.0000000000000000, 38.81718749999999574, 13.57481594606304576 ) ) ;
#5691 = CARTESIAN_POINT ( 'NONE',  ( 102.1631189606246295, 103.3426043859339103, -47.89999999453763735 ) ) ;
#5692 = CARTESIAN_POINT ( 'NONE',  ( 139.2950502721270425, 34.89804687608393863, -9.295050272127046043 ) ) ;
#5693 = EDGE_CURVE ( 'NONE', #2287, #24513, #14168, .T. ) ;
#5694 = VERTEX_POINT ( 'NONE', #10841 ) ;
#5695 = CARTESIAN_POINT ( 'NONE',  ( 143.5748159460630688, 37.57695312716787583, -5.622872871577873966 ) ) ;
#5696 = FACE_OUTER_BOUND ( 'NONE', #1107, .T. ) ;
#5697 = CARTESIAN_POINT ( 'NONE',  ( 94.99999999999995737, 79.12500000273118417, -1.387778780781445676E-14 ) ) ;
#5698 = CARTESIAN_POINT ( 'NONE',  ( 139.2950502721270425, 40.05742187608392868, 9.295050272127046043 ) ) ;
#5699 = CARTESIAN_POINT ( 'NONE',  ( 51.42518405393695957, 40.25585937716787299, -5.622872871577873077 ) ) ;
#5700 = VECTOR ( 'NONE', #1940, 1000.000000000000000 ) ;
#5701 = CARTESIAN_POINT ( 'NONE',  ( 91.91746824999998466, 110.0000000000000000, -53.62499999726882294 ) ) ;
#5702 = CARTESIAN_POINT ( 'NONE',  ( -9.598844408820458085, 37.82500000216787583, -9.598844408820458085 ) ) ;
#5703 = ORIENTED_EDGE ( 'NONE', *, *, #26777, .T. ) ;
#5704 = ADVANCED_FACE ( 'NONE', ( #2459 ), #24395, .T. ) ;
#5705 = CARTESIAN_POINT ( 'NONE',  ( 97.92893218813451028, -4.999999999999989342, 11.18749999999999822 ) ) ;
#5706 = VERTEX_POINT ( 'NONE', #15258 ) ;
#5707 =( BOUNDED_CURVE ( )  B_SPLINE_CURVE ( 2, ( #14547, #25396, #9861, #13978, #14267, #5877, #20847, #18701, #5318 ),
 .UNSPECIFIED., .F., .T. ) 
 B_SPLINE_CURVE_WITH_KNOTS ( ( 3, 2, 2, 2, 3 ),
 ( 0.1458333333333336757, 0.1562500000000002776, 0.1666666666666669072, 0.1770833333333335369, 0.1875000000000001388 ),
 .UNSPECIFIED. ) 
 CURVE ( )  GEOMETRIC_REPRESENTATION_ITEM ( )  RATIONAL_B_SPLINE_CURVE ( ( 0.9999999999999975575, 0.9238795325112891810, 1.000000000000000000, 0.9238795325112867385, 1.000000000000000000, 0.9238795325112867385, 1.000000000000000000, 0.9238795325112857393, 1.000000000000001110 ) ) 
 REPRESENTATION_ITEM ( '' )  );
#5708 = CARTESIAN_POINT ( 'NONE',  ( 13.14518615778179900, 32.36796875108393579, 5.444914386472293977 ) ) ;
#5709 = CARTESIAN_POINT ( 'NONE',  ( 195.0000000000000000, 39.16445312608392726, 13.14518615778179544 ) ) ;
#5710 = CARTESIAN_POINT ( 'NONE',  ( 5.622872871577946796, 36.58476562716786873, 13.57481594606297115 ) ) ;
#5711 = CARTESIAN_POINT ( 'NONE',  ( 99.99999999999995737, -4.999999999999990230, 13.37500000273118417 ) ) ;
#5712 = CARTESIAN_POINT ( 'NONE',  ( 135.4449143864723339, 39.21406250108392300, 13.14518615778179189 ) ) ;
#5713 = CARTESIAN_POINT ( 'NONE',  ( -18.00000000000000711, 52.00000000000000711, 2.081668171172169302E-15 ) ) ;
#5714 = PLANE ( 'NONE',  #7218 ) ;
#5715 = CARTESIAN_POINT ( 'NONE',  ( 95.54126587500000767, 93.81249999863440792, -7.484931351350258973E-15 ) ) ;
#5716 = CARTESIAN_POINT ( 'NONE',  ( 99.14382582708707048, 123.0000000010925021, -2.066987299999999195 ) ) ;
#5717 = CARTESIAN_POINT ( 'NONE',  ( 181.4251840539369596, 40.20624999999999005, 0.000000000000000000 ) ) ;
#5718 = PRODUCT_CONTEXT ( 'NONE', #20626, 'mechanical' ) ;
#5719 = CARTESIAN_POINT ( 'NONE',  ( 51.42518405393695957, 39.46210937499999005, 5.622872871577880183 ) ) ;
#5720 = CARTESIAN_POINT ( 'NONE',  ( 98.15313185440925281, -4.458734124999987891, 8.875000001365593860 ) ) ;
#5721 = DIRECTION ( 'NONE',  ( 0.000000000000000000, -1.000000000000000000, 0.000000000000000000 ) ) ;
#5722 = VECTOR ( 'NONE', #12649, 1000.000000000000000 ) ;
#5723 = CARTESIAN_POINT ( 'NONE',  ( 96.84719886470459471, -3.152801135295355994, 5.562500001365591196 ) ) ;
#5724 = CARTESIAN_POINT ( 'NONE',  ( 93.00000000000000000, 110.0000000000000000, -48.50000000546238255 ) ) ;
#5725 = CARTESIAN_POINT ( 'NONE',  ( 103.1528011352953484, 93.68749999863440792, -3.152801135295366208 ) ) ;
#5726 = CARTESIAN_POINT ( 'NONE',  ( -0.5932557025495835967, 36.00000000000000000, 13.13889047851777292 ) ) ;
#5727 = CARTESIAN_POINT ( 'NONE',  ( 5.622872871577871301, 39.95820312499999716, -13.57481594606304753 ) ) ;
#5728 = ORIENTED_EDGE ( 'NONE', *, *, #239, .T. ) ;
#5729 = FACE_OUTER_BOUND ( 'NONE', #20241, .T. ) ;
#5730 = AXIS2_PLACEMENT_3D ( 'NONE', #2444, #26237, #17677 ) ;
#5731 = AXIS2_PLACEMENT_3D ( 'NONE', #15828, #24817, #13821 ) ;
#5732 = CARTESIAN_POINT ( 'NONE',  ( 99.99999999999998579, 91.06249999863440792, 4.458734124999981674 ) ) ;
#5733 = EDGE_LOOP ( 'NONE', ( #3451, #26022, #9175, #10773, #1680, #16736, #4317, #2748, #23807, #5598 ) ) ;
#5734 = VERTEX_POINT ( 'NONE', #605 ) ;
#5735 = CARTESIAN_POINT ( 'NONE',  ( 199.0625835405769237, 50.00000000116060761, -12.98908657125174493 ) ) ;
#5736 = CARTESIAN_POINT ( 'NONE',  ( 98.15313185440925281, -4.458734124999987891, 8.875000001365593860 ) ) ;
#5737 = ORIENTED_EDGE ( 'NONE', *, *, #17160, .F. ) ;
#5738 = CARTESIAN_POINT ( 'NONE',  ( 97.50236033167492167, 117.6869444889999841, -49.77500000273119696 ) ) ;
#5739 = CARTESIAN_POINT ( 'NONE',  ( -9.295050272127046043, 32.51679687608393721, -9.295050272127046043 ) ) ;
#5740 = CARTESIAN_POINT ( 'NONE',  ( 208.5748159460630120, 39.95820312716787726, -5.622872871577873077 ) ) ;
#5741 = CARTESIAN_POINT ( 'NONE',  ( 13.14518615778179722, 38.61875000108392442, -5.444914386472297529 ) ) ;
#5742 = CARTESIAN_POINT ( 'NONE',  ( -8.049105076161786076E-16, 38.17226562608394147, -13.14518615778179544 ) ) ;
#5743 = CARTESIAN_POINT ( 'NONE',  ( 9.295050272127046043, 32.31835937608393294, -9.295050272127046043 ) ) ;
#5744 = CARTESIAN_POINT ( 'NONE',  ( 59.37712712842213136, 39.26367187499999289, -13.57481594606304753 ) ) ;
#5745 = VECTOR ( 'NONE', #16331, 1000.000000000000000 ) ;
#5746 = DIRECTION ( 'NONE',  ( 0.000000000000000000, 1.000000000000000000, 0.000000000000000000 ) ) ;
#5747 = ORIENTED_EDGE ( 'NONE', *, *, #24474, .F. ) ;
#5748 = CARTESIAN_POINT ( 'NONE',  ( 78.57481594606305464, 38.17226562499999432, 5.622872871577868636 ) ) ;
#5749 = CARTESIAN_POINT ( 'NONE',  ( -8.049105076161786076E-16, 33.40976562608393863, -13.14518615778179544 ) ) ;
#5750 = CARTESIAN_POINT ( 'NONE',  ( 99.99999999999995737, -4.458734124999988779, 4.937500001365592972 ) ) ;
#5751 = CARTESIAN_POINT ( 'NONE',  ( 103.1528011352953342, 81.31250000136559208, -3.152801135295383084 ) ) ;
#5752 = CARTESIAN_POINT ( 'NONE',  ( -13.14518615778179900, 34.94765625108392726, -5.444914386472297529 ) ) ;
#5753 = DIRECTION ( 'NONE',  ( 0.000000000000000000, 1.000000000000000000, 0.000000000000000000 ) ) ;
#5754 = CARTESIAN_POINT ( 'NONE',  ( 5.622872871577742515, 38.96601562716787015, 13.57481594606318076 ) ) ;
#5755 = VERTEX_POINT ( 'NONE', #6575 ) ;
#5756 = SURFACE_STYLE_FILL_AREA ( #8433 ) ;
#5757 = CARTESIAN_POINT ( 'NONE',  ( 101.4615807364564546, 124.0500000010924850, 1.461580736456455476 ) ) ;
#5758 = CARTESIAN_POINT ( 'NONE',  ( 96.84719886470463734, 93.93749999863440792, -3.152801135295366208 ) ) ;
#5759 = DIRECTION ( 'NONE',  ( 0.000000000000000000, 0.000000000000000000, 1.000000000000000000 ) ) ;
#5760 = DIRECTION ( 'NONE',  ( 0.000000000000000000, 1.000000000000000000, 0.000000000000000000 ) ) ;
#5761 = CARTESIAN_POINT ( 'NONE',  ( -9.295050272127046043, 31.72304687608393081, -9.295050272127046043 ) ) ;
#5762 = AXIS2_PLACEMENT_3D ( 'NONE', #19461, #28158, #23877 ) ;
#5763 = ORIENTED_EDGE ( 'NONE', *, *, #6347, .F. ) ;
#5764 = CARTESIAN_POINT ( 'NONE',  ( 74.29505027212704249, 38.86679687608393863, -9.295050272127046043 ) ) ;
#5765 = FACE_OUTER_BOUND ( 'NONE', #20936, .T. ) ;
#5766 = CARTESIAN_POINT ( 'NONE',  ( -9.598844408820454532, 39.51171874999999289, 9.598844408820459861 ) ) ;
#5767 = ORIENTED_EDGE ( 'NONE', *, *, #1710, .T. ) ;
#5768 = CARTESIAN_POINT ( 'NONE',  ( 74.59884440882045453, 37.52734375000000000, -9.598844408820458085 ) ) ;
#5769 = DIRECTION ( 'NONE',  ( 5.782411586589357392E-17, -0.000000000000000000, 1.000000000000000000 ) ) ;
#5770 = CARTESIAN_POINT ( 'NONE',  ( 130.0000000000000000, 36.53515625216787299, 13.57481594606304576 ) ) ;
#5771 = CARTESIAN_POINT ( 'NONE',  ( 135.6228728715778971, 33.40976562716787157, 13.57481594606304576 ) ) ;
#5772 = CARTESIAN_POINT ( 'NONE',  ( 97.83688103937537051, 103.3426043859339103, -44.10000000546238397 ) ) ;
#5773 = CARTESIAN_POINT ( 'NONE',  ( 94.99999999999995737, 1.387778780781445676E-14, 34.79898987322334136 ) ) ;
#5774 = CARTESIAN_POINT ( 'NONE',  ( 181.8548138422181921, 38.42031250108393436, 5.444914386472304635 ) ) ;
#5775 = ORIENTED_EDGE ( 'NONE', *, *, #10019, .T. ) ;
#5776 = EDGE_CURVE ( 'NONE', #12136, #19447, #13547, .T. ) ;
#5777 = ORIENTED_EDGE ( 'NONE', *, *, #1705, .F. ) ;
#5778 = CARTESIAN_POINT ( 'NONE',  ( 96.84719886470459471, -3.152801135295355994, 2.562500001365592084 ) ) ;
#5779 = AXIS2_PLACEMENT_3D ( 'NONE', #24021, #13299, #4500 ) ;
#5780 = CARTESIAN_POINT ( 'NONE',  ( 95.54126587499996504, 1.387778780781445676E-14, 13.68750000136559386 ) ) ;
#5781 = CARTESIAN_POINT ( 'NONE',  ( 5.622872871577796694, 39.95820312499999716, -13.57481594606312036 ) ) ;
#5782 = CIRCLE ( 'NONE', #16701, 19.22649730810373470 ) ;
#5783 = CARTESIAN_POINT ( 'NONE',  ( 101.8468681455907046, 83.12500000136560629, -4.458734125000016313 ) ) ;
#5784 = DIRECTION ( 'NONE',  ( 0.000000000000000000, 0.000000000000000000, 1.000000000000000000 ) ) ;
#5785 = CARTESIAN_POINT ( 'NONE',  ( 130.0000000000000000, 40.10703125216787157, -13.57481594606304576 ) ) ;
#5786 = CARTESIAN_POINT ( 'NONE',  ( -5.444914386472299306, 39.31328125108394289, 13.14518615778179722 ) ) ;
#5787 = CARTESIAN_POINT ( 'NONE',  ( 2.493653234604083739E-15, 38.81718749999999574, 13.57481594606304576 ) ) ;
#5788 = CARTESIAN_POINT ( 'NONE',  ( 6.831134457304148810, 36.00000000000000000, 11.35217666746037501 ) ) ;
#5789 = CARTESIAN_POINT ( 'NONE',  ( 130.0000000000000000, 50.00000000000000000, -1.503427012513233026E-14 ) ) ;
#5790 = CARTESIAN_POINT ( 'NONE',  ( 99.99999999999997158, 101.5015231886685854, -49.12499999726882294 ) ) ;
#5791 = VERTEX_POINT ( 'NONE', #6999 ) ;
#5792 = ORIENTED_EDGE ( 'NONE', *, *, #18415, .T. ) ;
#5793 = CARTESIAN_POINT ( 'NONE',  ( -9.598844408820454532, 37.22968750216787726, 9.598844408820459861 ) ) ;
#5794 = UNCERTAINTY_MEASURE_WITH_UNIT (LENGTH_MEASURE( 1.000000000000000082E-05 ), #13814, 'distance_accuracy_value', 'NONE');
#5795 = CARTESIAN_POINT ( 'NONE',  ( 9.598844408820456309, 39.11484374999999858, -9.598844408820458085 ) ) ;
#5796 = CARTESIAN_POINT ( 'NONE',  ( -8.049105076161786076E-16, 40.35507812608393152, -13.14518615778179544 ) ) ;
#5797 = VECTOR ( 'NONE', #20291, 1000.000000000000000 ) ;
#5798 = CARTESIAN_POINT ( 'NONE',  ( 94.99999999999995737, -2.071067811865466624, 6.187500002731184168 ) ) ;
#5799 = CARTESIAN_POINT ( 'NONE',  ( 139.2950502721270425, 39.46210937608393721, 9.295050272127046043 ) ) ;
#5800 = CARTESIAN_POINT ( 'NONE',  ( 51.85481384221819923, 35.74140625108393721, -5.444914386472297529 ) ) ;
#5801 = ORIENTED_EDGE ( 'NONE', *, *, #6518, .T. ) ;
#5802 = CARTESIAN_POINT ( 'NONE',  ( 55.88434273820531928, 36.00000000000001421, 9.510219181138525713 ) ) ;
#5803 = CARTESIAN_POINT ( 'NONE',  ( 13.14518615778179900, 35.34453125108392868, 5.444914386472293977 ) ) ;
#5804 = CARTESIAN_POINT ( 'NONE',  ( 55.40115559117954547, 36.33671874999999574, 9.598844408820459861 ) ) ;
#5805 = CARTESIAN_POINT ( 'NONE',  ( 107.0000000000000142, 110.0000000000000000, -49.00000000000000711 ) ) ;
#5806 = DIRECTION ( 'NONE',  ( -0.000000000000000000, 1.000000000000000000, -0.000000000000000000 ) ) ;
#5807 = CARTESIAN_POINT ( 'NONE',  ( -13.14518615778179900, 38.91640625108393436, -5.444914386472297529 ) ) ;
#5808 = CARTESIAN_POINT ( 'NONE',  ( 142.2511908804447387, 36.00000000000001421, 5.405483146087447288 ) ) ;
#5809 = CARTESIAN_POINT ( 'NONE',  ( 97.50000000000000000, 125.0184775906502068, 0.3826834323650784575 ) ) ;
#5810 = CARTESIAN_POINT ( 'NONE',  ( 101.4615807364564546, 123.6500000010924651, -1.461580736456474794 ) ) ;
#5811 = CARTESIAN_POINT ( 'NONE',  ( 99.99999999999995737, 85.00000000000000000, -1.387778780781445676E-14 ) ) ;
#5812 = CARTESIAN_POINT ( 'NONE',  ( -8.312177448680279460E-16, 38.42031249999999432, -13.57481594606304576 ) ) ;
#5813 = CARTESIAN_POINT ( 'NONE',  ( 95.54126587499995082, 1.846868145590750077, 12.37500000136559208 ) ) ;
#5814 = CARTESIAN_POINT ( 'NONE',  ( 99.99999999999995737, 82.25000000000000000, 4.999999999999990230 ) ) ;
#5815 = VERTEX_POINT ( 'NONE', #2745 ) ;
#5816 = CARTESIAN_POINT ( 'NONE',  ( 102.4999999999999716, 123.9500000021849502, -1.035533905932742638 ) ) ;
#5817 = CARTESIAN_POINT ( 'NONE',  ( -9.598844408820454532, 40.30546874999999574, 9.598844408820459861 ) ) ;
#5818 = CARTESIAN_POINT ( 'NONE',  ( 94.99999999999995737, 2.071067811865491493, 8.937500000000000000 ) ) ;
#5819 = CARTESIAN_POINT ( 'NONE',  ( 5.622872871577878406, 33.40976562716787157, 13.57481594606304576 ) ) ;
#5820 = CARTESIAN_POINT ( 'NONE',  ( 99.99999999999998579, 90.00000000000000000, -6.938893903907228378E-15 ) ) ;
#5821 = CARTESIAN_POINT ( 'NONE',  ( 95.54126587499995082, 79.50000000136560629, 1.846868145590724986 ) ) ;
#5822 = CARTESIAN_POINT ( 'NONE',  ( 55.70494972787295751, 39.26367187608393294, 9.295050272127047819 ) ) ;
#5823 = EDGE_CURVE ( 'NONE', #12988, #12573, #22944, .T. ) ;
#5824 = CARTESIAN_POINT ( 'NONE',  ( 102.4976396683250925, 102.3130555110000159, -48.77500000273119696 ) ) ;
#5825 = CARTESIAN_POINT ( 'NONE',  ( -9.396418828207704684E-17, 52.00000000000000711, -12.99999999999999822 ) ) ;
#5826 =( BOUNDED_CURVE ( )  B_SPLINE_CURVE ( 2, ( #17493, #4533, #8802, #17067, #12912, #10786, #19776, #19636, #14921 ),
 .UNSPECIFIED., .F., .F. ) 
 B_SPLINE_CURVE_WITH_KNOTS ( ( 3, 2, 2, 2, 3 ),
 ( 0.6458333333333333703, 0.6562500000000000000, 0.6666666666666665186, 0.6770833333333332593, 0.6874999999999997780 ),
 .UNSPECIFIED. ) 
 CURVE ( )  GEOMETRIC_REPRESENTATION_ITEM ( )  RATIONAL_B_SPLINE_CURVE ( ( 1.000000000000000000, 0.9238795325112867385, 1.000000000000000000, 0.9238795325112867385, 1.000000000000000000, 0.9238795325112867385, 1.000000000000000000, 0.9238795325112884038, 0.9999999999999983347 ) ) 
 REPRESENTATION_ITEM ( '' )  );
#5827 = CARTESIAN_POINT ( 'NONE',  ( 97.93301270000000613, 122.9500000010924765, -9.540979117872439019E-15 ) ) ;
#5828 = CARTESIAN_POINT ( 'NONE',  ( 13.57481594606304576, 33.45937499999999432, -1.662435489736055892E-15 ) ) ;
#5829 = CARTESIAN_POINT ( 'NONE',  ( 95.67376207875069838, 115.9545556584642867, -50.79999999453764303 ) ) ;
#5830 = CARTESIAN_POINT ( 'NONE',  ( 143.5748159460630404, 40.55351562499998863, 5.622872871577869525 ) ) ;
#5831 = EDGE_LOOP ( 'NONE', ( #3312, #12341, #14432, #5000 ) ) ;
#5832 = CARTESIAN_POINT ( 'NONE',  ( -8.392215291638379426, 54.99999999999999289, -14.99999999999999822 ) ) ;
#5833 = CARTESIAN_POINT ( 'NONE',  ( -5.444914386472297529, 40.60312500108393863, -13.14518615778179900 ) ) ;
#5834 = CARTESIAN_POINT ( 'NONE',  ( 13.57481594606304931, 39.06523437716786873, 5.622872871577869525 ) ) ;
#5835 = CARTESIAN_POINT ( 'NONE',  ( 95.00000000000000000, 94.50000000000000000, -7.551217303480904118E-15 ) ) ;
#5836 = CARTESIAN_POINT ( 'NONE',  ( 74.59884440882045453, 37.62656250216787157, -9.598844408820458085 ) ) ;
#5837 = CARTESIAN_POINT ( 'NONE',  ( 93.46109445667489979, 105.2492070361643215, -53.42499999726882720 ) ) ;
#5838 = CARTESIAN_POINT ( 'NONE',  ( 13.57481594606304931, 38.27148437716787299, 5.622872871577869525 ) ) ;
#5839 = ORIENTED_EDGE ( 'NONE', *, *, #1180, .T. ) ;
#5840 = CARTESIAN_POINT ( 'NONE',  ( 103.5355339059327093, -3.535533905932726206, 9.375000000000000000 ) ) ;
#5841 = EDGE_CURVE ( 'NONE', #8652, #26290, #23836, .T. ) ;
#5842 = CARTESIAN_POINT ( 'NONE',  ( -13.14518615778179900, 34.35234375108393579, -5.444914386472297529 ) ) ;
#5843 = CARTESIAN_POINT ( 'NONE',  ( 200.4449143864723055, 40.30546875108393579, -13.14518615778179900 ) ) ;
#5844 = CARTESIAN_POINT ( 'NONE',  ( 94.99999999999995737, 2.071067811865491493, 14.06250000273118772 ) ) ;
#5845 = CARTESIAN_POINT ( 'NONE',  ( 139.2950502721270425, 37.08085937608393579, -9.295050272127046043 ) ) ;
#5846 = DIRECTION ( 'NONE',  ( -0.000000000000000000, -0.000000000000000000, -1.000000000000000000 ) ) ;
#5847 = CARTESIAN_POINT ( 'NONE',  ( 104.9999999999999716, 1.449011120738813565E-14, 11.62500000273118417 ) ) ;
#5848 = PLANE ( 'NONE',  #17407 ) ;
#5849 = CARTESIAN_POINT ( 'NONE',  ( 102.4976396683250925, 117.6869444889999841, -49.97500000273119269 ) ) ;
#5850 = CARTESIAN_POINT ( 'NONE',  ( 99.99999999999998579, 123.3500000010924680, 2.066987299999980099 ) ) ;
#5851 = ADVANCED_FACE ( 'NONE', ( #13108 ), #26110, .T. ) ;
#5852 = CARTESIAN_POINT ( 'NONE',  ( 181.4251840539369596, 36.98164062499999005, -5.622872871577873077 ) ) ;
#5853 = SHAPE_DEFINITION_REPRESENTATION ( #831, #10045 ) ;
#5854 = DIRECTION ( 'NONE',  ( -0.000000000000000000, -1.000000000000000000, -0.000000000000000000 ) ) ;
#5855 = CARTESIAN_POINT ( 'NONE',  ( 104.4587341249999781, -1.846868145590721655, 2.125000001365591640 ) ) ;
#5856 = CARTESIAN_POINT ( 'NONE',  ( 78.14518615778179367, 38.56914062608393579, -1.609821015232357215E-15 ) ) ;
#5857 = CARTESIAN_POINT ( 'NONE',  ( 104.4587341249999781, -1.846868145590721655, 4.875000001365592084 ) ) ;
#5858 = CARTESIAN_POINT ( 'NONE',  ( 93.00000000000001421, 107.7255621263696668, -50.40000000546238823 ) ) ;
#5859 = CARTESIAN_POINT ( 'NONE',  ( 95.54126587499999346, 90.74999999863439371, -1.846868145590737864 ) ) ;
#5860 = CARTESIAN_POINT ( 'NONE',  ( 99.99999999999995737, 78.00000000000000000, -3.000000000000018208 ) ) ;
#5861 = CARTESIAN_POINT ( 'NONE',  ( 65.00000000000000000, 36.00000000000000000, -7.517135062566165128E-15 ) ) ;
#5862 = CARTESIAN_POINT ( 'NONE',  ( -13.57481594606304576, 39.41249999999999432, 0.000000000000000000 ) ) ;
#5863 = EDGE_CURVE ( 'NONE', #21579, #9459, #19692, .T. ) ;
#5864 = VECTOR ( 'NONE', #4979, 999.9999999999998863 ) ;
#5865 = ORIENTED_EDGE ( 'NONE', *, *, #27798, .T. ) ;
#5866 = DIRECTION ( 'NONE',  ( -1.000000000000000000, -1.387778780781407810E-15, 7.228014483236696740E-18 ) ) ;
#5867 = DIRECTION ( 'NONE',  ( 0.000000000000000000, 0.000000000000000000, 1.000000000000000000 ) ) ;
#5868 = ORIENTED_EDGE ( 'NONE', *, *, #16537, .T. ) ;
#5869 = EDGE_CURVE ( 'NONE', #23013, #11839, #17552, .T. ) ;
#5870 =( BOUNDED_CURVE ( )  B_SPLINE_CURVE ( 2, ( #25343, #12766, #7819, #14357, #5828, #10076, #10633, #6923, #9070 ),
 .UNSPECIFIED., .F., .F. ) 
 B_SPLINE_CURVE_WITH_KNOTS ( ( 3, 2, 2, 2, 3 ),
 ( 0.7708333333333333703, 0.7812500000000000000, 0.7916666666666665186, 0.8020833333333332593, 0.8124999999999998890 ),
 .UNSPECIFIED. ) 
 CURVE ( )  GEOMETRIC_REPRESENTATION_ITEM ( )  RATIONAL_B_SPLINE_CURVE ( ( 1.000000000000000000, 0.9238795325112867385, 1.000000000000000000, 0.9238795325112867385, 1.000000000000000000, 0.9238795325112867385, 1.000000000000000000, 0.9238795325112875156, 0.9999999999999992228 ) ) 
 REPRESENTATION_ITEM ( '' )  );
#5871 = ORIENTED_EDGE ( 'NONE', *, *, #25176, .T. ) ;
#5872 = CARTESIAN_POINT ( 'NONE',  ( 196.0141308260785706, 51.45790058219387220, -14.99999999999864642 ) ) ;
#5873 = CARTESIAN_POINT ( 'NONE',  ( 104.4587341249999781, -1.846868145590721655, 8.125000001365592084 ) ) ;
#5874 = ORIENTED_EDGE ( 'NONE', *, *, #6004, .F. ) ;
#5875 = CARTESIAN_POINT ( 'NONE',  ( 95.00472066334982912, 116.8754121666685393, -47.67500000273120264 ) ) ;
#5876 = CARTESIAN_POINT ( 'NONE',  ( -5.444914386472297529, 34.84843750108393579, -13.14518615778179900 ) ) ;
#5877 = CARTESIAN_POINT ( 'NONE',  ( 181.4251840539369596, 38.66835937716787441, -5.622872871577872189 ) ) ;
#5878 = CARTESIAN_POINT ( 'NONE',  ( -8.049105076161786076E-16, 39.56132812608393579, -13.14518615778179544 ) ) ;
#5879 = CARTESIAN_POINT ( 'NONE',  ( 102.4976396683250925, 102.3130555110000159, -50.52500000273119696 ) ) ;
#5880 = AXIS2_PLACEMENT_3D ( 'NONE', #11450, #7178, #7467 ) ;
#5881 = CARTESIAN_POINT ( 'NONE',  ( 116.8548138422182205, 38.32109375108394289, -5.444914386472297529 ) ) ;
#5882 = CARTESIAN_POINT ( 'NONE',  ( -13.14518615778179544, 32.61601562608393579, 0.000000000000000000 ) ) ;
#5883 = EDGE_LOOP ( 'NONE', ( #12035, #24685 ) ) ;
#5884 = VECTOR ( 'NONE', #22028, 1000.000000000000000 ) ;
#5885 = CARTESIAN_POINT ( 'NONE',  ( 70.62287287157788285, 37.27929687499999289, 13.57481594606304576 ) ) ;
#5886 = CARTESIAN_POINT ( 'NONE',  ( 99.99999999999998579, 123.2000000000000028, -2.499999999999997780 ) ) ;
#5887 = DIRECTION ( 'NONE',  ( 0.000000000000000000, 0.000000000000000000, -1.000000000000000000 ) ) ;
#5888 = CARTESIAN_POINT ( 'NONE',  ( 96.84719886470459471, 3.152801135295383084, 4.312500001365592084 ) ) ;
#5889 = DIRECTION ( 'NONE',  ( -1.000000000000000000, 0.000000000000000000, 0.000000000000000000 ) ) ;
#5890 = CARTESIAN_POINT ( 'NONE',  ( 104.4587341249999781, -1.846868145590721655, 1.125000001365592750 ) ) ;
#5891 = CARTESIAN_POINT ( 'NONE',  ( 98.15313185440923860, 82.50000000136560629, -4.458734125000016313 ) ) ;
#5892 = CARTESIAN_POINT ( 'NONE',  ( 5.444914386472302859, 33.65781250108393152, 13.14518615778179189 ) ) ;
#5893 = CARTESIAN_POINT ( 'NONE',  ( 13.14518615778179900, 39.61093750108393863, -5.444914386472297529 ) ) ;
#5894 = EDGE_CURVE ( 'NONE', #7171, #16160, #14850, .T. ) ;
#5895 = CARTESIAN_POINT ( 'NONE',  ( 13.57481594606304576, 39.11484375216787157, -1.662435489736055892E-15 ) ) ;
#5896 = EDGE_LOOP ( 'NONE', ( #5064, #25393, #10460, #20794 ) ) ;
#5897 = SURFACE_SIDE_STYLE ('',( #5756 ) ) ;
#5898 = CARTESIAN_POINT ( 'NONE',  ( 0.000000000000000000, 50.00000000000000000, 0.000000000000000000 ) ) ;
#5899 = CARTESIAN_POINT ( 'NONE',  ( 95.54126587500000767, 93.06249999863440792, -7.484931351350258973E-15 ) ) ;
#5900 = DIRECTION ( 'NONE',  ( 1.000000000000000000, 0.000000000000000000, 0.000000000000000000 ) ) ;
#5901 = CARTESIAN_POINT ( 'NONE',  ( 102.2498298612819525, 123.0000000000000284, -0.9005770716734564640 ) ) ;
#5902 = LINE ( 'NONE', #16580, #13937 ) ;
#5903 = PRESENTATION_LAYER_ASSIGNMENT (  '', '', ( #18176 ) ) ;
#5904 =( BOUNDED_CURVE ( )  B_SPLINE_CURVE ( 2, ( #26235, #11246, #6693, #7118, #19964 ),
 .UNSPECIFIED., .F., .F. ) 
 B_SPLINE_CURVE_WITH_KNOTS ( ( 3, 2, 3 ),
 ( 0.000000000000000000, 0.01041666666666679446, 0.02083333333333358892 ),
 .UNSPECIFIED. ) 
 CURVE ( )  GEOMETRIC_REPRESENTATION_ITEM ( )  RATIONAL_B_SPLINE_CURVE ( ( 1.000000000000000000, 0.9238795325112867385, 1.000000000000000000, 0.9238795325112848511, 1.000000000000001776 ) ) 
 REPRESENTATION_ITEM ( '' )  );
#5905 = ORIENTED_EDGE ( 'NONE', *, *, #9151, .T. ) ;
#5906 = CARTESIAN_POINT ( 'NONE',  ( 70.44491438647229131, 38.12265625108393863, -13.14518615778179722 ) ) ;
#5907 = CIRCLE ( 'NONE', #17257, 4.999999999999999112 ) ;
#5908 = CARTESIAN_POINT ( 'NONE',  ( 99.99999999999998579, 90.00000000000000000, -6.938893903907228378E-15 ) ) ;
#5909 = CARTESIAN_POINT ( 'NONE',  ( 5.622872871577878406, 34.89804687499999147, 13.57481594606304398 ) ) ;
#5910 = ORIENTED_EDGE ( 'NONE', *, *, #3900, .T. ) ;
#5911 = PLANE ( 'NONE',  #3411 ) ;
#5912 = CARTESIAN_POINT ( 'NONE',  ( -2.529583995168191990, 49.99999999938367523, -13.34625891065979353 ) ) ;
#5913 = CARTESIAN_POINT ( 'NONE',  ( 130.0000000000000000, 36.93203125216787441, -13.57481594606304576 ) ) ;
#5914 = CARTESIAN_POINT ( 'NONE',  ( 116.4251840539369596, 33.21132812716787441, 5.622872871577880183 ) ) ;
#5915 = CARTESIAN_POINT ( 'NONE',  ( 95.67376207875072680, 104.0454443415356991, -44.20000000546236407 ) ) ;
#5916 = CARTESIAN_POINT ( 'NONE',  ( 95.67376207875072680, 115.9545556584642867, -46.79999999453764303 ) ) ;
#5917 = CARTESIAN_POINT ( 'NONE',  ( 185.7049497278729575, 39.06523437608392868, -9.295050272127046043 ) ) ;
#5918 = ORIENTED_EDGE ( 'NONE', *, *, #12134, .F. ) ;
#5919 = ORIENTED_EDGE ( 'NONE', *, *, #20742, .T. ) ;
#5920 = CARTESIAN_POINT ( 'NONE',  ( 104.4587341249999639, 1.442382525525748735E-14, 13.18750000136559208 ) ) ;
#5921 = CARTESIAN_POINT ( 'NONE',  ( 13.57481594606304931, 39.75976562499999289, 5.622872871577868636 ) ) ;
#5922 = CARTESIAN_POINT ( 'NONE',  ( 99.99999999999995737, 5.000000000000018652, 13.75000000000000000 ) ) ;
#5923 = CARTESIAN_POINT ( 'NONE',  ( 9.598844408820456309, 34.45156250216787441, -9.598844408820458085 ) ) ;
#5924 = CARTESIAN_POINT ( 'NONE',  ( 143.5748159460630688, 39.85898437716787157, 5.622872871577868636 ) ) ;
#5925 = FACE_OUTER_BOUND ( 'NONE', #4204, .T. ) ;
#5926 = CARTESIAN_POINT ( 'NONE',  ( 13.24545034676870969, 36.00000000000000000, 2.307131236161232835 ) ) ;
#5927 = DIRECTION ( 'NONE',  ( 0.000000000000000000, -1.000000000000000000, 0.000000000000000000 ) ) ;
#5928 = CARTESIAN_POINT ( 'NONE',  ( 91.91746824999997045, 107.3738262389971538, -49.52499999726881441 ) ) ;
#5929 = ORIENTED_EDGE ( 'NONE', *, *, #27798, .F. ) ;
#5930 = CARTESIAN_POINT ( 'NONE',  ( -9.598844408820458085, 40.10703124999999147, -9.598844408820458085 ) ) ;
#5931 = CARTESIAN_POINT ( 'NONE',  ( -9.598844408820454532, 32.46718750216787441, 9.598844408820459861 ) ) ;
#5932 = CARTESIAN_POINT ( 'NONE',  ( 94.99999999999995737, -2.071067811865466624, 5.187500002731184168 ) ) ;
#5933 = CARTESIAN_POINT ( 'NONE',  ( 143.1451861577818079, 37.97382812608393721, -1.609821015232357215E-15 ) ) ;
#5934 = CARTESIAN_POINT ( 'NONE',  ( 59.55508561352770158, 35.64218750108392442, -13.14518615778179900 ) ) ;
#5935 = EDGE_CURVE ( 'NONE', #27080, #8561, #17072, .T. ) ;
#5936 = CARTESIAN_POINT ( 'NONE',  ( 99.99999999999995737, 80.25000000000000000, 4.999999999999990230 ) ) ;
#5937 = CARTESIAN_POINT ( 'NONE',  ( 2.414731522848535132E-15, 34.40195312608393152, 13.14518615778179544 ) ) ;
#5938 = CARTESIAN_POINT ( 'NONE',  ( 181.8508260188482097, 35.99999999999998579, -1.058935892997001194 ) ) ;
#5939 = CARTESIAN_POINT ( 'NONE',  ( 95.67376207875072680, 115.9545556584642867, -48.30000000000001137 ) ) ;
#5940 = DIRECTION ( 'NONE',  ( 0.000000000000000000, 0.000000000000000000, -1.000000000000000000 ) ) ;
#5941 = LINE ( 'NONE', #11133, #24366 ) ;
#5942 = CARTESIAN_POINT ( 'NONE',  ( -13.14518615778179544, 38.96601562608393721, 0.000000000000000000 ) ) ;
#5943 = CARTESIAN_POINT ( 'NONE',  ( 143.0198548647682344, 35.99999999999997868, 3.369129432478993103 ) ) ;
#5944 = CARTESIAN_POINT ( 'NONE',  ( 101.0355339059327378, 123.6500000000000199, 2.499999999999977796 ) ) ;
#5945 = CYLINDRICAL_SURFACE ( 'NONE', #20067, 13.57481594606304398 ) ;
#5946 = CARTESIAN_POINT ( 'NONE',  ( 0.000000000000000000, 40.99999999999999289, -15.57481594606304576 ) ) ;
#5947 = PRESENTATION_LAYER_ASSIGNMENT (  '', '', ( #25076 ) ) ;
#5948 = CARTESIAN_POINT ( 'NONE',  ( 99.99999999999995737, 1.387778780781445676E-14, 34.79898987322334136 ) ) ;
#5949 = CARTESIAN_POINT ( 'NONE',  ( 98.15313185440925281, -4.458734124999987891, 11.62500000136559031 ) ) ;
#5950 = DIRECTION ( 'NONE',  ( -0.000000000000000000, -1.000000000000000000, -0.000000000000000000 ) ) ;
#5951 = VERTEX_POINT ( 'NONE', #10376 ) ;
#5952 = CARTESIAN_POINT ( 'NONE',  ( 98.96446609406727646, 123.6500000021849530, 2.499999999999977796 ) ) ;
#5953 = CARTESIAN_POINT ( 'NONE',  ( 9.598844408820459861, 38.91640624999999432, 9.598844408820456309 ) ) ;
#5954 = DIRECTION ( 'NONE',  ( -0.000000000000000000, 1.000000000000000000, -0.000000000000000000 ) ) ;
#5955 = CARTESIAN_POINT ( 'NONE',  ( 13.57481594606304753, 32.02070312716787015, -5.622872871577873077 ) ) ;
#5956 = CARTESIAN_POINT ( 'NONE',  ( 104.4587341249999781, 80.00000000136559208, -1.846868145590750299 ) ) ;
#5957 = CARTESIAN_POINT ( 'NONE',  ( 59.55508561352770158, 39.31328125108394289, 13.14518615778179722 ) ) ;
#5958 = CARTESIAN_POINT ( 'NONE',  ( 108.0825317500000153, 110.0000000000000000, -46.37500000273119838 ) ) ;
#5959 = DIRECTION ( 'NONE',  ( 0.000000000000000000, 0.000000000000000000, 1.000000000000000000 ) ) ;
#5960 = CARTESIAN_POINT ( 'NONE',  ( 99.99999999999998579, 122.9500000010924765, -2.066987299999998751 ) ) ;
#5961 = CARTESIAN_POINT ( 'NONE',  ( 55.40115559117954547, 38.61875000216787157, -9.598844408820458085 ) ) ;
#5962 = CARTESIAN_POINT ( 'NONE',  ( 97.83688103937537051, 103.3426043859339103, -52.09999999453764019 ) ) ;
#5963 = CARTESIAN_POINT ( 'NONE',  ( 130.0000000000000000, 40.40468749999999432, 13.57481594606304576 ) ) ;
#5964 = ORIENTED_EDGE ( 'NONE', *, *, #11204, .F. ) ;
#5965 = CARTESIAN_POINT ( 'NONE',  ( 6.116560239716792857, 54.66944451632674173, -15.00000000000000000 ) ) ;
#5966 = CARTESIAN_POINT ( 'NONE',  ( 5.444914386472297529, 38.91640625108393436, -13.14518615778179900 ) ) ;
#5967 = CARTESIAN_POINT ( 'NONE',  ( 13.57481594606304753, 39.95820312716787726, -5.622872871577873077 ) ) ;
#5968 = CARTESIAN_POINT ( 'NONE',  ( 104.9999999999999716, 94.93750000000000000, 2.071067811865467956 ) ) ;
#5969 = CARTESIAN_POINT ( 'NONE',  ( 59.37712712842213136, 37.77539062716788010, -13.57481594606304753 ) ) ;
#5970 = EDGE_CURVE ( 'NONE', #10403, #152, #19083, .T. ) ;
#5971 = AXIS2_PLACEMENT_3D ( 'NONE', #10755, #15025, #23745 ) ;
#5972 = CARTESIAN_POINT ( 'NONE',  ( 95.00472066334982912, 116.8754121666685393, -53.92499999726881299 ) ) ;
#5973 = CARTESIAN_POINT ( 'NONE',  ( 9.598844408820456309, 34.45156250216787441, -9.598844408820458085 ) ) ;
#5974 = ORIENTED_EDGE ( 'NONE', *, *, #15277, .F. ) ;
#5975 = CARTESIAN_POINT ( 'NONE',  ( 104.9999999999999574, 2.071067811865491937, 8.562500000000000000 ) ) ;
#5976 = VERTEX_POINT ( 'NONE', #1986 ) ;
#5977 = CARTESIAN_POINT ( 'NONE',  ( 65.00000000000000000, 36.00000000000000000, -7.517135062566165128E-15 ) ) ;
#5978 = CARTESIAN_POINT ( 'NONE',  ( 189.5550856135277229, 38.02343750108394005, -13.14518615778179900 ) ) ;
#5979 = CARTESIAN_POINT ( 'NONE',  ( 97.92893218813451028, 5.000000000000018652, 13.93750000273118772 ) ) ;
#5980 = CARTESIAN_POINT ( 'NONE',  ( 139.2950502721270425, 39.26367187608393294, 9.295050272127046043 ) ) ;
#5981 = CARTESIAN_POINT ( 'NONE',  ( 4.157286354961724939, 36.00000000000000000, -12.92256159328856135 ) ) ;
#5982 = CARTESIAN_POINT ( 'NONE',  ( 51.63999894807758295, 40.87597656304196647, 0.000000000000000000 ) ) ;
#5983 = CARTESIAN_POINT ( 'NONE',  ( 0.000000000000000000, 36.00000000000000000, 0.000000000000000000 ) ) ;
#5984 = DIRECTION ( 'NONE',  ( 0.000000000000000000, 0.000000000000000000, -1.000000000000000000 ) ) ;
#5985 =( BOUNDED_SURFACE ( )  B_SPLINE_SURFACE ( 1, 2, ( 
 ( #23630, #19345, #18793, #5833, #23079, #16789, #16654, #1698, #28048, #25349, #12211, #14501, #8515, #19207, #27635, #23218, #3694, #25488, #20940, #12357, #21075, #3826, #1564, #14635, #27772, #10500, #4106, #10355, #8371, #17055, #23353, #12772, #25759, #18927, #21489, #8095, #23490, #5966, #12487, #1970, #8230, #16921, #25621, #6103, #14770, #10638, #17199, #19763, #2108, #9076, #2396, #13469, #8653, #394, #108, #6646, #26329, #15474, #17910, #24189, #28185, #13330, #21776, #22056, #2255, #26621, #19626, #8790, #10917, #6931, #22195, #2674, #21632, #15048, #19911, #15332, #10775, #23766, #11054, #15624, #11335, #23904, #13182, #24048, #8933, #4384, #4242, #12902, #6789, #26475, #19487, #17771, #4668, #24326, #4523, #2530, #17344, #26040, #6511, #535, #9217, #21921, #247, #17622, #4810, #11192, #20056, #15186, #13041, #17481, #26180, #22624, #3366, #3232, #26761, #11900, #5093, #4955, #13899, #11762, #16042, #18622, #16190, #11615, #5518, #2945, #16336, #20761, #26905, #9355, #15898, #27192, #5377, #7203, #9636, #5233, #7351, #680, #20486, #22767, #27046, #18048, #24896, #7068, #967, #22339, #1109, #3095, #14185, #24615, #20624, #20340, #24752, #18341, #7494, #9908, #14046, #20195, #9776, #13755, #18484, #22480, #15763, #827, #9494, #18194, #7643, #22903, #12037, #13616, #24470, #25036, #1245, #2809, #11478, #14598, #27870, #6203, #7918, #25450, #18884, #21174, #16614 ),
 ( #27734, #1796, #8054, #19021, #12173, #20903, #25167, #12732, #21456, #27593, #23316, #16749, #12588, #14732, #21312, #19169, #10461, #1385, #5930, #3789, #23588, #23452, #18757, #3930, #25307, #5655, #12447, #1654, #10313, #10603, #8194, #3654, #25720, #23180, #8333, #1934, #16884, #10046, #5795, #17017, #25583, #27460, #6066, #14873, #4070, #14461, #27326, #7785, #16472, #12317, #14320, #21038, #23041, #1522, #3512, #10174, #10739, #72, #25865, #10880, #24011, #17586, #19870, #6609, #24152, #4629, #19589, #11154, #13287, #28148, #26291, #15010, #19726, #2637, #8615, #355, #15149, #13146, #4205, #4345, #2216, #22159, #11013, #2069, #211, #19449, #23731, #13001, #19310, #28010, #17303, #8753, #6336, #17445, #4489, #6753, #9042, #15294, #22016, #2493, #26144, #17734, #26436, #26003, #15437, #12864, #8896, #8475, #6474, #6895, #23867, #21883, #21594, #21740, #2358, #17164, #15582, #24290, #4771, #13431, #26871, #9741, #4918, #24859, #24576, #2911, #22588, #11723, #14150, #20449, #24430, #9602, #18013, #18303, #26724, #22869, #15866, #5058, #7169, #3196, #18450, #27156, #17874, #11299, #16153, #11581, #26580, #20020, #7317, #11867, #7609, #20161, #9457, #20301, #5198, #643, #500, #9181, #3057, #22729, #7029, #14006, #931, #20589, #787, #27011, #13579, #22302, #15726, #25000, #5480, #18159, #16006, #24720, #5340, #7458, #1072, #16299, #2777, #11441, #13863, #9316, #13722 ) ),
 .UNSPECIFIED., .F., .F., .F. ) 
 B_SPLINE_SURFACE_WITH_KNOTS ( ( 2, 2 ),
 ( 3, 2, 2, 2, 2, 2, 2, 2, 2, 2, 2, 2, 2, 2, 2, 2, 2, 2, 2, 2, 2, 2, 2, 2, 2, 2, 2, 2, 2, 2, 2, 2, 2, 2, 2, 2, 2, 2, 2, 2, 2, 2, 2, 2, 2, 2, 2, 2, 2, 2, 2, 2, 2, 2, 2, 2, 2, 2, 2, 2, 2, 2, 2, 2, 2, 2, 2, 2, 2, 2, 2, 2, 2, 2, 2, 2, 2, 2, 2, 2, 2, 2, 2, 2, 2, 2, 2, 2, 2, 2, 2, 3 ),
 ( 0.000000000000000000, 1.000000000000000000 ),
 ( 0.000000000000000000, 0.01041666666666666609, 0.02083333333333333218, 0.03125000000000000000, 0.04166666666666666435, 0.05208333333333333565, 0.06250000000000000000, 0.07291666666666667129, 0.08333333333333332871, 0.09375000000000000000, 0.1041666666666666713, 0.1145833333333333287, 0.1250000000000000000, 0.1354166666666666574, 0.1458333333333333426, 0.1562500000000000000, 0.1666666666666666574, 0.1770833333333333426, 0.1875000000000000000, 0.1979166666666666574, 0.2083333333333333426, 0.2187500000000000000, 0.2291666666666666574, 0.2395833333333333426, 0.2500000000000000000, 0.2604166666666666852, 0.2708333333333333148, 0.2812500000000000000, 0.2916666666666666852, 0.3020833333333333148, 0.3125000000000000000, 0.3229166666666666852, 0.3333333333333333148, 0.3437500000000000000, 0.3541666666666666852, 0.3645833333333333148, 0.3750000000000000000, 0.3854166666666666852, 0.3958333333333333148, 0.4062500000000000000, 0.4166666666666666852, 0.4270833333333333148, 0.4375000000000000000, 0.4479166666666666852, 0.4583333333333333148, 0.4687500000000000000, 0.4791666666666666852, 0.4895833333333333148, 0.5000000000000000000, 0.5104166666666666297, 0.5208333333333333703, 0.5312500000000000000, 0.5416666666666666297, 0.5520833333333333703, 0.5625000000000000000, 0.5729166666666666297, 0.5833333333333333703, 0.5937500000000000000, 0.6041666666666666297, 0.6145833333333333703, 0.6250000000000000000, 0.6354166666666666297, 0.6458333333333333703, 0.6562500000000000000, 0.6666666666666666297, 0.6770833333333333703, 0.6875000000000000000, 0.6979166666666666297, 0.7083333333333333703, 0.7187500000000000000, 0.7291666666666666297, 0.7395833333333333703, 0.7500000000000000000, 0.7604166666666666297, 0.7708333333333333703, 0.7812500000000000000, 0.7916666666666666297, 0.8020833333333333703, 0.8125000000000000000, 0.8229166666666666297, 0.8333333333333333703, 0.8437500000000000000, 0.8541666666666666297, 0.8645833333333333703, 0.8750000000000000000, 0.8854166666666666297, 0.8958333333333333703, 0.9062500000000000000, 0.9166666666666666297, 0.9270833333333333703, 0.9375000000000000000, 0.9448586968893691873 ),
 .UNSPECIFIED. ) 
 GEOMETRIC_REPRESENTATION_ITEM ( )  RATIONAL_B_SPLINE_SURFACE ( (
 ( 1.000000000000000000, 0.9238795325112867385, 1.000000000000000000, 0.9238795325112867385, 1.000000000000000000, 0.9238795325112867385, 1.000000000000000000, 0.9238795325112867385, 1.000000000000000000, 0.9238795325112867385, 1.000000000000000000, 0.9238795325112867385, 1.000000000000000000, 0.9238795325112867385, 1.000000000000000000, 0.9238795325112867385, 1.000000000000000000, 0.9238795325112867385, 1.000000000000000000, 0.9238795325112867385, 1.000000000000000000, 0.9238795325112867385, 1.000000000000000000, 0.9238795325112867385, 1.000000000000000000, 0.9238795325112867385, 1.000000000000000000, 0.9238795325112867385, 1.000000000000000000, 0.9238795325112867385, 1.000000000000000000, 0.9238795325112867385, 1.000000000000000000, 0.9238795325112867385, 1.000000000000000000, 0.9238795325112867385, 1.000000000000000000, 0.9238795325112867385, 1.000000000000000000, 0.9238795325112867385, 1.000000000000000000, 0.9238795325112867385, 1.000000000000000000, 0.9238795325112867385, 1.000000000000000000, 0.9238795325112867385, 1.000000000000000000, 0.9238795325112867385, 1.000000000000000000, 0.9238795325112867385, 1.000000000000000000, 0.9238795325112867385, 1.000000000000000000, 0.9238795325112867385, 1.000000000000000000, 0.9238795325112867385, 1.000000000000000000, 0.9238795325112867385, 1.000000000000000000, 0.9238795325112867385, 1.000000000000000000, 0.9238795325112867385, 1.000000000000000000, 0.9238795325112867385, 1.000000000000000000, 0.9238795325112867385, 1.000000000000000000, 0.9238795325112867385, 1.000000000000000000, 0.9238795325112867385, 1.000000000000000000, 0.9238795325112867385, 1.000000000000000000, 0.9238795325112867385, 1.000000000000000000, 0.9238795325112867385, 1.000000000000000000, 0.9238795325112867385, 1.000000000000000000, 0.9238795325112867385, 1.000000000000000000, 0.9238795325112867385, 1.000000000000000000, 0.9238795325112867385, 1.000000000000000000, 0.9238795325112867385, 1.000000000000000000, 0.9238795325112867385, 1.000000000000000000, 0.9238795325112867385, 1.000000000000000000, 0.9238795325112867385, 1.000000000000000000, 0.9238795325112867385, 1.000000000000000000, 0.9238795325112867385, 1.000000000000000000, 0.9238795325112867385, 1.000000000000000000, 0.9238795325112867385, 1.000000000000000000, 0.9238795325112867385, 1.000000000000000000, 0.9238795325112867385, 1.000000000000000000, 0.9238795325112867385, 1.000000000000000000, 0.9238795325112867385, 1.000000000000000000, 0.9238795325112867385, 1.000000000000000000, 0.9238795325112867385, 1.000000000000000000, 0.9238795325112867385, 1.000000000000000000, 0.9238795325112867385, 1.000000000000000000, 0.9238795325112867385, 1.000000000000000000, 0.9238795325112867385, 1.000000000000000000, 0.9238795325112867385, 1.000000000000000000, 0.9238795325112867385, 1.000000000000000000, 0.9238795325112867385, 1.000000000000000000, 0.9238795325112867385, 1.000000000000000000, 0.9238795325112867385, 1.000000000000000000, 0.9238795325112867385, 1.000000000000000000, 0.9238795325112867385, 1.000000000000000000, 0.9238795325112867385, 1.000000000000000000, 0.9238795325112867385, 1.000000000000000000, 0.9238795325112867385, 1.000000000000000000, 0.9238795325112867385, 1.000000000000000000, 0.9238795325112867385, 1.000000000000000000, 0.9238795325112867385, 1.000000000000000000, 0.9238795325112867385, 1.000000000000000000, 0.9238795325112867385, 1.000000000000000000, 0.9238795325112867385, 1.000000000000000000, 0.9238795325112867385, 1.000000000000000000, 0.9238795325112867385, 1.000000000000000000, 0.9238795325112867385, 1.000000000000000000, 0.9238795325112867385, 1.000000000000000000, 0.9238795325112867385, 1.000000000000000000, 0.9238795325112867385, 1.000000000000000000, 0.9238795325112867385, 1.000000000000000000, 0.9238795325112867385, 1.000000000000000000, 0.9238795325112867385, 1.000000000000000000, 0.9238795325112867385, 1.000000000000000000, 0.9238795325112867385, 1.000000000000000000, 0.9238795325112867385, 1.000000000000000000, 0.9238795325112867385, 1.000000000000000000, 0.9238795325112867385, 1.000000000000000000, 0.9462258450566536361, 0.9684275698016389100),
 ( 1.000000000000000000, 0.9238795325112867385, 1.000000000000000000, 0.9238795325112867385, 1.000000000000000000, 0.9238795325112867385, 1.000000000000000000, 0.9238795325112867385, 1.000000000000000000, 0.9238795325112867385, 1.000000000000000000, 0.9238795325112867385, 1.000000000000000000, 0.9238795325112867385, 1.000000000000000000, 0.9238795325112867385, 1.000000000000000000, 0.9238795325112867385, 1.000000000000000000, 0.9238795325112867385, 1.000000000000000000, 0.9238795325112867385, 1.000000000000000000, 0.9238795325112867385, 1.000000000000000000, 0.9238795325112867385, 1.000000000000000000, 0.9238795325112867385, 1.000000000000000000, 0.9238795325112867385, 1.000000000000000000, 0.9238795325112867385, 1.000000000000000000, 0.9238795325112867385, 1.000000000000000000, 0.9238795325112867385, 1.000000000000000000, 0.9238795325112867385, 1.000000000000000000, 0.9238795325112867385, 1.000000000000000000, 0.9238795325112867385, 1.000000000000000000, 0.9238795325112867385, 1.000000000000000000, 0.9238795325112867385, 1.000000000000000000, 0.9238795325112867385, 1.000000000000000000, 0.9238795325112867385, 1.000000000000000000, 0.9238795325112867385, 1.000000000000000000, 0.9238795325112867385, 1.000000000000000000, 0.9238795325112867385, 1.000000000000000000, 0.9238795325112867385, 1.000000000000000000, 0.9238795325112867385, 1.000000000000000000, 0.9238795325112867385, 1.000000000000000000, 0.9238795325112867385, 1.000000000000000000, 0.9238795325112867385, 1.000000000000000000, 0.9238795325112867385, 1.000000000000000000, 0.9238795325112867385, 1.000000000000000000, 0.9238795325112867385, 1.000000000000000000, 0.9238795325112867385, 1.000000000000000000, 0.9238795325112867385, 1.000000000000000000, 0.9238795325112867385, 1.000000000000000000, 0.9238795325112867385, 1.000000000000000000, 0.9238795325112867385, 1.000000000000000000, 0.9238795325112867385, 1.000000000000000000, 0.9238795325112867385, 1.000000000000000000, 0.9238795325112867385, 1.000000000000000000, 0.9238795325112867385, 1.000000000000000000, 0.9238795325112867385, 1.000000000000000000, 0.9238795325112867385, 1.000000000000000000, 0.9238795325112867385, 1.000000000000000000, 0.9238795325112867385, 1.000000000000000000, 0.9238795325112867385, 1.000000000000000000, 0.9238795325112867385, 1.000000000000000000, 0.9238795325112867385, 1.000000000000000000, 0.9238795325112867385, 1.000000000000000000, 0.9238795325112867385, 1.000000000000000000, 0.9238795325112867385, 1.000000000000000000, 0.9238795325112867385, 1.000000000000000000, 0.9238795325112867385, 1.000000000000000000, 0.9238795325112867385, 1.000000000000000000, 0.9238795325112867385, 1.000000000000000000, 0.9238795325112867385, 1.000000000000000000, 0.9238795325112867385, 1.000000000000000000, 0.9238795325112867385, 1.000000000000000000, 0.9238795325112867385, 1.000000000000000000, 0.9238795325112867385, 1.000000000000000000, 0.9238795325112867385, 1.000000000000000000, 0.9238795325112867385, 1.000000000000000000, 0.9238795325112867385, 1.000000000000000000, 0.9238795325112867385, 1.000000000000000000, 0.9238795325112867385, 1.000000000000000000, 0.9238795325112867385, 1.000000000000000000, 0.9238795325112867385, 1.000000000000000000, 0.9238795325112867385, 1.000000000000000000, 0.9238795325112867385, 1.000000000000000000, 0.9238795325112867385, 1.000000000000000000, 0.9238795325112867385, 1.000000000000000000, 0.9238795325112867385, 1.000000000000000000, 0.9238795325112867385, 1.000000000000000000, 0.9238795325112867385, 1.000000000000000000, 0.9238795325112867385, 1.000000000000000000, 0.9238795325112867385, 1.000000000000000000, 0.9238795325112867385, 1.000000000000000000, 0.9238795325112867385, 1.000000000000000000, 0.9238795325112867385, 1.000000000000000000, 0.9238795325112867385, 1.000000000000000000, 0.9238795325112867385, 1.000000000000000000, 0.9238795325112867385, 1.000000000000000000, 0.9238795325112867385, 1.000000000000000000, 0.9238795325112867385, 1.000000000000000000, 0.9238795325112867385, 1.000000000000000000, 0.9238795325112867385, 1.000000000000000000, 0.9462258450566536361, 0.9684275698016389100) ) ) 
 REPRESENTATION_ITEM ( '' )  SURFACE ( )  );
#5986 = CARTESIAN_POINT ( 'NONE',  ( 13.14518615778179900, 40.20625000108393010, -5.444914386472297529 ) ) ;
#5987 = CARTESIAN_POINT ( 'NONE',  ( 189.3771271284221314, 36.88242187499999858, -13.57481594606304753 ) ) ;
#5988 = SHAPE_DEFINITION_REPRESENTATION ( #24710, #14045 ) ;
#5989 = DIRECTION ( 'NONE',  ( -0.000000000000000000, -0.000000000000000000, -1.000000000000000000 ) ) ;
#5990 = CARTESIAN_POINT ( 'NONE',  ( 98.15313185440925281, 4.458734125000016313, 3.500000001365592528 ) ) ;
#5991 = CARTESIAN_POINT ( 'NONE',  ( 55.70494972787295751, 38.86679687608393863, -9.295050272127046043 ) ) ;
#5992 = CARTESIAN_POINT ( 'NONE',  ( 104.4587341249999781, 1.846868145590750521, 8.000000001365592084 ) ) ;
#5993 = CARTESIAN_POINT ( 'NONE',  ( 104.3262379212492590, 104.0454443415356991, -51.80000000546238681 ) ) ;
#5994 = CARTESIAN_POINT ( 'NONE',  ( 99.99999999999998579, 91.06249999863440792, 4.458734124999981674 ) ) ;
#5995 = CARTESIAN_POINT ( 'NONE',  ( -11.26481880218173615, 35.99999999999999289, 6.828991891054706720 ) ) ;
#5996 = CARTESIAN_POINT ( 'NONE',  ( 13.57481594606304576, 40.60312499999999858, -1.662435489736055892E-15 ) ) ;
#5997 = CARTESIAN_POINT ( 'NONE',  ( 139.2950502721270425, 40.25585937608393294, 9.295050272127046043 ) ) ;
#5998 = ORIENTED_EDGE ( 'NONE', *, *, #19646, .T. ) ;
#5999 = CARTESIAN_POINT ( 'NONE',  ( 104.4587341249999781, 82.25000000136559208, -1.846868145590750299 ) ) ;
#6000 = EDGE_CURVE ( 'NONE', #4040, #15812, #8386, .T. ) ;
#6001 = CARTESIAN_POINT ( 'NONE',  ( -8.312177448680279460E-16, 31.37578125216787583, -13.57481594606304576 ) ) ;
#6002 = VERTEX_POINT ( 'NONE', #8670 ) ;
#6003 = ORIENTED_EDGE ( 'NONE', *, *, #22404, .T. ) ;
#6004 = EDGE_CURVE ( 'NONE', #24017, #21579, #6395, .T. ) ;
#6005 = CARTESIAN_POINT ( 'NONE',  ( 139.1801758136479918, 55.00000000000000000, -15.00000000000000000 ) ) ;
#6006 = CARTESIAN_POINT ( 'NONE',  ( 95.54126587499996504, 1.387778780781445676E-14, 8.687500001365592084 ) ) ;
#6007 = EDGE_CURVE ( 'NONE', #11095, #10159, #12374, .T. ) ;
#6008 = ORIENTED_EDGE ( 'NONE', *, *, #15615, .T. ) ;
#6009 = CARTESIAN_POINT ( 'NONE',  ( 108.0825317500000153, 110.0000000000000000, -50.37500000273119127 ) ) ;
#6010 = CARTESIAN_POINT ( 'NONE',  ( -5.444914386472297529, 34.05468750108393294, -13.14518615778179900 ) ) ;
#6011 = CARTESIAN_POINT ( 'NONE',  ( 208.5748159460630120, 37.57695312716787583, -5.622872871577873077 ) ) ;
#6012 = CARTESIAN_POINT ( 'NONE',  ( 104.3262379212492448, 115.9545556584642867, -53.69999999999999574 ) ) ;
#6013 = EDGE_CURVE ( 'NONE', #3638, #7806, #18897, .T. ) ;
#6014 = FACE_OUTER_BOUND ( 'NONE', #2341, .T. ) ;
#6015 = CARTESIAN_POINT ( 'NONE',  ( 197.0246277255383234, 50.00000000050969362, 13.43320860980889897 ) ) ;
#6016 = CARTESIAN_POINT ( 'NONE',  ( 143.1451861577818363, 38.02343750108395426, -5.444914386472297529 ) ) ;
#6017 = CARTESIAN_POINT ( 'NONE',  ( -13.14518615778179900, 32.56640625108394005, -5.444914386472297529 ) ) ;
#6018 = VERTEX_POINT ( 'NONE', #19505 ) ;
#6019 = CARTESIAN_POINT ( 'NONE',  ( 55.40115559117954547, 36.33671874999999574, 9.598844408820459861 ) ) ;
#6020 = DIRECTION ( 'NONE',  ( 1.000000000000000000, 0.000000000000000000, 0.000000000000000000 ) ) ;
#6021 = EDGE_CURVE ( 'NONE', #18802, #26308, #4144, .T. ) ;
#6022 = CARTESIAN_POINT ( 'NONE',  ( 206.2065315021356753, 36.00000000000000000, 7.323573988460882589 ) ) ;
#6023 = CARTESIAN_POINT ( 'NONE',  ( 103.1528011352953342, 3.152801135295383084, 2.062500001365591640 ) ) ;
#6024 = CARTESIAN_POINT ( 'NONE',  ( 5.444914386472302859, 33.06250000108393294, 13.14518615778179189 ) ) ;
#6025 = CARTESIAN_POINT ( 'NONE',  ( 104.4587341249999781, 1.846868145590750521, 3.250000001365592972 ) ) ;
#6026 = CARTESIAN_POINT ( 'NONE',  ( 96.84719886470459471, 82.56250000136559208, -3.152801135295383084 ) ) ;
#6027 = CARTESIAN_POINT ( 'NONE',  ( -13.14518615778179544, 33.40976562608393863, 0.000000000000000000 ) ) ;
#6028 = CARTESIAN_POINT ( 'NONE',  ( 9.295050272127046043, 40.45429687608393721, -9.295050272127046043 ) ) ;
#6029 = CARTESIAN_POINT ( 'NONE',  ( 195.0000000000000000, 38.42031249999999432, -13.57481594606304576 ) ) ;
#6030 = VERTEX_POINT ( 'NONE', #19225 ) ;
#6031 = CARTESIAN_POINT ( 'NONE',  ( -9.295050272127044266, 32.91367187608393152, 9.295050272127047819 ) ) ;
#6032 =( BOUNDED_SURFACE ( )  B_SPLINE_SURFACE ( 1, 2, ( 
 ( #26060, #23509, #8672, #13059, #3988, #21653, #12504, #5986, #19226, #25507, #2128, #14652, #14930, #15206, #10793, #25923, #17364, #19507, #8387, #6528, #23371, #21376, #10934, #8114, #19084, #25778, #21233, #6256, #2275, #1716, #8249, #23926, #27654, #10377, #18138, #16808, #12790, #4405, #23650, #12651, #14786, #4125, #6397, #27791, #16937, #25637, #6120, #21508, #23784, #1989, #10655, #1854, #19363, #28066, #8532, #17218, #8812, #15351, #2555, #13778, #24491, #19931, #4976, #9098, #26351, #557, #26495, #24637, #15647, #24210, #7230, #8954, #11499, #22500, #21939, #9374, #18070, #6952, #26785, #269, #26202, #2965, #24345, #20216, #15921, #17644, #17793, #11215, #13497, #6810, #19644, #127, #5113, #17502, #6666, #414, #4836, #24067, #22217, #15498, #2695, #11356, #19787, #13641, #4543, #20079, #4689, #13205, #9239, #2416, #11075, #13349, #22078, #17931, #22356, #26641, #7088, #15788, #2831, #701, #12574, #23438, #25059, #23577, #9521, #10449, #24775, #21301, #1267, #26929, #9931, #5256, #991, #7372, #5681, #25194, #1131, #9800, #27069, #11640, #22648, #3117, #14069, #3915, #27859, #11926, #16067, #25709, #1783, #17005, #16215, #22929, #20508, #16359, #3390, #11785, #20786, #14860, #19156, #22789, #18220, #18506, #8319, #5545, #12061, #20363, #6190, #7520, #848, #13920, #27212, #14209, #9659, #18361, #24916, #5400, #3259, #20648, #7667, #18646, #27351, #7809, #16499 ),
 ( #14720, #4614, #11140, #12853, #2202, #23854, #26132, #21581, #6883, #12719, #9031, #19856, #343, #25992, #8459, #19714, #23718, #19576, #17572, #2479, #26278, #10863, #13133, #25850, #17433, #19435, #6739, #15424, #14998, #12989, #24137, #6323, #21729, #60, #17723, #28134, #13273, #26425, #8602, #8882, #17148, #10591, #4332, #1923, #22003, #19298, #8740, #15570, #4057, #2345, #21445, #27998, #15135, #4194, #2058, #6461, #10727, #17290, #6598, #15281, #24000, #4476, #21868, #11001, #199, #13991, #24278, #26566, #917, #18435, #9445, #22717, #22431, #20150, #11430, #15855, #3041, #22145, #11287, #9588, #27143, #2899, #11711, #772, #24564, #4905, #18002, #13567, #11855, #629, #13419, #20008, #7159, #7595, #18292, #5045, #26998, #13710, #2766, #5186, #11569, #1060, #20286, #9304, #20577, #22290, #16141, #4759, #7019, #3185, #9730, #18145, #2625, #26710, #488, #9170, #26859, #24849, #17862, #7305, #15992, #24706, #13849, #22574, #15714, #24416, #20436, #7445, #5327, #10001, #20718, #3747, #7735, #3609, #1614, #14688, #10272, #23132, #25407, #9869, #1474, #3463, #18981, #27690, #27279, #25258, #8153, #18576, #5749, #12268, #1201, #16846, #25544, #16425, #12408, #6024, #25121, #23407, #21128, #16567, #3882, #12543, #24986, #14417, #20994, #14275, #5609, #21269, #1753, #27410, #10419, #10131, #16709, #22993, #3323, #19125, #18843, #27832, #12128, #16285, #20855, #18708, #1337 ) ),
 .UNSPECIFIED., .F., .F., .F. ) 
 B_SPLINE_SURFACE_WITH_KNOTS ( ( 2, 2 ),
 ( 3, 2, 2, 2, 2, 2, 2, 2, 2, 2, 2, 2, 2, 2, 2, 2, 2, 2, 2, 2, 2, 2, 2, 2, 2, 2, 2, 2, 2, 2, 2, 2, 2, 2, 2, 2, 2, 2, 2, 2, 2, 2, 2, 2, 2, 2, 2, 2, 2, 2, 2, 2, 2, 2, 2, 2, 2, 2, 2, 2, 2, 2, 2, 2, 2, 2, 2, 2, 2, 2, 2, 2, 2, 2, 2, 2, 2, 2, 2, 2, 2, 2, 2, 2, 2, 2, 2, 2, 2, 2, 2, 3 ),
 ( 0.000000000000000000, 1.000000000000000000 ),
 ( 0.000000000000000000, 0.01041666666666666609, 0.02083333333333333218, 0.03125000000000000000, 0.04166666666666666435, 0.05208333333333333565, 0.06250000000000000000, 0.07291666666666667129, 0.08333333333333332871, 0.09375000000000000000, 0.1041666666666666713, 0.1145833333333333287, 0.1250000000000000000, 0.1354166666666666574, 0.1458333333333333426, 0.1562500000000000000, 0.1666666666666666574, 0.1770833333333333426, 0.1875000000000000000, 0.1979166666666666574, 0.2083333333333333426, 0.2187500000000000000, 0.2291666666666666574, 0.2395833333333333426, 0.2500000000000000000, 0.2604166666666666852, 0.2708333333333333148, 0.2812500000000000000, 0.2916666666666666852, 0.3020833333333333148, 0.3125000000000000000, 0.3229166666666666852, 0.3333333333333333148, 0.3437500000000000000, 0.3541666666666666852, 0.3645833333333333148, 0.3750000000000000000, 0.3854166666666666852, 0.3958333333333333148, 0.4062500000000000000, 0.4166666666666666852, 0.4270833333333333148, 0.4375000000000000000, 0.4479166666666666852, 0.4583333333333333148, 0.4687500000000000000, 0.4791666666666666852, 0.4895833333333333148, 0.5000000000000000000, 0.5104166666666666297, 0.5208333333333333703, 0.5312500000000000000, 0.5416666666666666297, 0.5520833333333333703, 0.5625000000000000000, 0.5729166666666666297, 0.5833333333333333703, 0.5937500000000000000, 0.6041666666666666297, 0.6145833333333333703, 0.6250000000000000000, 0.6354166666666666297, 0.6458333333333333703, 0.6562500000000000000, 0.6666666666666666297, 0.6770833333333333703, 0.6875000000000000000, 0.6979166666666666297, 0.7083333333333333703, 0.7187500000000000000, 0.7291666666666666297, 0.7395833333333333703, 0.7500000000000000000, 0.7604166666666666297, 0.7708333333333333703, 0.7812500000000000000, 0.7916666666666666297, 0.8020833333333333703, 0.8125000000000000000, 0.8229166666666666297, 0.8333333333333333703, 0.8437500000000000000, 0.8541666666666666297, 0.8645833333333333703, 0.8750000000000000000, 0.8854166666666666297, 0.8958333333333333703, 0.9062500000000000000, 0.9166666666666666297, 0.9270833333333333703, 0.9375000000000000000, 0.9448587001587775980 ),
 .UNSPECIFIED. ) 
 GEOMETRIC_REPRESENTATION_ITEM ( )  RATIONAL_B_SPLINE_SURFACE ( (
 ( 1.000000000000000000, 0.9238795325112867385, 1.000000000000000000, 0.9238795325112867385, 1.000000000000000000, 0.9238795325112867385, 1.000000000000000000, 0.9238795325112867385, 1.000000000000000000, 0.9238795325112867385, 1.000000000000000000, 0.9238795325112867385, 1.000000000000000000, 0.9238795325112867385, 1.000000000000000000, 0.9238795325112867385, 1.000000000000000000, 0.9238795325112867385, 1.000000000000000000, 0.9238795325112867385, 1.000000000000000000, 0.9238795325112867385, 1.000000000000000000, 0.9238795325112867385, 1.000000000000000000, 0.9238795325112867385, 1.000000000000000000, 0.9238795325112867385, 1.000000000000000000, 0.9238795325112867385, 1.000000000000000000, 0.9238795325112867385, 1.000000000000000000, 0.9238795325112867385, 1.000000000000000000, 0.9238795325112867385, 1.000000000000000000, 0.9238795325112867385, 1.000000000000000000, 0.9238795325112867385, 1.000000000000000000, 0.9238795325112867385, 1.000000000000000000, 0.9238795325112867385, 1.000000000000000000, 0.9238795325112867385, 1.000000000000000000, 0.9238795325112867385, 1.000000000000000000, 0.9238795325112867385, 1.000000000000000000, 0.9238795325112867385, 1.000000000000000000, 0.9238795325112867385, 1.000000000000000000, 0.9238795325112867385, 1.000000000000000000, 0.9238795325112867385, 1.000000000000000000, 0.9238795325112867385, 1.000000000000000000, 0.9238795325112867385, 1.000000000000000000, 0.9238795325112867385, 1.000000000000000000, 0.9238795325112867385, 1.000000000000000000, 0.9238795325112867385, 1.000000000000000000, 0.9238795325112867385, 1.000000000000000000, 0.9238795325112867385, 1.000000000000000000, 0.9238795325112867385, 1.000000000000000000, 0.9238795325112867385, 1.000000000000000000, 0.9238795325112867385, 1.000000000000000000, 0.9238795325112867385, 1.000000000000000000, 0.9238795325112867385, 1.000000000000000000, 0.9238795325112867385, 1.000000000000000000, 0.9238795325112867385, 1.000000000000000000, 0.9238795325112867385, 1.000000000000000000, 0.9238795325112867385, 1.000000000000000000, 0.9238795325112867385, 1.000000000000000000, 0.9238795325112867385, 1.000000000000000000, 0.9238795325112867385, 1.000000000000000000, 0.9238795325112867385, 1.000000000000000000, 0.9238795325112867385, 1.000000000000000000, 0.9238795325112867385, 1.000000000000000000, 0.9238795325112867385, 1.000000000000000000, 0.9238795325112867385, 1.000000000000000000, 0.9238795325112867385, 1.000000000000000000, 0.9238795325112867385, 1.000000000000000000, 0.9238795325112867385, 1.000000000000000000, 0.9238795325112867385, 1.000000000000000000, 0.9238795325112867385, 1.000000000000000000, 0.9238795325112867385, 1.000000000000000000, 0.9238795325112867385, 1.000000000000000000, 0.9238795325112867385, 1.000000000000000000, 0.9238795325112867385, 1.000000000000000000, 0.9238795325112867385, 1.000000000000000000, 0.9238795325112867385, 1.000000000000000000, 0.9238795325112867385, 1.000000000000000000, 0.9238795325112867385, 1.000000000000000000, 0.9238795325112867385, 1.000000000000000000, 0.9238795325112867385, 1.000000000000000000, 0.9238795325112867385, 1.000000000000000000, 0.9238795325112867385, 1.000000000000000000, 0.9238795325112867385, 1.000000000000000000, 0.9238795325112867385, 1.000000000000000000, 0.9238795325112867385, 1.000000000000000000, 0.9238795325112867385, 1.000000000000000000, 0.9238795325112867385, 1.000000000000000000, 0.9238795325112867385, 1.000000000000000000, 0.9238795325112867385, 1.000000000000000000, 0.9238795325112867385, 1.000000000000000000, 0.9238795325112867385, 1.000000000000000000, 0.9238795325112867385, 1.000000000000000000, 0.9238795325112867385, 1.000000000000000000, 0.9238795325112867385, 1.000000000000000000, 0.9238795325112867385, 1.000000000000000000, 0.9238795325112867385, 1.000000000000000000, 0.9238795325112867385, 1.000000000000000000, 0.9238795325112867385, 1.000000000000000000, 0.9238795325112867385, 1.000000000000000000, 0.9238795325112867385, 1.000000000000000000, 0.9238795325112867385, 1.000000000000000000, 0.9238795325112867385, 1.000000000000000000, 0.9462258211652395667, 0.9684275895297407288),
 ( 1.000000000000000000, 0.9238795325112867385, 1.000000000000000000, 0.9238795325112867385, 1.000000000000000000, 0.9238795325112867385, 1.000000000000000000, 0.9238795325112867385, 1.000000000000000000, 0.9238795325112867385, 1.000000000000000000, 0.9238795325112867385, 1.000000000000000000, 0.9238795325112867385, 1.000000000000000000, 0.9238795325112867385, 1.000000000000000000, 0.9238795325112867385, 1.000000000000000000, 0.9238795325112867385, 1.000000000000000000, 0.9238795325112867385, 1.000000000000000000, 0.9238795325112867385, 1.000000000000000000, 0.9238795325112867385, 1.000000000000000000, 0.9238795325112867385, 1.000000000000000000, 0.9238795325112867385, 1.000000000000000000, 0.9238795325112867385, 1.000000000000000000, 0.9238795325112867385, 1.000000000000000000, 0.9238795325112867385, 1.000000000000000000, 0.9238795325112867385, 1.000000000000000000, 0.9238795325112867385, 1.000000000000000000, 0.9238795325112867385, 1.000000000000000000, 0.9238795325112867385, 1.000000000000000000, 0.9238795325112867385, 1.000000000000000000, 0.9238795325112867385, 1.000000000000000000, 0.9238795325112867385, 1.000000000000000000, 0.9238795325112867385, 1.000000000000000000, 0.9238795325112867385, 1.000000000000000000, 0.9238795325112867385, 1.000000000000000000, 0.9238795325112867385, 1.000000000000000000, 0.9238795325112867385, 1.000000000000000000, 0.9238795325112867385, 1.000000000000000000, 0.9238795325112867385, 1.000000000000000000, 0.9238795325112867385, 1.000000000000000000, 0.9238795325112867385, 1.000000000000000000, 0.9238795325112867385, 1.000000000000000000, 0.9238795325112867385, 1.000000000000000000, 0.9238795325112867385, 1.000000000000000000, 0.9238795325112867385, 1.000000000000000000, 0.9238795325112867385, 1.000000000000000000, 0.9238795325112867385, 1.000000000000000000, 0.9238795325112867385, 1.000000000000000000, 0.9238795325112867385, 1.000000000000000000, 0.9238795325112867385, 1.000000000000000000, 0.9238795325112867385, 1.000000000000000000, 0.9238795325112867385, 1.000000000000000000, 0.9238795325112867385, 1.000000000000000000, 0.9238795325112867385, 1.000000000000000000, 0.9238795325112867385, 1.000000000000000000, 0.9238795325112867385, 1.000000000000000000, 0.9238795325112867385, 1.000000000000000000, 0.9238795325112867385, 1.000000000000000000, 0.9238795325112867385, 1.000000000000000000, 0.9238795325112867385, 1.000000000000000000, 0.9238795325112867385, 1.000000000000000000, 0.9238795325112867385, 1.000000000000000000, 0.9238795325112867385, 1.000000000000000000, 0.9238795325112867385, 1.000000000000000000, 0.9238795325112867385, 1.000000000000000000, 0.9238795325112867385, 1.000000000000000000, 0.9238795325112867385, 1.000000000000000000, 0.9238795325112867385, 1.000000000000000000, 0.9238795325112867385, 1.000000000000000000, 0.9238795325112867385, 1.000000000000000000, 0.9238795325112867385, 1.000000000000000000, 0.9238795325112867385, 1.000000000000000000, 0.9238795325112867385, 1.000000000000000000, 0.9238795325112867385, 1.000000000000000000, 0.9238795325112867385, 1.000000000000000000, 0.9238795325112867385, 1.000000000000000000, 0.9238795325112867385, 1.000000000000000000, 0.9238795325112867385, 1.000000000000000000, 0.9238795325112867385, 1.000000000000000000, 0.9238795325112867385, 1.000000000000000000, 0.9238795325112867385, 1.000000000000000000, 0.9238795325112867385, 1.000000000000000000, 0.9238795325112867385, 1.000000000000000000, 0.9238795325112867385, 1.000000000000000000, 0.9238795325112867385, 1.000000000000000000, 0.9238795325112867385, 1.000000000000000000, 0.9238795325112867385, 1.000000000000000000, 0.9238795325112867385, 1.000000000000000000, 0.9238795325112867385, 1.000000000000000000, 0.9238795325112867385, 1.000000000000000000, 0.9238795325112867385, 1.000000000000000000, 0.9238795325112867385, 1.000000000000000000, 0.9238795325112867385, 1.000000000000000000, 0.9238795325112867385, 1.000000000000000000, 0.9238795325112867385, 1.000000000000000000, 0.9238795325112867385, 1.000000000000000000, 0.9238795325112867385, 1.000000000000000000, 0.9462258211652395667, 0.9684275895297407288) ) ) 
 REPRESENTATION_ITEM ( '' )  SURFACE ( )  );
#6033 = DIRECTION ( 'NONE',  ( -0.000000000000000000, -1.000000000000000000, -0.000000000000000000 ) ) ;
#6034 = LINE ( 'NONE', #25554, #8916 ) ;
#6035 = CARTESIAN_POINT ( 'NONE',  ( 101.5243464873929042, 123.0000000000000000, -1.749128039131298884 ) ) ;
#6036 = EDGE_CURVE ( 'NONE', #11583, #21223, #3986, .T. ) ;
#6037 = CARTESIAN_POINT ( 'NONE',  ( 97.92893218813448186, 93.31249999999998579, -4.999999999999963585 ) ) ;
#6038 = ORIENTED_EDGE ( 'NONE', *, *, #21365, .T. ) ;
#6039 = CARTESIAN_POINT ( 'NONE',  ( 51.85481384221820633, 39.16445312608393436, 0.000000000000000000 ) ) ;
#6040 = CARTESIAN_POINT ( 'NONE',  ( 97.83688103937537051, 103.3426043859339103, -54.60000000000000853 ) ) ;
#6041 = CARTESIAN_POINT ( 'NONE',  ( 68.86541437541316668, 54.10683252460148651, -15.00000000000000178 ) ) ;
#6042 = ORIENTED_EDGE ( 'NONE', *, *, #13151, .F. ) ;
#6043 = DIRECTION ( 'NONE',  ( 0.000000000000000000, 0.000000000000000000, 1.000000000000000000 ) ) ;
#6044 = ADVANCED_FACE ( 'NONE', ( #27926 ), #23370, .T. ) ;
#6045 = CARTESIAN_POINT ( 'NONE',  ( 181.6399989480775901, 40.87597656304196647, 0.000000000000000000 ) ) ;
#6046 = CARTESIAN_POINT ( 'NONE',  ( 191.1345856245867765, 54.10683252460147230, 14.99999999999994493 ) ) ;
#6047 = EDGE_CURVE ( 'NONE', #24596, #9425, #12919, .T. ) ;
#6048 = CIRCLE ( 'NONE', #4210, 22.40192378864669109 ) ;
#6049 = CARTESIAN_POINT ( 'NONE',  ( 143.5748159460630688, 35.93984375216787441, -1.662435489736055892E-15 ) ) ;
#6050 =( REPRESENTATION_RELATIONSHIP ('NONE','NONE', #2411, #14045 ) REPRESENTATION_RELATIONSHIP_WITH_TRANSFORMATION ( #18813 )SHAPE_REPRESENTATION_RELATIONSHIP( ) );
#6051 = CARTESIAN_POINT ( 'NONE',  ( 134.1572863549629062, 35.99999999999997868, -12.92256159328817411 ) ) ;
#6052 = CARTESIAN_POINT ( 'NONE',  ( 130.0000000000000000, 37.72578125216787726, -13.57481594606304576 ) ) ;
#6053 = CARTESIAN_POINT ( 'NONE',  ( 189.5550856135277229, 39.31328125108394289, 13.14518615778179722 ) ) ;
#6054 = ORIENTED_EDGE ( 'NONE', *, *, #3941, .F. ) ;
#6055 = ORIENTED_EDGE ( 'NONE', *, *, #10957, .T. ) ;
#6056 = SURFACE_STYLE_USAGE ( .BOTH. , #4333 ) ;
#6057 = DIRECTION ( 'NONE',  ( -0.000000000000000000, -0.000000000000000000, -1.000000000000000000 ) ) ;
#6058 = CARTESIAN_POINT ( 'NONE',  ( 1.662435489736055892E-15, 36.00000000000000000, 13.57481594606304576 ) ) ;
#6059 = CARTESIAN_POINT ( 'NONE',  ( 97.83688103937537051, 103.3426043859339103, -52.10000000546238397 ) ) ;
#6060 = DIRECTION ( 'NONE',  ( 0.000000000000000000, -0.000000000000000000, 1.000000000000000000 ) ) ;
#6061 = CARTESIAN_POINT ( 'NONE',  ( 5.444914386472297529, 39.71015625108393010, -13.14518615778179722 ) ) ;
#6062 = FACE_OUTER_BOUND ( 'NONE', #28198, .T. ) ;
#6063 = DIRECTION ( 'NONE',  ( 0.000000000000000000, 0.000000000000000000, 1.000000000000000000 ) ) ;
#6064 = CARTESIAN_POINT ( 'NONE',  ( 108.0825317499999869, 112.6261737610028320, -46.52499999726882152 ) ) ;
#6065 = ORIENTED_EDGE ( 'NONE', *, *, #8879, .T. ) ;
#6066 = CARTESIAN_POINT ( 'NONE',  ( 9.598844408820459861, 38.91640624999999432, 9.598844408820456309 ) ) ;
#6067 = CARTESIAN_POINT ( 'NONE',  ( -9.295050272127044266, 39.06523437608392868, 9.295050272127047819 ) ) ;
#6068 = CARTESIAN_POINT ( 'NONE',  ( 99.99999999999995737, 4.458734125000016313, 14.18750000136559208 ) ) ;
#6069 = CARTESIAN_POINT ( 'NONE',  ( 135.4449143864723055, 38.91640625108393436, -13.14518615778179900 ) ) ;
#6070 = CARTESIAN_POINT ( 'NONE',  ( 65.00000000000000000, 38.37070312608393152, 13.14518615778179544 ) ) ;
#6071 = EDGE_CURVE ( 'NONE', #16704, #17997, #2371, .T. ) ;
#6072 = CARTESIAN_POINT ( 'NONE',  ( 189.5550856135277229, 40.60312500108393863, -13.14518615778179900 ) ) ;
#6073 = PLANE ( 'NONE',  #25696 ) ;
#6074 = CARTESIAN_POINT ( 'NONE',  ( 5.444914386472302859, 36.83281250108392868, 13.14518615778179189 ) ) ;
#6075 = CARTESIAN_POINT ( 'NONE',  ( 65.00000000000000000, 36.03906250000000000, -13.57481594606304576 ) ) ;
#6076 = CARTESIAN_POINT ( 'NONE',  ( -9.598844408820454532, 38.81718750216787583, 9.598844408820459861 ) ) ;
#6077 = CYLINDRICAL_SURFACE ( 'NONE', #8524, 13.57481594606304398 ) ;
#6078 = CARTESIAN_POINT ( 'NONE',  ( -9.295050272127044266, 39.06523437608392868, 9.295050272127047819 ) ) ;
#6079 = DIRECTION ( 'NONE',  ( -5.782411586589357392E-17, 0.000000000000000000, -1.000000000000000000 ) ) ;
#6080 = CARTESIAN_POINT ( 'NONE',  ( 98.23223304703363112, 123.5000000000000000, 1.767766952966351557 ) ) ;
#6081 = CARTESIAN_POINT ( 'NONE',  ( 101.4615807364564546, 123.4500000010924765, 1.461580736456455476 ) ) ;
#6082 = CARTESIAN_POINT ( 'NONE',  ( 102.0669872999999797, 123.5500000010924708, -9.794112055954760458E-15 ) ) ;
#6083 = VECTOR ( 'NONE', #24732, 1000.000000000000000 ) ;
#6084 = CARTESIAN_POINT ( 'NONE',  ( -5.622872871577736298, 36.88242187499999858, -13.57481594606318254 ) ) ;
#6085 = CARTESIAN_POINT ( 'NONE',  ( 99.99999999999995737, 4.458734125000016313, 12.18750000136559208 ) ) ;
#6086 = CARTESIAN_POINT ( 'NONE',  ( 97.92893218813451028, -4.999999999999989342, 13.31250000273118594 ) ) ;
#6087 = CYLINDRICAL_SURFACE ( 'NONE', #10241, 13.57481594606304576 ) ;
#6088 = CARTESIAN_POINT ( 'NONE',  ( -5.622872871577873077, 40.85117187499999147, -13.57481594606304753 ) ) ;
#6089 = CARTESIAN_POINT ( 'NONE',  ( -9.295050272127044266, 31.92148437608393508, 9.295050272127047819 ) ) ;
#6090 = CARTESIAN_POINT ( 'NONE',  ( 9.598844408820459861, 33.45937500216787441, 9.598844408820456309 ) ) ;
#6091 = CARTESIAN_POINT ( 'NONE',  ( 99.99999999999995737, 80.25000000000000000, 4.999999999999990230 ) ) ;
#6092 = CARTESIAN_POINT ( 'NONE',  ( 96.84719886470459471, 80.31250000136559208, -3.152801135295383084 ) ) ;
#6093 = CARTESIAN_POINT ( 'NONE',  ( 55.70494972787295751, 38.27148437608393294, -9.295050272127046043 ) ) ;
#6094 = CARTESIAN_POINT ( 'NONE',  ( 91.91746824999998466, 107.3738262389971538, -51.27500000273119696 ) ) ;
#6095 = CYLINDRICAL_SURFACE ( 'NONE', #4576, 7.000000000000006217 ) ;
#6096 = VERTEX_POINT ( 'NONE', #14785 ) ;
#6097 = DIRECTION ( 'NONE',  ( 0.000000000000000000, 0.000000000000000000, -1.000000000000000000 ) ) ;
#6098 = FACE_OUTER_BOUND ( 'NONE', #8377, .T. ) ;
#6099 = CARTESIAN_POINT ( 'NONE',  ( 107.0000000000000000, 110.0000000000000000, -49.49999999453764588 ) ) ;
#6100 = CARTESIAN_POINT ( 'NONE',  ( 130.0000000000000000, 40.80156249999999574, -13.57481594606304576 ) ) ;
#6101 = ORIENTED_EDGE ( 'NONE', *, *, #13351, .T. ) ;
#6102 = CARTESIAN_POINT ( 'NONE',  ( 3.116592080465746761, 53.90895096933311237, -15.00000000000000178 ) ) ;
#6103 = CARTESIAN_POINT ( 'NONE',  ( 5.444914386472302859, 38.61875000108393152, 13.14518615778179189 ) ) ;
#6104 = CARTESIAN_POINT ( 'NONE',  ( 13.57481594606304931, 39.85898437716787157, 5.622872871577869525 ) ) ;
#6105 = CARTESIAN_POINT ( 'NONE',  ( 135.4449143864723055, 40.30546875108393579, -13.14518615778179900 ) ) ;
#6106 = CARTESIAN_POINT ( 'NONE',  ( 74.59884440882045453, 37.42812500216787441, 9.598844408820456309 ) ) ;
#6107 = CARTESIAN_POINT ( 'NONE',  ( 95.00472066334982912, 103.1245878333314323, -53.32499999726881157 ) ) ;
#6108 = CARTESIAN_POINT ( 'NONE',  ( 5.622872871577871301, 36.88242187716787157, -13.57481594606304753 ) ) ;
#6109 = EDGE_LOOP ( 'NONE', ( #6544, #18119, #12285, #19575 ) ) ;
#6110 = CARTESIAN_POINT ( 'NONE',  ( 99.99999999999995737, -4.999999999999990230, 7.249999999999999112 ) ) ;
#6111 = CARTESIAN_POINT ( 'NONE',  ( 97.83688103937538472, 116.6573956140660897, -52.40000000000000568 ) ) ;
#6112 = AXIS2_PLACEMENT_3D ( 'NONE', #7570, #5449, #10252 ) ;
#6113 = CARTESIAN_POINT ( 'NONE',  ( 200.4449143864723055, 36.03906250108394005, 13.14518615778179189 ) ) ;
#6114 = CARTESIAN_POINT ( 'NONE',  ( 13.57481594606304931, 35.89023437716787868, 5.622872871577868636 ) ) ;
#6115 = CARTESIAN_POINT ( 'NONE',  ( 139.2950502721270425, 37.87460937608393152, -9.295050272127046043 ) ) ;
#6116 = CARTESIAN_POINT ( 'NONE',  ( 93.00000000000000000, 110.0000000000000000, -55.00000000000000711 ) ) ;
#6117 = DIRECTION ( 'NONE',  ( 0.000000000000000000, 0.000000000000000000, 1.000000000000000000 ) ) ;
#6118 = DIRECTION ( 'NONE',  ( -0.000000000000000000, 1.000000000000000000, -0.000000000000000000 ) ) ;
#6119 = CARTESIAN_POINT ( 'NONE',  ( 92.99999999999997158, 107.7255621263696810, -48.90000000000001279 ) ) ;
#6120 = CARTESIAN_POINT ( 'NONE',  ( -9.295050272127044266, 38.27148437608393294, 9.295050272127047819 ) ) ;
#6121 = CARTESIAN_POINT ( 'NONE',  ( 208.5748159460630120, 36.68398437499999432, -5.622872871577873077 ) ) ;
#6122 = CONTEXT_DEPENDENT_SHAPE_REPRESENTATION ( #13297, #22677 ) ;
#6123 = CARTESIAN_POINT ( 'NONE',  ( -8.312177448680279460E-16, 36.03906250000000000, -13.57481594606304576 ) ) ;
#6124 = CARTESIAN_POINT ( 'NONE',  ( 104.4587341249999781, -1.846868145590721655, 4.125000001365592084 ) ) ;
#6125 = CARTESIAN_POINT ( 'NONE',  ( 51.85481384221820633, 39.75976562608393294, 0.000000000000000000 ) ) ;
#6126 = EDGE_CURVE ( 'NONE', #25694, #5706, #24758, .T. ) ;
#6127 = CARTESIAN_POINT ( 'NONE',  ( 99.99999999999995737, 4.458734125000016313, 4.187500001365592084 ) ) ;
#6128 = DIRECTION ( 'NONE',  ( 0.000000000000000000, 0.000000000000000000, -1.000000000000000000 ) ) ;
#6129 = CARTESIAN_POINT ( 'NONE',  ( 103.1528011352953484, 91.18749999863440792, 3.152801135295352886 ) ) ;
#6130 = CARTESIAN_POINT ( 'NONE',  ( -2.117096883972749467E-15, 29.95886589889650509, -11.57481594606304576 ) ) ;
#6131 = CARTESIAN_POINT ( 'NONE',  ( -5.622872871577873077, 40.05742187499999574, -13.57481594606304753 ) ) ;
#6132 = CARTESIAN_POINT ( 'NONE',  ( 143.1451861577818079, 39.61093750108393863, -5.444914386472297529 ) ) ;
#6133 = ORIENTED_EDGE ( 'NONE', *, *, #3595, .T. ) ;
#6134 = CARTESIAN_POINT ( 'NONE',  ( 104.4587341249999639, 84.18750000136560629, -1.442382525525748735E-14 ) ) ;
#6135 = CARTESIAN_POINT ( 'NONE',  ( 92.99999999999998579, 110.0000000000000000, -51.00000000000000711 ) ) ;
#6136 = ORIENTED_EDGE ( 'NONE', *, *, #14706, .T. ) ;
#6137 = CARTESIAN_POINT ( 'NONE',  ( 130.0000000000000000, 38.91640625216786731, 13.57481594606304576 ) ) ;
#6138 = CARTESIAN_POINT ( 'NONE',  ( 51.85481384221819923, 35.14609375108393152, -5.444914386472297529 ) ) ;
#6139 =( BOUNDED_CURVE ( )  B_SPLINE_CURVE ( 2, ( #5785, #14452, #19161, #27865, #1646, #5924, #25857, #12858, #16879 ),
 .UNSPECIFIED., .F., .T. ) 
 B_SPLINE_CURVE_WITH_KNOTS ( ( 3, 2, 2, 2, 3 ),
 ( 0.02083333333333358892, 0.03125000000000020123, 0.04166666666666681007, 0.05208333333333342585, 0.06250000000000004163 ),
 .UNSPECIFIED. ) 
 CURVE ( )  GEOMETRIC_REPRESENTATION_ITEM ( )  RATIONAL_B_SPLINE_CURVE ( ( 0.9999999999999981126, 0.9238795325112886259, 1.000000000000000000, 0.9238795325112867385, 1.000000000000000000, 0.9238795325112867385, 1.000000000000000000, 0.9238795325112864054, 1.000000000000000222 ) ) 
 REPRESENTATION_ITEM ( '' )  );
#6140 = ORIENTED_EDGE ( 'NONE', *, *, #8955, .T. ) ;
#6141 = CARTESIAN_POINT ( 'NONE',  ( -8.312177448680279460E-16, 32.96328125216787441, -13.57481594606304576 ) ) ;
#6142 = CARTESIAN_POINT ( 'NONE',  ( 103.1528011352953342, -3.152801135295355106, 2.062500001365591640 ) ) ;
#6143 = ORIENTED_EDGE ( 'NONE', *, *, #930, .T. ) ;
#6144 = CARTESIAN_POINT ( 'NONE',  ( 13.14518615778179544, 34.79882812608394005, -1.609821015232357215E-15 ) ) ;
#6145 = CARTESIAN_POINT ( 'NONE',  ( 9.295050272127046043, 32.31835937608393294, -9.295050272127046043 ) ) ;
#6146 = CARTESIAN_POINT ( 'NONE',  ( 208.5748159460630120, 39.06523437716786873, 5.622872871577869525 ) ) ;
#6147 = CARTESIAN_POINT ( 'NONE',  ( 97.83688103937535629, 116.6573956140660897, -53.40000000000001990 ) ) ;
#6148 = CARTESIAN_POINT ( 'NONE',  ( 84.99999999999998579, 95.00000000000000000, 14.99999999999999467 ) ) ;
#6149 = CARTESIAN_POINT ( 'NONE',  ( 192.8300434168937727, 49.99999999883907975, 13.43548448457828037 ) ) ;
#6150 = CARTESIAN_POINT ( 'NONE',  ( 139.2950502721270425, 38.66835937608393436, 9.295050272127046043 ) ) ;
#6151 = CARTESIAN_POINT ( 'NONE',  ( 9.295050272127047819, 37.87460937608393863, 9.295050272127046043 ) ) ;
#6152 = VECTOR ( 'NONE', #18596, 1000.000000000000000 ) ;
#6153 = ORIENTED_EDGE ( 'NONE', *, *, #21226, .T. ) ;
#6154 = CARTESIAN_POINT ( 'NONE',  ( 51.42518405393695957, 38.56914062500000284, -5.622872871577873077 ) ) ;
#6155 = CYLINDRICAL_SURFACE ( 'NONE', #494, 13.57481594606304398 ) ;
#6156 = CARTESIAN_POINT ( 'NONE',  ( 207.0095733385116716, 36.00000000000000711, 5.901833544881684546 ) ) ;
#6157 = CARTESIAN_POINT ( 'NONE',  ( 96.84719886470459471, -3.152801135295355994, 3.562500001365591196 ) ) ;
#6158 = CARTESIAN_POINT ( 'NONE',  ( 91.91746824999998466, 112.6261737610028320, -53.22500000273119269 ) ) ;
#6159 = CARTESIAN_POINT ( 'NONE',  ( 101.8468681455907046, -4.458734124999987891, 2.000000001365591640 ) ) ;
#6160 = ADVANCED_FACE ( 'NONE', ( #11212 ), #13347, .F. ) ;
#6161 = CARTESIAN_POINT ( 'NONE',  ( 103.1528011352953342, 80.06250000136559208, 3.152801135295355106 ) ) ;
#6162 = CARTESIAN_POINT ( 'NONE',  ( -13.14518615778179189, 32.66562500108393863, 5.444914386472304635 ) ) ;
#6163 = CARTESIAN_POINT ( 'NONE',  ( 2.414731522848535132E-15, 40.15664062608393436, 13.14518615778179544 ) ) ;
#6164 = CARTESIAN_POINT ( 'NONE',  ( 108.0825317499999869, 112.6261737610028320, -48.77499999726882152 ) ) ;
#6165 = ORIENTED_EDGE ( 'NONE', *, *, #22907, .T. ) ;
#6166 = EDGE_CURVE ( 'NONE', #861, #18432, #24833, .T. ) ;
#6167 = CARTESIAN_POINT ( 'NONE',  ( 97.93301270000000613, 124.5500000010924850, -9.540979117872439019E-15 ) ) ;
#6168 = DIRECTION ( 'NONE',  ( -0.000000000000000000, 1.000000000000000000, -0.000000000000000000 ) ) ;
#6169 = CARTESIAN_POINT ( 'NONE',  ( 94.99999999999995737, 81.06250000273119838, -2.071067811865491048 ) ) ;
#6170 = CARTESIAN_POINT ( 'NONE',  ( 91.91746824999997045, 107.3738262389971538, -55.77499999726882862 ) ) ;
#6171 = VECTOR ( 'NONE', #1531, 1000.000000000000000 ) ;
#6172 = DIRECTION ( 'NONE',  ( 1.000000000000000000, 0.000000000000000000, 0.000000000000000000 ) ) ;
#6173 = VERTEX_POINT ( 'NONE', #10932 ) ;
#6174 = CARTESIAN_POINT ( 'NONE',  ( 70.44491438647229131, 37.82500000108392868, 13.14518615778179189 ) ) ;
#6175 = EDGE_CURVE ( 'NONE', #5976, #444, #2414, .T. ) ;
#6176 = CARTESIAN_POINT ( 'NONE',  ( -13.57481594606304753, 39.36289062499999858, -5.622872871577872189 ) ) ;
#6177 = ORIENTED_EDGE ( 'NONE', *, *, #17078, .F. ) ;
#6178 = CARTESIAN_POINT ( 'NONE',  ( 94.33688103937537051, 105.8855032339526758, -51.80000000000000426 ) ) ;
#6179 = CARTESIAN_POINT ( 'NONE',  ( -3.044609456930747804, 53.89089363584124470, -15.00000000000000000 ) ) ;
#6180 = VECTOR ( 'NONE', #3997, 1000.000000000000000 ) ;
#6181 = CARTESIAN_POINT ( 'NONE',  ( 101.4615807364564546, 124.4500000010924765, -1.461580736456474794 ) ) ;
#6182 = CARTESIAN_POINT ( 'NONE',  ( 124.3771271284221314, 33.80664062716786589, -13.57481594606304753 ) ) ;
#6183 = CARTESIAN_POINT ( 'NONE',  ( 181.4251840539369596, 40.95039062499999005, -5.622872871577872189 ) ) ;
#6184 = FACE_OUTER_BOUND ( 'NONE', #15691, .T. ) ;
#6185 = CARTESIAN_POINT ( 'NONE',  ( 181.8548138422181921, 35.24531250108393721, 5.444914386472304635 ) ) ;
#6186 = ORIENTED_EDGE ( 'NONE', *, *, #9831, .F. ) ;
#6187 =( BOUNDED_CURVE ( )  B_SPLINE_CURVE ( 2, ( #22182, #1341, #27414, #11323, #25126, #7877, #523, #3613, #5613 ),
 .UNSPECIFIED., .F., .F. ) 
 B_SPLINE_CURVE_WITH_KNOTS ( ( 3, 2, 2, 2, 3 ),
 ( 0.1041666666666664909, 0.1145833333333332732, 0.1250000000000000833, 0.1354166666666668517, 0.1458333333333336757 ),
 .UNSPECIFIED. ) 
 CURVE ( )  GEOMETRIC_REPRESENTATION_ITEM ( )  RATIONAL_B_SPLINE_CURVE ( ( 1.000000000000001332, 0.9238795325112854062, 1.000000000000000000, 0.9238795325112867385, 1.000000000000000000, 0.9238795325112867385, 1.000000000000000000, 0.9238795325112842960, 1.000000000000002442 ) ) 
 REPRESENTATION_ITEM ( '' )  );
#6188 = ORIENTED_EDGE ( 'NONE', *, *, #19611, .F. ) ;
#6189 = VERTEX_POINT ( 'NONE', #17929 ) ;
#6190 = CARTESIAN_POINT ( 'NONE',  ( 9.295050272127046043, 32.31835937608393294, -9.295050272127046043 ) ) ;
#6191 = DIRECTION ( 'NONE',  ( -1.003171929053526103E-16, -0.5735764363510443831, -0.8191520442889929088 ) ) ;
#6192 = EDGE_CURVE ( 'NONE', #24599, #11583, #5289, .T. ) ;
#6193 = CARTESIAN_POINT ( 'NONE',  ( 96.46446609406726225, 92.24999999726880162, -3.535533905932738197 ) ) ;
#6194 = CARTESIAN_POINT ( 'NONE',  ( 105.6631189606246295, 105.8855032339526758, -51.70000000546237828 ) ) ;
#6195 = CARTESIAN_POINT ( 'NONE',  ( 104.9999999999999716, 1.449011120738813565E-14, 14.49999999999999822 ) ) ;
#6196 = CARTESIAN_POINT ( 'NONE',  ( -9.295050272127046043, 40.65273437608393436, -9.295050272127046043 ) ) ;
#6197 = DIRECTION ( 'NONE',  ( -0.000000000000000000, -1.000000000000000000, -0.000000000000000000 ) ) ;
#6198 = CARTESIAN_POINT ( 'NONE',  ( 99.99999999999998579, 93.75000000000000000, 4.999999999999984013 ) ) ;
#6199 = CARTESIAN_POINT ( 'NONE',  ( 195.0000000000000000, 40.15664062608393436, 13.14518615778179544 ) ) ;
#6200 = CARTESIAN_POINT ( 'NONE',  ( 91.91746824999997045, 107.3738262389971538, -47.52499999726881441 ) ) ;
#6201 = EDGE_CURVE ( 'NONE', #499, #21009, #7037, .T. ) ;
#6202 = EDGE_LOOP ( 'NONE', ( #23639, #1547, #23288 ) ) ;
#6203 = CARTESIAN_POINT ( 'NONE',  ( -13.14518615778179900, 31.97109375108393436, -5.444914386472297529 ) ) ;
#6204 = CARTESIAN_POINT ( 'NONE',  ( 2.493653234604083739E-15, 31.77265625216787370, 13.57481594606304576 ) ) ;
#6205 = CARTESIAN_POINT ( 'NONE',  ( 96.46446609406721961, 3.535533905932755072, 2.000000002731185056 ) ) ;
#6206 = CARTESIAN_POINT ( 'NONE',  ( 116.8548138422182063, 36.03906250108394005, 5.444914386472304635 ) ) ;
#6207 = CARTESIAN_POINT ( 'NONE',  ( 78.14518615778179367, 37.03125000108393294, -5.444914386472297529 ) ) ;
#6208 = ADVANCED_FACE ( 'NONE', ( #13203 ), #26199, .T. ) ;
#6209 = CARTESIAN_POINT ( 'NONE',  ( 189.5550856135277229, 32.76484375108393010, 13.14518615778179722 ) ) ;
#6210 = CARTESIAN_POINT ( 'NONE',  ( 52.16024876314180858, 35.99999999999999289, 2.850296047819762091 ) ) ;
#6211 = CARTESIAN_POINT ( 'NONE',  ( -13.14518615778179189, 36.63437500108393152, 5.444914386472304635 ) ) ;
#6212 = CARTESIAN_POINT ( 'NONE',  ( 99.99999999999995737, 1.387778780781445676E-14, 34.79898987322334136 ) ) ;
#6213 = CIRCLE ( 'NONE', #11648, 5.000000000000004441 ) ;
#6214 = CARTESIAN_POINT ( 'NONE',  ( 192.7020394139928499, 35.99999999999997868, 12.97104423350699420 ) ) ;
#6215 = DIRECTION ( 'NONE',  ( 0.000000000000000000, 0.000000000000000000, -1.000000000000000000 ) ) ;
#6216 = CARTESIAN_POINT ( 'NONE',  ( 13.14518615778179900, 37.82500000108392868, -5.444914386472297529 ) ) ;
#6217 = CIRCLE ( 'NONE', #307, 2.500000000000008882 ) ;
#6218 = CARTESIAN_POINT ( 'NONE',  ( 98.96446609406726225, 124.0499999999999829, -2.499999999999998668 ) ) ;
#6219 = CARTESIAN_POINT ( 'NONE',  ( 98.96446609406727646, 124.3499999999999943, 2.499999999999977796 ) ) ;
#6220 = CARTESIAN_POINT ( 'NONE',  ( 101.4615807364564546, 124.2500000010924737, 1.461580736456455476 ) ) ;
#6221 = CARTESIAN_POINT ( 'NONE',  ( 99.14382582708708469, 124.6000000010924822, -2.066987299999998751 ) ) ;
#6222 = EDGE_LOOP ( 'NONE', ( #28079, #2253, #4495, #177 ) ) ;
#6223 = CARTESIAN_POINT ( 'NONE',  ( 95.54126587499995082, -1.846868145590724986, 9.500000001365593860 ) ) ;
#6224 = CARTESIAN_POINT ( 'NONE',  ( -13.57481594606304576, 32.36796875216787583, 0.000000000000000000 ) ) ;
#6225 = ORIENTED_EDGE ( 'NONE', *, *, #5776, .F. ) ;
#6226 = CARTESIAN_POINT ( 'NONE',  ( 97.50000000000000000, 124.2500000021849758, -1.035533905932742416 ) ) ;
#6227 = CARTESIAN_POINT ( 'NONE',  ( 104.4587341249999781, 1.846868145590750299, 12.00000000136559208 ) ) ;
#6228 = CARTESIAN_POINT ( 'NONE',  ( -13.14518615778179189, 33.45937500108393436, 5.444914386472304635 ) ) ;
#6229 = CARTESIAN_POINT ( 'NONE',  ( -9.295050272127044266, 39.06523437608392868, 9.295050272127047819 ) ) ;
#6230 = DIRECTION ( 'NONE',  ( 1.000000000000000000, 0.000000000000000000, -0.000000000000000000 ) ) ;
#6231 = CARTESIAN_POINT ( 'NONE',  ( 104.4587341249999639, 84.18750000136560629, -1.442382525525748735E-14 ) ) ;
#6232 = CARTESIAN_POINT ( 'NONE',  ( 70.44491438647230552, 37.82500000108392868, 13.14518615778179189 ) ) ;
#6233 = CARTESIAN_POINT ( 'NONE',  ( 91.91746824999999887, 110.0000000000000000, -45.37500000273119838 ) ) ;
#6234 = CARTESIAN_POINT ( 'NONE',  ( 94.99999999999995737, 1.387778780781445676E-14, 6.125000002731185056 ) ) ;
#6235 = VECTOR ( 'NONE', #19825, 1000.000000000000000 ) ;
#6236 = CARTESIAN_POINT ( 'NONE',  ( 0.000000000000000000, 52.00000000000000711, 0.000000000000000000 ) ) ;
#6237 = CARTESIAN_POINT ( 'NONE',  ( 99.99999999999997158, 117.3602355696678501, -54.99999999453763166 ) ) ;
#6238 = CARTESIAN_POINT ( 'NONE',  ( 116.4251840539369454, 40.15664062500000142, -5.622872871577873077 ) ) ;
#6239 = EDGE_CURVE ( 'NONE', #26226, #4887, #26493, .T. ) ;
#6240 = ORIENTED_EDGE ( 'NONE', *, *, #8435, .T. ) ;
#6241 = CARTESIAN_POINT ( 'NONE',  ( 107.0000000000000000, 107.7255621263696668, -55.59999999453764019 ) ) ;
#6242 = CARTESIAN_POINT ( 'NONE',  ( -13.57481594606304576, 39.56132812716787583, 5.622872871577880183 ) ) ;
#6243 = CARTESIAN_POINT ( 'NONE',  ( 120.7049497278729575, 37.47773437608393010, 9.295050272127047819 ) ) ;
#6244 = CARTESIAN_POINT ( 'NONE',  ( 65.00000000000000000, 37.32890625216786873, 13.57481594606304576 ) ) ;
#6245 = CARTESIAN_POINT ( 'NONE',  ( 91.91746824999997045, 112.6261737610028320, -51.72499999726882436 ) ) ;
#6246 = CARTESIAN_POINT ( 'NONE',  ( 5.622872871577878406, 34.20351562716788862, 13.57481594606304576 ) ) ;
#6247 = CARTESIAN_POINT ( 'NONE',  ( 94.99999999999995737, -2.071067811865466624, 5.062500000000000888 ) ) ;
#6248 = CARTESIAN_POINT ( 'NONE',  ( 189.5550856135277229, 37.52734375108393294, 13.14518615778179722 ) ) ;
#6249 = VECTOR ( 'NONE', #22171, 1000.000000000000000 ) ;
#6250 = DIRECTION ( 'NONE',  ( 1.000000000000000000, 0.000000000000000000, -7.228014483236696740E-18 ) ) ;
#6251 = CARTESIAN_POINT ( 'NONE',  ( 130.0000000000000000, 39.56132812608393579, -13.14518615778179544 ) ) ;
#6252 = DIRECTION ( 'NONE',  ( 0.000000000000000000, 0.000000000000000000, 1.000000000000000000 ) ) ;
#6253 = CARTESIAN_POINT ( 'NONE',  ( 94.99999999999997158, 2.071067811865471953, 5.062500002731186832 ) ) ;
#6254 = LINE ( 'NONE', #10233, #16039 ) ;
#6255 = CARTESIAN_POINT ( 'NONE',  ( 59.37712712842228058, 36.88242187499999858, -13.57481594606318254 ) ) ;
#6256 = CARTESIAN_POINT ( 'NONE',  ( 5.444914386472302859, 39.21406250108392300, 13.14518615778179189 ) ) ;
#6257 = CARTESIAN_POINT ( 'NONE',  ( 204.5988444088204687, 36.53515624999999289, 9.598844408820456309 ) ) ;
#6258 = DIRECTION ( 'NONE',  ( -0.000000000000000000, -1.000000000000000000, -0.000000000000000000 ) ) ;
#6259 = CARTESIAN_POINT ( 'NONE',  ( 98.15313185440925281, 4.458734125000016313, 4.500000001365592084 ) ) ;
#6260 = CARTESIAN_POINT ( 'NONE',  ( 78.14518615778179367, 40.10703125108393152, 5.444914386472293977 ) ) ;
#6261 = CARTESIAN_POINT ( 'NONE',  ( 99.99999999999995737, 4.458734125000016313, 6.187500001365592084 ) ) ;
#6262 = LINE ( 'NONE', #10800, #10455 ) ;
#6263 = CARTESIAN_POINT ( 'NONE',  ( 95.54126587500000767, 94.81249999863440792, -7.484931351350258973E-15 ) ) ;
#6264 = CARTESIAN_POINT ( 'NONE',  ( -12.99948823019059319, 35.99999999999999289, 1.999176114741941346 ) ) ;
#6265 = CARTESIAN_POINT ( 'NONE',  ( -9.598844408820458085, 38.51953124999999289, -9.598844408820458085 ) ) ;
#6266 = FACE_OUTER_BOUND ( 'NONE', #8026, .T. ) ;
#6267 = VERTEX_POINT ( 'NONE', #2273 ) ;
#6268 = CARTESIAN_POINT ( 'NONE',  ( 104.4587341249999781, 80.25000000136559208, -1.846868145590750299 ) ) ;
#6269 = CARTESIAN_POINT ( 'NONE',  ( 65.00000000000000000, -7.395377635281828788, -7.517135062566165128E-15 ) ) ;
#6270 = EDGE_LOOP ( 'NONE', ( #19724, #4189, #14182, #23384 ) ) ;
#6271 = CARTESIAN_POINT ( 'NONE',  ( 214.9999999999999716, 50.00000000000000000, 14.99999999999994316 ) ) ;
#6272 = CARTESIAN_POINT ( 'NONE',  ( 74.29505027212704249, 34.10429687608393579, -9.295050272127046043 ) ) ;
#6273 = EDGE_LOOP ( 'NONE', ( #14539, #1807, #13451, #20733 ) ) ;
#6274 = DIRECTION ( 'NONE',  ( 0.000000000000000000, 0.000000000000000000, -1.000000000000000000 ) ) ;
#6275 = CARTESIAN_POINT ( 'NONE',  ( 103.1528011352953342, 3.152801135295383084, 1.312500001365592750 ) ) ;
#6276 = EDGE_CURVE ( 'NONE', #25525, #20971, #22153, .T. ) ;
#6277 = VERTEX_POINT ( 'NONE', #26927 ) ;
#6278 = CARTESIAN_POINT ( 'NONE',  ( 9.295050272127046043, 34.89804687608393863, -9.295050272127046043 ) ) ;
#6279 = CARTESIAN_POINT ( 'NONE',  ( 5.444914386472297529, 38.12265625108393152, -13.14518615778179900 ) ) ;
#6280 = CARTESIAN_POINT ( 'NONE',  ( 200.6228728715778686, 37.37851562716787157, 13.57481594606304576 ) ) ;
#6281 = CARTESIAN_POINT ( 'NONE',  ( 5.444914386472302859, 35.24531250108393010, 13.14518615778179189 ) ) ;
#6282 = FACE_BOUND ( 'NONE', #20105, .T. ) ;
#6283 = DIRECTION ( 'NONE',  ( -1.000000000000000000, -0.000000000000000000, -0.000000000000000000 ) ) ;
#6284 = CARTESIAN_POINT ( 'NONE',  ( 139.2950502721270425, 39.66054687608393436, -9.295050272127046043 ) ) ;
#6285 = CARTESIAN_POINT ( 'NONE',  ( -8.049105076161786076E-16, 39.75976562608394005, -13.14518615778179544 ) ) ;
#6286 = CARTESIAN_POINT ( 'NONE',  ( 139.2950502721270425, 33.70742187608393436, 9.295050272127046043 ) ) ;
#6287 = CARTESIAN_POINT ( 'NONE',  ( 78.57481594606304043, 37.47773437500001137, -5.622872871577873077 ) ) ;
#6288 = CARTESIAN_POINT ( 'NONE',  ( 94.99999999999995737, 2.071067811865500818, 9.937499999999996447 ) ) ;
#6289 = VECTOR ( 'NONE', #13039, 1000.000000000000000 ) ;
#6290 = CARTESIAN_POINT ( 'NONE',  ( 103.1528011352953342, -3.152801135295355106, 0.8125000013655924169 ) ) ;
#6291 = CARTESIAN_POINT ( 'NONE',  ( 93.00000000000000000, 110.0000000000000000, -46.00000000000000711 ) ) ;
#6292 = CARTESIAN_POINT ( 'NONE',  ( 99.99999999999995737, 4.458734125000016313, 2.187500001365592084 ) ) ;
#6293 = CARTESIAN_POINT ( 'NONE',  ( 108.0825317500000011, 107.3738262389971538, -52.22500000273118559 ) ) ;
#6294 = AXIS2_PLACEMENT_3D ( 'NONE', #4477, #16252, #14104 ) ;
#6295 = CYLINDRICAL_SURFACE ( 'NONE', #19420, 15.57481594606304576 ) ;
#6296 = CARTESIAN_POINT ( 'NONE',  ( 13.14518615778179900, 32.96328125108393436, 5.444914386472293977 ) ) ;
#6297 = CARTESIAN_POINT ( 'NONE',  ( 5.444914386472297529, 38.12265625108393152, -13.14518615778179900 ) ) ;
#6298 = CARTESIAN_POINT ( 'NONE',  ( 102.4976396683250783, 117.6869444889999841, -50.47499999726882436 ) ) ;
#6299 = EDGE_LOOP ( 'NONE', ( #5203, #14768, #7767, #13424 ) ) ;
#6300 = CARTESIAN_POINT ( 'NONE',  ( -9.295050272127044266, 32.11992187608393579, 9.295050272127047819 ) ) ;
#6301 =( BOUNDED_CURVE ( )  B_SPLINE_CURVE ( 2, ( #10557, #8708, #27966, #8284, #19545 ),
 .UNSPECIFIED., .F., .F. ) 
 B_SPLINE_CURVE_WITH_KNOTS ( ( 3, 2, 3 ),
 ( 0.000000000000000000, 0.02500000000000002220, 0.05000000000000004441 ),
 .UNSPECIFIED. ) 
 CURVE ( )  GEOMETRIC_REPRESENTATION_ITEM ( )  RATIONAL_B_SPLINE_CURVE ( ( 1.000000000000000000, 0.9238795325112867385, 1.000000000000000000, 0.9238795325112866275, 1.000000000000000222 ) ) 
 REPRESENTATION_ITEM ( '' )  );
#6302 = LINE ( 'NONE', #21562, #4789 ) ;
#6303 = CARTESIAN_POINT ( 'NONE',  ( 101.1344650075701566, 123.0000000000000426, 2.161518037331323416 ) ) ;
#6304 = CARTESIAN_POINT ( 'NONE',  ( 189.3771271284220745, 36.38632812499999858, 13.57481594606300135 ) ) ;
#6305 = CARTESIAN_POINT ( 'NONE',  ( 103.5355339059327093, 84.62500000000000000, -3.535533905932755072 ) ) ;
#6306 = CARTESIAN_POINT ( 'NONE',  ( 200.4449143864723055, 39.51171875108392584, -13.14518615778179900 ) ) ;
#6307 = ORIENTED_EDGE ( 'NONE', *, *, #12599, .T. ) ;
#6308 = CARTESIAN_POINT ( 'NONE',  ( 0.000000000000000000, 40.99999999999999289, 0.000000000000000000 ) ) ;
#6309 = CARTESIAN_POINT ( 'NONE',  ( 92.99999999999998579, 110.0000000000000000, -55.00000000000002132 ) ) ;
#6310 = VECTOR ( 'NONE', #14314, 1000.000000000000000 ) ;
#6311 = CYLINDRICAL_SURFACE ( 'NONE', #20320, 13.57481594606304576 ) ;
#6312 = ORIENTED_EDGE ( 'NONE', *, *, #1361, .T. ) ;
#6313 = CARTESIAN_POINT ( 'NONE',  ( 97.83688103937537051, 103.3426043859339103, -49.60000000000000853 ) ) ;
#6314 = CARTESIAN_POINT ( 'NONE',  ( -8.201446187645640151, 50.69246985422426377, -15.00000000000000000 ) ) ;
#6315 = AXIS2_PLACEMENT_3D ( 'NONE', #13054, #6661, #12916 ) ;
#6316 = CARTESIAN_POINT ( 'NONE',  ( 130.0000000000000000, 34.15390625216787157, 13.57481594606304576 ) ) ;
#6317 = CARTESIAN_POINT ( 'NONE',  ( 55.70494972787295751, 40.05742187608393579, 9.295050272127047819 ) ) ;
#6318 = CARTESIAN_POINT ( 'NONE',  ( -8.312177448680279460E-16, 35.34453125216787583, -13.57481594606304576 ) ) ;
#6319 = CARTESIAN_POINT ( 'NONE',  ( 208.1451861577818079, 34.79882812608394005, -1.609821015232357215E-15 ) ) ;
#6320 = VERTEX_POINT ( 'NONE', #7941 ) ;
#6321 = EDGE_LOOP ( 'NONE', ( #8543, #3591, #244, #10437 ) ) ;
#6322 = ORIENTED_EDGE ( 'NONE', *, *, #23377, .T. ) ;
#6323 = CARTESIAN_POINT ( 'NONE',  ( -13.14518615778179189, 39.21406250108392300, 5.444914386472304635 ) ) ;
#6324 = CARTESIAN_POINT ( 'NONE',  ( 101.8468681455907046, 4.458734125000016313, 14.37500000136559386 ) ) ;
#6325 = CARTESIAN_POINT ( 'NONE',  ( 102.4999999999999858, 124.6000000000000085, -9.847140817659276890E-15 ) ) ;
#6326 = CARTESIAN_POINT ( 'NONE',  ( 103.1528011352953342, 81.81250000136559208, 3.152801135295355106 ) ) ;
#6327 = CARTESIAN_POINT ( 'NONE',  ( 189.5550856135277229, 37.52734375108393294, 13.14518615778179722 ) ) ;
#6328 = CARTESIAN_POINT ( 'NONE',  ( -13.14518615778179722, 39.90859375108393436, -5.444914386472297529 ) ) ;
#6329 = CYLINDRICAL_SURFACE ( 'NONE', #5479, 5.000000000000004441 ) ;
#6330 =( GEOMETRIC_REPRESENTATION_CONTEXT ( 3 ) GLOBAL_UNCERTAINTY_ASSIGNED_CONTEXT ( ( #7784 ) ) GLOBAL_UNIT_ASSIGNED_CONTEXT ( ( #5640, #12024, #27441 ) ) REPRESENTATION_CONTEXT ( 'NONE', 'WORKASPACE' ) );
#6331 = AXIS2_PLACEMENT_3D ( 'NONE', #26109, #11264, #15692 ) ;
#6332 = CARTESIAN_POINT ( 'NONE',  ( 95.67376207875072680, 104.0454443415356991, -49.70000000000000995 ) ) ;
#6333 = CARTESIAN_POINT ( 'NONE',  ( 104.9952793366501709, 116.8754121666685393, -48.32499999726881867 ) ) ;
#6334 = ORIENTED_EDGE ( 'NONE', *, *, #23255, .T. ) ;
#6335 = EDGE_CURVE ( 'NONE', #20101, #7889, #20784, .T. ) ;
#6336 = CARTESIAN_POINT ( 'NONE',  ( 2.493653234604083739E-15, 36.43593749999999432, 13.57481594606304576 ) ) ;
#6337 = CARTESIAN_POINT ( 'NONE',  ( 5.444914386472297529, 36.33671875108394289, -13.14518615778179900 ) ) ;
#6338 = CARTESIAN_POINT ( 'NONE',  ( 96.46446609406721961, -3.535533905932727539, 0.2500000027311852779 ) ) ;
#6339 = CARTESIAN_POINT ( 'NONE',  ( 120.7049497278729575, 35.29492187608393294, 9.295050272127047819 ) ) ;
#6340 = CARTESIAN_POINT ( 'NONE',  ( 65.00000000000000000, 33.21132812608393436, -13.14518615778179544 ) ) ;
#6341 = CARTESIAN_POINT ( 'NONE',  ( 181.8548138422182205, 37.57695312608393579, 0.000000000000000000 ) ) ;
#6342 = CARTESIAN_POINT ( 'NONE',  ( 195.0000000000000000, 37.22968749999999716, 13.57481594606304576 ) ) ;
#6343 = CARTESIAN_POINT ( 'NONE',  ( -5.444914386472299306, 35.93984375108392726, 13.14518615778179722 ) ) ;
#6344 = EDGE_CURVE ( 'NONE', #7430, #8989, #9961, .T. ) ;
#6345 = CARTESIAN_POINT ( 'NONE',  ( -9.598844408820458085, 38.61875000216787157, -9.598844408820458085 ) ) ;
#6346 = CARTESIAN_POINT ( 'NONE',  ( 219.9999999999999716, 75.00000000000000000, 9.999999999999946709 ) ) ;
#6347 = EDGE_CURVE ( 'NONE', #17326, #14317, #1265, .T. ) ;
#6348 =( BOUNDED_CURVE ( )  B_SPLINE_CURVE ( 2, ( #19304, #8607, #6196, #10307, #3644, #12725, #12307, #2063, #27727, #8188, #1513, #8467, #1928, #10596, #25577, #28003, #28140, #6328, #15003, #10167, #27586, #6061, #8046, #16743, #25442, #2208, #24145, #17438, #6745, #4338, #17579, #636, #12994, #6603, #15720, #25997, #65, #2632, #20156, #11146, #24423, #26285, #21734, #11436, #7024, #2772, #2351, #9036, #15287, #2486, #17728, #26137, #6890, #9310, #26431, #11007, #4622, #23860, #15576, #6468, #8747, #19862, #11292, #15430, #20014, #13279, #4482, #24283, #22009, #15142, #349, #19719, #13573, #24005, #17869, #10871, #13138, #4911, #22296, #4764, #19582, #21875, #204, #8889, #13425, #26573, #22151, #9176, #495, #14000, #12000, #18444, #1209, #26717, #24995, #5334, #5616, #20725, #16292, #7743, #22863, #16431, #1067, #18150, #22580, #3190, #5474, #2905, #7311, #13716, #9875, #3330, #7452, #16146, #5191, #1344, #779, #9451, #20442, #18581, #14282, #13855, #3049, #9594, #14144, #15860, #5050, #27285, #20862, #24854, #25129, #22724, #18297, #26864, #27005, #23000, #3470, #15998, #27151, #7603, #11861, #12137, #11717, #18007, #7164, #20583, #9736, #24714, #924, #24569, #22437, #11574, #20294, #8161, #10425, #3616, #25265, #17123, #6031, #10568, #18850, #16573, #21561, #25552, #19277, #25826, #27558, #16853, #1621, #3889, #8016, #12834, #18719, #14977, #6300, #23696, #3754, #18988, #14695, #12275, #7880, #21277, #10008 ),
 .UNSPECIFIED., .F., .F. ) 
 B_SPLINE_CURVE_WITH_KNOTS ( ( 3, 2, 2, 2, 2, 2, 2, 2, 2, 2, 2, 2, 2, 2, 2, 2, 2, 2, 2, 2, 2, 2, 2, 2, 2, 2, 2, 2, 2, 2, 2, 2, 2, 2, 2, 2, 2, 2, 2, 2, 2, 2, 2, 2, 2, 2, 2, 2, 2, 2, 2, 2, 2, 2, 2, 2, 2, 2, 2, 2, 2, 2, 2, 2, 2, 2, 2, 2, 2, 2, 2, 2, 2, 2, 2, 2, 2, 2, 2, 2, 2, 2, 2, 2, 2, 2, 2, 2, 2, 2, 2, 3 ),
 ( 0.000000000000000000, 0.01041666666666666609, 0.02083333333333333218, 0.03125000000000000000, 0.04166666666666666435, 0.05208333333333333565, 0.06250000000000000000, 0.07291666666666667129, 0.08333333333333332871, 0.09375000000000000000, 0.1041666666666666713, 0.1145833333333333287, 0.1250000000000000000, 0.1354166666666666574, 0.1458333333333333426, 0.1562499999999999722, 0.1666666666666666574, 0.1770833333333333426, 0.1875000000000000000, 0.1979166666666666574, 0.2083333333333333426, 0.2187500000000000278, 0.2291666666666666574, 0.2395833333333333426, 0.2500000000000000000, 0.2604166666666666852, 0.2708333333333333148, 0.2812500000000000000, 0.2916666666666666852, 0.3020833333333333148, 0.3124999999999999445, 0.3229166666666666852, 0.3333333333333333148, 0.3437500000000000000, 0.3541666666666666852, 0.3645833333333333148, 0.3750000000000000000, 0.3854166666666666852, 0.3958333333333333148, 0.4062500000000000000, 0.4166666666666666852, 0.4270833333333333148, 0.4375000000000000555, 0.4479166666666666852, 0.4583333333333333148, 0.4687500000000000000, 0.4791666666666666852, 0.4895833333333333148, 0.5000000000000000000, 0.5104166666666666297, 0.5208333333333333703, 0.5312500000000000000, 0.5416666666666666297, 0.5520833333333333703, 0.5625000000000000000, 0.5729166666666666297, 0.5833333333333333703, 0.5937500000000000000, 0.6041666666666666297, 0.6145833333333333703, 0.6249999999999998890, 0.6354166666666666297, 0.6458333333333333703, 0.6562500000000000000, 0.6666666666666666297, 0.6770833333333333703, 0.6875000000000000000, 0.6979166666666666297, 0.7083333333333333703, 0.7187500000000000000, 0.7291666666666666297, 0.7395833333333333703, 0.7500000000000000000, 0.7604166666666666297, 0.7708333333333333703, 0.7812500000000000000, 0.7916666666666666297, 0.8020833333333333703, 0.8125000000000000000, 0.8229166666666666297, 0.8333333333333333703, 0.8437500000000000000, 0.8541666666666666297, 0.8645833333333333703, 0.8750000000000001110, 0.8854166666666666297, 0.8958333333333333703, 0.9062500000000000000, 0.9166666666666666297, 0.9270833333333333703, 0.9375000000000000000, 0.9448587001587775980 ),
 .UNSPECIFIED. ) 
 CURVE ( )  GEOMETRIC_REPRESENTATION_ITEM ( )  RATIONAL_B_SPLINE_CURVE ( ( 1.000000000000000000, 0.9238795325112867385, 1.000000000000000000, 0.9238795325112867385, 1.000000000000000000, 0.9238795325112867385, 1.000000000000000000, 0.9238795325112867385, 1.000000000000000000, 0.9238795325112867385, 1.000000000000000000, 0.9238795325112867385, 1.000000000000000000, 0.9238795325112867385, 1.000000000000000000, 0.9238795325112867385, 1.000000000000000000, 0.9238795325112867385, 1.000000000000000000, 0.9238795325112867385, 1.000000000000000000, 0.9238795325112867385, 1.000000000000000000, 0.9238795325112867385, 1.000000000000000000, 0.9238795325112867385, 1.000000000000000000, 0.9238795325112867385, 1.000000000000000000, 0.9238795325112867385, 1.000000000000000000, 0.9238795325112867385, 1.000000000000000000, 0.9238795325112867385, 1.000000000000000000, 0.9238795325112867385, 1.000000000000000000, 0.9238795325112867385, 1.000000000000000000, 0.9238795325112867385, 1.000000000000000000, 0.9238795325112867385, 1.000000000000000000, 0.9238795325112867385, 1.000000000000000000, 0.9238795325112867385, 1.000000000000000000, 0.9238795325112867385, 1.000000000000000000, 0.9238795325112867385, 1.000000000000000000, 0.9238795325112867385, 1.000000000000000000, 0.9238795325112867385, 1.000000000000000000, 0.9238795325112867385, 1.000000000000000000, 0.9238795325112867385, 1.000000000000000000, 0.9238795325112867385, 1.000000000000000000, 0.9238795325112867385, 1.000000000000000000, 0.9238795325112867385, 1.000000000000000000, 0.9238795325112867385, 1.000000000000000000, 0.9238795325112867385, 1.000000000000000000, 0.9238795325112867385, 1.000000000000000000, 0.9238795325112867385, 1.000000000000000000, 0.9238795325112867385, 1.000000000000000000, 0.9238795325112867385, 1.000000000000000000, 0.9238795325112867385, 1.000000000000000000, 0.9238795325112867385, 1.000000000000000000, 0.9238795325112867385, 1.000000000000000000, 0.9238795325112867385, 1.000000000000000000, 0.9238795325112867385, 1.000000000000000000, 0.9238795325112867385, 1.000000000000000000, 0.9238795325112867385, 1.000000000000000000, 0.9238795325112867385, 1.000000000000000000, 0.9238795325112867385, 1.000000000000000000, 0.9238795325112867385, 1.000000000000000000, 0.9238795325112867385, 1.000000000000000000, 0.9238795325112867385, 1.000000000000000000, 0.9238795325112867385, 1.000000000000000000, 0.9238795325112867385, 1.000000000000000000, 0.9238795325112867385, 1.000000000000000000, 0.9238795325112867385, 1.000000000000000000, 0.9238795325112867385, 1.000000000000000000, 0.9238795325112867385, 1.000000000000000000, 0.9238795325112867385, 1.000000000000000000, 0.9238795325112867385, 1.000000000000000000, 0.9238795325112867385, 1.000000000000000000, 0.9238795325112867385, 1.000000000000000000, 0.9238795325112867385, 1.000000000000000000, 0.9238795325112867385, 1.000000000000000000, 0.9238795325112867385, 1.000000000000000000, 0.9238795325112867385, 1.000000000000000000, 0.9238795325112867385, 1.000000000000000000, 0.9238795325112867385, 1.000000000000000000, 0.9238795325112867385, 1.000000000000000000, 0.9238795325112867385, 1.000000000000000000, 0.9238795325112867385, 1.000000000000000000, 0.9238795325112867385, 1.000000000000000000, 0.9238795325112867385, 1.000000000000000000, 0.9238795325112867385, 1.000000000000000000, 0.9238795325112867385, 1.000000000000000000, 0.9238795325112867385, 1.000000000000000000, 0.9238795325112867385, 1.000000000000000000, 0.9238795325112867385, 1.000000000000000000, 0.9238795325112867385, 1.000000000000000000, 0.9238795325112867385, 1.000000000000000000, 0.9238795325112867385, 1.000000000000000000, 0.9238795325112867385, 1.000000000000000000, 0.9238795325112867385, 1.000000000000000000, 0.9238795325112867385, 1.000000000000000000, 0.9238795325112867385, 1.000000000000000000, 0.9238795325112867385, 1.000000000000000000, 0.9238795325112867385, 1.000000000000000000, 0.9238795325112867385, 1.000000000000000000, 0.9238795325112867385, 1.000000000000000000, 0.9238795325112867385, 1.000000000000000000, 0.9238795325112867385, 1.000000000000000000, 0.9238795325112867385, 1.000000000000000000, 0.9462258211652395667, 0.9684275895297407288 ) ) 
 REPRESENTATION_ITEM ( '' )  );
#6349 = CARTESIAN_POINT ( 'NONE',  ( -5.444914386472299306, 39.90859375108393436, 13.14518615778179722 ) ) ;
#6350 = CARTESIAN_POINT ( 'NONE',  ( 94.99999999999995737, 2.071067811865491493, 10.93750000000000000 ) ) ;
#6351 = CARTESIAN_POINT ( 'NONE',  ( 99.99999999999998579, 122.5000000021849615, -2.499999999999997780 ) ) ;
#6352 = AXIS2_PLACEMENT_3D ( 'NONE', #20558, #16117, #3018 ) ;
#6353 = CARTESIAN_POINT ( 'NONE',  ( 63.98586917393215145, 51.45790058219657936, 15.00000000000065548 ) ) ;
#6354 = ORIENTED_EDGE ( 'NONE', *, *, #24509, .T. ) ;
#6355 = CARTESIAN_POINT ( 'NONE',  ( 104.4587341249999639, 1.442382525525748735E-14, 6.937500001365592972 ) ) ;
#6356 = CYLINDRICAL_SURFACE ( 'NONE', #22603, 5.000000000000004441 ) ;
#6357 = ORIENTED_EDGE ( 'NONE', *, *, #13284, .F. ) ;
#6358 = CARTESIAN_POINT ( 'NONE',  ( 124.3771271284222308, 40.85117187499999147, -13.57481594606315412 ) ) ;
#6359 = CARTESIAN_POINT ( 'NONE',  ( 99.99999999999995737, 4.458734125000016313, 10.18750000136559208 ) ) ;
#6360 = CARTESIAN_POINT ( 'NONE',  ( 51.42518405393695957, 37.97382812716787726, 5.622872871577880183 ) ) ;
#6361 = AXIS2_PLACEMENT_3D ( 'NONE', #12998, #2211, #208 ) ;
#6362 = ADVANCED_FACE ( 'NONE', ( #10066 ), #18778, .T. ) ;
#6363 = CARTESIAN_POINT ( 'NONE',  ( 9.295050272127046043, 39.46210937608393010, -9.295050272127046043 ) ) ;
#6364 = CARTESIAN_POINT ( 'NONE',  ( 92.99999999999995737, 1.387778780781445676E-14, 0.000000000000000000 ) ) ;
#6365 = CARTESIAN_POINT ( 'NONE',  ( 95.54126587499995082, 79.75000000136560629, 1.846868145590724986 ) ) ;
#6366 = CARTESIAN_POINT ( 'NONE',  ( 78.14518615778179367, 37.18007812608393436, -1.609821015232357215E-15 ) ) ;
#6367 = CARTESIAN_POINT ( 'NONE',  ( 93.46109445667491400, 114.7507929638356785, -51.32500000273120122 ) ) ;
#6368 = CARTESIAN_POINT ( 'NONE',  ( -5.444914386472297529, 39.61093750108393152, -13.14518615778179722 ) ) ;
#6369 = DIRECTION ( 'NONE',  ( 0.000000000000000000, 0.000000000000000000, -1.000000000000000000 ) ) ;
#6370 = CARTESIAN_POINT ( 'NONE',  ( 1.907364849565526780E-15, 40.99999999999999289, 15.57481594606304576 ) ) ;
#6371 = CARTESIAN_POINT ( 'NONE',  ( 102.1631189606246295, 103.3426043859339103, -53.89999999453763735 ) ) ;
#6372 = CARTESIAN_POINT ( 'NONE',  ( 116.4251840539369596, 40.20624999999999005, 0.000000000000000000 ) ) ;
#6373 = ORIENTED_EDGE ( 'NONE', *, *, #4442, .F. ) ;
#6374 = CARTESIAN_POINT ( 'NONE',  ( -20.00000000000000000, 50.00000000000000000, 10.00000000000000178 ) ) ;
#6375 = DIRECTION ( 'NONE',  ( 0.000000000000000000, 0.000000000000000000, 1.000000000000000000 ) ) ;
#6376 = CARTESIAN_POINT ( 'NONE',  ( 99.99999999999995737, 79.68750000136559208, 4.458734124999988779 ) ) ;
#6377 = CARTESIAN_POINT ( 'NONE',  ( 116.8548138422182063, 35.84062500108394289, 5.444914386472304635 ) ) ;
#6378 = CARTESIAN_POINT ( 'NONE',  ( 59.37712712842213136, 36.18789062716787441, -13.57481594606304753 ) ) ;
#6379 = EDGE_CURVE ( 'NONE', #13072, #11653, #16212, .T. ) ;
#6380 = AXIS2_PLACEMENT_3D ( 'NONE', #11253, #19970, #6986 ) ;
#6381 = DIRECTION ( 'NONE',  ( 0.000000000000000000, 1.000000000000000000, 0.000000000000000000 ) ) ;
#6382 = CARTESIAN_POINT ( 'NONE',  ( 9.598844408820456309, 36.83281250216787583, -9.598844408820458085 ) ) ;
#6383 = CARTESIAN_POINT ( 'NONE',  ( 94.99999999999995737, 2.071067811865491048, 5.937500000000000000 ) ) ;
#6384 = CARTESIAN_POINT ( 'NONE',  ( -8.312177448680279460E-16, 35.24531249999999716, -13.57481594606304576 ) ) ;
#6385 =( GEOMETRIC_REPRESENTATION_CONTEXT ( 3 ) GLOBAL_UNCERTAINTY_ASSIGNED_CONTEXT ( ( #23810 ) ) GLOBAL_UNIT_ASSIGNED_CONTEXT ( ( #15640, #15061, #19778 ) ) REPRESENTATION_CONTEXT ( 'NONE', 'WORKASPACE' ) );
#6386 = EDGE_CURVE ( 'NONE', #9781, #10399, #8182, .T. ) ;
#6387 = CARTESIAN_POINT ( 'NONE',  ( 185.7049497278729575, 38.27148437608393294, 9.295050272127047819 ) ) ;
#6388 =( BOUNDED_SURFACE ( )  B_SPLINE_SURFACE ( 1, 2, ( 
 ( #22335, #1104, #9771, #821, #22476, #2940, #18480, #27187, #7199, #24465, #4948, #20334, #13612, #11472, #9489, #19708, #24132, #15561, #10994, #26270, #4608, #13264, #335, #4469, #21721, #15418, #6591, #9023, #26703, #26124, #2195, #6876, #17715, #22138, #24270, #23990, #24409, #7011, #2617, #192, #24557, #13411, #5039, #26559, #2760, #10857, #53, #6732, #4752, #26417, #9297, #8874, #4897, #15707, #21997, #2473, #19568, #19849, #11279, #15272, #22284, #20000, #8733, #480, #13127, #17566, #17426, #13561, #9162, #17993, #21862, #17854, #11423, #20142, #11134, #623, #7152, #15848, #2336, #22853, #18139 ),
 ( #22422, #27275, #20851, #1197, #13984, #20715, #26993, #18287, #20430, #11992, #7588, #9865, #11851, #16135, #13704, #18572, #3181, #14272, #26852, #25118, #16281, #20279, #7730, #20573, #5324, #9583, #3036, #18705, #5463, #15987, #27408, #1332, #913, #24982, #22990, #12125, #11704, #24841, #7299, #3459, #24701, #5605, #1054, #9726, #16421, #14132, #9997, #2893, #11562, #7869, #16564, #22711, #3320, #25255, #18429, #765, #27137, #9438, #5181, #13844, #22568, #7439, #24363, #20097, #24508, #575, #15517, #4996, #23941, #22094, #22235, #429, #6827, #9256, #9114, #17809, #17948, #26512, #21815, #24225, #20234 ) ),
 .UNSPECIFIED., .F., .F., .F. ) 
 B_SPLINE_SURFACE_WITH_KNOTS ( ( 2, 2 ),
 ( 3, 2, 2, 2, 2, 2, 2, 2, 2, 2, 2, 2, 2, 2, 2, 2, 2, 2, 2, 2, 2, 2, 2, 2, 2, 2, 2, 2, 2, 2, 2, 2, 2, 2, 2, 2, 2, 2, 2, 2, 3 ),
 ( 0.000000000000000000, 1.000000000000000000 ),
 ( 0.000000000000000000, 0.02500000000000000139, 0.05000000000000000278, 0.07499999999999999722, 0.1000000000000000056, 0.1250000000000000000, 0.1499999999999999944, 0.1749999999999999889, 0.2000000000000000111, 0.2250000000000000056, 0.2500000000000000000, 0.2750000000000000222, 0.2999999999999999889, 0.3250000000000000111, 0.3499999999999999778, 0.3750000000000000000, 0.4000000000000000222, 0.4249999999999999889, 0.4500000000000000111, 0.4749999999999999778, 0.5000000000000000000, 0.5250000000000000222, 0.5500000000000000444, 0.5749999999999999556, 0.5999999999999999778, 0.6250000000000000000, 0.6500000000000000222, 0.6750000000000000444, 0.6999999999999999556, 0.7249999999999999778, 0.7500000000000000000, 0.7750000000000000222, 0.8000000000000000444, 0.8249999999999999556, 0.8499999999999999778, 0.8750000000000000000, 0.9000000000000000222, 0.9250000000000000444, 0.9499999999999999556, 0.9749999999999999778, 1.000000000000000000 ),
 .UNSPECIFIED. ) 
 GEOMETRIC_REPRESENTATION_ITEM ( )  RATIONAL_B_SPLINE_SURFACE ( (
 ( 1.000000000000000000, 0.9238795325112867385, 1.000000000000000000, 0.9238795325112867385, 1.000000000000000000, 0.9238795325112867385, 1.000000000000000000, 0.9238795325112867385, 1.000000000000000000, 0.9238795325112867385, 1.000000000000000000, 0.9238795325112867385, 1.000000000000000000, 0.9238795325112867385, 1.000000000000000000, 0.9238795325112867385, 1.000000000000000000, 0.9238795325112867385, 1.000000000000000000, 0.9238795325112867385, 1.000000000000000000, 0.9238795325112867385, 1.000000000000000000, 0.9238795325112867385, 1.000000000000000000, 0.9238795325112867385, 1.000000000000000000, 0.9238795325112867385, 1.000000000000000000, 0.9238795325112867385, 1.000000000000000000, 0.9238795325112867385, 1.000000000000000000, 0.9238795325112867385, 1.000000000000000000, 0.9238795325112867385, 1.000000000000000000, 0.9238795325112867385, 1.000000000000000000, 0.9238795325112867385, 1.000000000000000000, 0.9238795325112867385, 1.000000000000000000, 0.9238795325112867385, 1.000000000000000000, 0.9238795325112867385, 1.000000000000000000, 0.9238795325112867385, 1.000000000000000000, 0.9238795325112867385, 1.000000000000000000, 0.9238795325112867385, 1.000000000000000000, 0.9238795325112867385, 1.000000000000000000, 0.9238795325112867385, 1.000000000000000000, 0.9238795325112867385, 1.000000000000000000, 0.9238795325112867385, 1.000000000000000000, 0.9238795325112867385, 1.000000000000000000, 0.9238795325112867385, 1.000000000000000000, 0.9238795325112867385, 1.000000000000000000, 0.9238795325112867385, 1.000000000000000000, 0.9238795325112867385, 1.000000000000000000, 0.9238795325112867385, 1.000000000000000000, 0.9238795325112867385, 1.000000000000000000, 0.9238795325112867385, 1.000000000000000000, 0.9238795325112867385, 1.000000000000000000, 0.9238795325112867385, 1.000000000000000000),
 ( 1.000000000000000000, 0.9238795325112867385, 1.000000000000000000, 0.9238795325112867385, 1.000000000000000000, 0.9238795325112867385, 1.000000000000000000, 0.9238795325112867385, 1.000000000000000000, 0.9238795325112867385, 1.000000000000000000, 0.9238795325112867385, 1.000000000000000000, 0.9238795325112867385, 1.000000000000000000, 0.9238795325112867385, 1.000000000000000000, 0.9238795325112867385, 1.000000000000000000, 0.9238795325112867385, 1.000000000000000000, 0.9238795325112867385, 1.000000000000000000, 0.9238795325112867385, 1.000000000000000000, 0.9238795325112867385, 1.000000000000000000, 0.9238795325112867385, 1.000000000000000000, 0.9238795325112867385, 1.000000000000000000, 0.9238795325112867385, 1.000000000000000000, 0.9238795325112867385, 1.000000000000000000, 0.9238795325112867385, 1.000000000000000000, 0.9238795325112867385, 1.000000000000000000, 0.9238795325112867385, 1.000000000000000000, 0.9238795325112867385, 1.000000000000000000, 0.9238795325112867385, 1.000000000000000000, 0.9238795325112867385, 1.000000000000000000, 0.9238795325112867385, 1.000000000000000000, 0.9238795325112867385, 1.000000000000000000, 0.9238795325112867385, 1.000000000000000000, 0.9238795325112867385, 1.000000000000000000, 0.9238795325112867385, 1.000000000000000000, 0.9238795325112867385, 1.000000000000000000, 0.9238795325112867385, 1.000000000000000000, 0.9238795325112867385, 1.000000000000000000, 0.9238795325112867385, 1.000000000000000000, 0.9238795325112867385, 1.000000000000000000, 0.9238795325112867385, 1.000000000000000000, 0.9238795325112867385, 1.000000000000000000, 0.9238795325112867385, 1.000000000000000000, 0.9238795325112867385, 1.000000000000000000, 0.9238795325112867385, 1.000000000000000000, 0.9238795325112867385, 1.000000000000000000, 0.9238795325112867385, 1.000000000000000000) ) ) 
 REPRESENTATION_ITEM ( '' )  SURFACE ( )  );
#6389 = CARTESIAN_POINT ( 'NONE',  ( 70.62287287157793969, 39.16445312500000142, -13.57481594606299247 ) ) ;
#6390 = EDGE_CURVE ( 'NONE', #18296, #24795, #20720, .T. ) ;
#6391 = CARTESIAN_POINT ( 'NONE',  ( 143.1451861577818079, 36.18789062608393436, -1.609821015232357215E-15 ) ) ;
#6392 = CARTESIAN_POINT ( 'NONE',  ( 195.0000000000000000, 37.72578125216787726, -13.57481594606304576 ) ) ;
#6393 = CARTESIAN_POINT ( 'NONE',  ( 99.99999999999995737, 5.000000000000018652, 6.749999999999999112 ) ) ;
#6394 = CARTESIAN_POINT ( 'NONE',  ( 133.0393970508025916, 53.88964894337313183, 14.99999999999997158 ) ) ;
#6395 = LINE ( 'NONE', #15204, #26184 ) ;
#6396 = CARTESIAN_POINT ( 'NONE',  ( 13.14518615778179900, 36.43593750108392726, -5.444914386472297529 ) ) ;
#6397 = CARTESIAN_POINT ( 'NONE',  ( 9.295050272127047819, 38.46992187608393010, 9.295050272127046043 ) ) ;
#6398 = CARTESIAN_POINT ( 'NONE',  ( 208.5748159460630120, 37.47773437500001137, -5.622872871577873077 ) ) ;
#6399 = LINE ( 'NONE', #6668, #28146 ) ;
#6400 = CARTESIAN_POINT ( 'NONE',  ( 96.84719886470459471, 3.152801135295383084, 1.562500001365592972 ) ) ;
#6401 = CARTESIAN_POINT ( 'NONE',  ( 51.85481384221820633, 37.37851562608393863, 0.000000000000000000 ) ) ;
#6402 = AXIS2_PLACEMENT_3D ( 'NONE', #8150, #22854, #16565 ) ;
#6403 = CARTESIAN_POINT ( 'NONE',  ( 103.1528011352953342, -3.152801135295355106, 0.8125000013655924169 ) ) ;
#6404 = DIRECTION ( 'NONE',  ( 1.000000000000000000, 0.000000000000000000, 0.000000000000000000 ) ) ;
#6405 = CARTESIAN_POINT ( 'NONE',  ( 96.84719886470463734, 93.93749999863440792, 3.152801135295351997 ) ) ;
#6406 = CARTESIAN_POINT ( 'NONE',  ( 95.00000000000000000, 93.37499999726881583, -7.551217303480904118E-15 ) ) ;
#6407 = CARTESIAN_POINT ( 'NONE',  ( -8.312177448680279460E-16, 37.62656249999999858, -13.57481594606304576 ) ) ;
#6408 = DIRECTION ( 'NONE',  ( -1.000000000000000000, 0.000000000000000000, 0.000000000000000000 ) ) ;
#6409 = ORIENTED_EDGE ( 'NONE', *, *, #22053, .T. ) ;
#6410 = CARTESIAN_POINT ( 'NONE',  ( 95.54126587499996504, 80.68750000136559208, -1.387778780781445676E-14 ) ) ;
#6411 = CARTESIAN_POINT ( 'NONE',  ( 101.8468681455907330, 95.12499999863439371, 4.458734124999979898 ) ) ;
#6412 = ORIENTED_EDGE ( 'NONE', *, *, #23068, .T. ) ;
#6413 = CARTESIAN_POINT ( 'NONE',  ( 95.67376207875069838, 115.9545556584642867, -51.30000000000000426 ) ) ;
#6414 = CARTESIAN_POINT ( 'NONE',  ( 78.14518615778179367, 34.05468750108394005, -5.444914386472297529 ) ) ;
#6415 = APPLICATION_CONTEXT ( 'automotive_design' ) ;
#6416 = VERTEX_POINT ( 'NONE', #7665 ) ;
#6417 = CARTESIAN_POINT ( 'NONE',  ( 136.1165602397167902, 54.66944451632673463, -15.00000000000000000 ) ) ;
#6418 = CARTESIAN_POINT ( 'NONE',  ( 103.1528011352953342, 3.152801135295383084, 3.312500001365592972 ) ) ;
#6419 = ORIENTED_EDGE ( 'NONE', *, *, #16651, .T. ) ;
#6420 = CARTESIAN_POINT ( 'NONE',  ( -9.295050272127046043, 35.09648437608393579, -9.295050272127046043 ) ) ;
#6421 = CARTESIAN_POINT ( 'NONE',  ( 9.295050272127047819, 40.25585937608393294, 9.295050272127046043 ) ) ;
#6422 = CARTESIAN_POINT ( 'NONE',  ( 189.3771271284221314, 36.98164062716787015, -13.57481594606304753 ) ) ;
#6423 = CARTESIAN_POINT ( 'NONE',  ( -13.14518615778179544, 35.79101562608393294, 0.000000000000000000 ) ) ;
#6424 = PLANE ( 'NONE',  #17575 ) ;
#6425 = LINE ( 'NONE', #23814, #3087 ) ;
#6426 = CARTESIAN_POINT ( 'NONE',  ( 135.4449143864723339, 37.32890625108393579, -13.14518615778179722 ) ) ;
#6427 = CARTESIAN_POINT ( 'NONE',  ( 2.414731522848535132E-15, 36.98164062608393721, 13.14518615778179544 ) ) ;
#6428 = CARTESIAN_POINT ( 'NONE',  ( 116.8548138422182063, 33.45937500108392726, 5.444914386472304635 ) ) ;
#6429 = CARTESIAN_POINT ( 'NONE',  ( 74.59884440882045453, 33.55859375000000000, -9.598844408820458085 ) ) ;
#6430 = CARTESIAN_POINT ( 'NONE',  ( 102.4999999999999858, 123.0000000000000000, -8.724596124144689908E-15 ) ) ;
#6431 = CARTESIAN_POINT ( 'NONE',  ( 96.84719886470459471, -3.152801135295355994, 13.81250000136559208 ) ) ;
#6432 = CYLINDRICAL_SURFACE ( 'NONE', #7115, 13.57481594606304398 ) ;
#6433 =( BOUNDED_CURVE ( )  B_SPLINE_CURVE ( 2, ( #9368, #9652, #5536, #25052, #22783, #18502, #7935, #18773, #3253, #7366, #7660 ),
 .UNSPECIFIED., .F., .F. ) 
 B_SPLINE_CURVE_WITH_KNOTS ( ( 3, 2, 2, 2, 2, 3 ),
 ( 0.3999999999999996891, 0.4199999999999996514, 0.4399999999999996692, 0.4599999999999996869, 0.4799999999999996492, 0.4999999999999996669 ),
 .UNSPECIFIED. ) 
 CURVE ( )  GEOMETRIC_REPRESENTATION_ITEM ( )  RATIONAL_B_SPLINE_CURVE ( ( 1.000000000000000888, 0.9510565162951527540, 1.000000000000000000, 0.9510565162951535312, 1.000000000000000000, 0.9510565162951535312, 1.000000000000000000, 0.9510565162951535312, 1.000000000000000000, 0.9510565162951543083, 0.9999999999999992228 ) ) 
 REPRESENTATION_ITEM ( '' )  );
#6434 = CARTESIAN_POINT ( 'NONE',  ( 95.54126587499995082, 1.846868145590750077, 4.375000001365592084 ) ) ;
#6435 = CARTESIAN_POINT ( 'NONE',  ( 104.9999999999999716, 1.449011120738813565E-14, 3.625000002731184612 ) ) ;
#6436 = CARTESIAN_POINT ( 'NONE',  ( 0.000000000000000000, 36.00000000000000000, 0.000000000000000000 ) ) ;
#6437 = CARTESIAN_POINT ( 'NONE',  ( 99.99999999999995737, 80.93750000136559208, 4.458734124999988779 ) ) ;
#6438 = CARTESIAN_POINT ( 'NONE',  ( 9.295050272127047819, 33.70742187608393436, 9.295050272127046043 ) ) ;
#6439 = CARTESIAN_POINT ( 'NONE',  ( -5.444914386472299306, 40.10703125108393152, 13.14518615778179722 ) ) ;
#6440 = CARTESIAN_POINT ( 'NONE',  ( 102.4976396683250783, 117.6869444889999841, -46.47499999726882436 ) ) ;
#6441 = ORIENTED_EDGE ( 'NONE', *, *, #18222, .F. ) ;
#6442 = CARTESIAN_POINT ( 'NONE',  ( 102.0669873000000081, 124.3000000010924708, 0.8561741729129311862 ) ) ;
#6443 = CARTESIAN_POINT ( 'NONE',  ( 98.09035273295538104, 123.0000000000000142, 0.7910017786517971050 ) ) ;
#6444 = DIRECTION ( 'NONE',  ( -0.000000000000000000, 1.000000000000000000, -0.000000000000000000 ) ) ;
#6445 = CARTESIAN_POINT ( 'NONE',  ( 204.2950502721270425, 40.05742187608392868, 9.295050272127046043 ) ) ;
#6446 = ORIENTED_EDGE ( 'NONE', *, *, #20656, .F. ) ;
#6447 = LINE ( 'NONE', #24260, #27017 ) ;
#6448 = DIRECTION ( 'NONE',  ( 1.000000000000000000, 0.000000000000000000, 0.000000000000000000 ) ) ;
#6449 = CARTESIAN_POINT ( 'NONE',  ( 130.0000000000000000, 39.61093749999999147, 13.57481594606304576 ) ) ;
#6450 = ORIENTED_EDGE ( 'NONE', *, *, #25620, .T. ) ;
#6451 = CARTESIAN_POINT ( 'NONE',  ( 97.83688103937538472, 116.6573956140660897, -50.40000000000000568 ) ) ;
#6452 = CARTESIAN_POINT ( 'NONE',  ( 2.414731522848535132E-15, 38.37070312608393152, 13.14518615778179544 ) ) ;
#6453 = CARTESIAN_POINT ( 'NONE',  ( 97.93301269999999192, 123.1000000010924822, -0.8561741729129505041 ) ) ;
#6454 = CARTESIAN_POINT ( 'NONE',  ( 135.4449143864723055, 39.51171875108392584, -13.14518615778179900 ) ) ;
#6455 = SURFACE_STYLE_FILL_AREA ( #25318 ) ;
#6456 = CARTESIAN_POINT ( 'NONE',  ( 104.3262379212492590, 104.0454443415356991, -43.80000000546237970 ) ) ;
#6457 = CARTESIAN_POINT ( 'NONE',  ( -9.598844408820458085, 34.65000000216787868, -9.598844408820458085 ) ) ;
#6458 = CARTESIAN_POINT ( 'NONE',  ( 204.2950502721270425, 33.90585937608393863, 9.295050272127046043 ) ) ;
#6459 = ORIENTED_EDGE ( 'NONE', *, *, #12876, .F. ) ;
#6460 = ORIENTED_EDGE ( 'NONE', *, *, #23415, .T. ) ;
#6461 = CARTESIAN_POINT ( 'NONE',  ( 13.14518615778179900, 38.02343750108395426, -5.444914386472297529 ) ) ;
#6462 = FILL_AREA_STYLE_COLOUR ( '', #12641 ) ;
#6463 = CARTESIAN_POINT ( 'NONE',  ( 99.99999999999995737, -4.458734124999988779, 12.93750000136559208 ) ) ;
#6464 =( BOUNDED_CURVE ( )  B_SPLINE_CURVE ( 2, ( #4213, #15017, #23738, #12870, #2223, #10887, #10746, #19457, #28155, #26010, #19595 ),
 .UNSPECIFIED., .F., .T. ) 
 B_SPLINE_CURVE_WITH_KNOTS ( ( 3, 2, 2, 2, 2, 3 ),
 ( 0.6999999999999998446, 0.7199999999999998623, 0.7399999999999998801, 0.7600000000000000089, 0.7800000000000000266, 0.8000000000000000444 ),
 .UNSPECIFIED. ) 
 CURVE ( )  GEOMETRIC_REPRESENTATION_ITEM ( )  RATIONAL_B_SPLINE_CURVE ( ( 1.000000000000000222, 0.9510565162951533091, 1.000000000000000000, 0.9510565162951535312, 1.000000000000000000, 0.9510565162951535312, 1.000000000000000000, 0.9510565162951535312, 1.000000000000000000, 0.9510565162951535312, 1.000000000000000000 ) ) 
 REPRESENTATION_ITEM ( '' )  );
#6465 = CARTESIAN_POINT ( 'NONE',  ( 70.44491438647229131, 39.21406250108392300, 13.14518615778179189 ) ) ;
#6466 = CARTESIAN_POINT ( 'NONE',  ( 95.54126587499996504, 79.43750000136559208, -1.387778780781445676E-14 ) ) ;
#6467 = CARTESIAN_POINT ( 'NONE',  ( 189.5550856135277229, 39.90859375108392726, 13.14518615778179722 ) ) ;
#6468 = CARTESIAN_POINT ( 'NONE',  ( 5.444914386472302859, 37.82500000108392868, 13.14518615778179189 ) ) ;
#6469 = EDGE_CURVE ( 'NONE', #10849, #27236, #12847, .T. ) ;
#6470 = CARTESIAN_POINT ( 'NONE',  ( 77.07727640983618755, 35.99999999999999289, -6.197985357348143154 ) ) ;
#6471 = CARTESIAN_POINT ( 'NONE',  ( 104.4587341249999781, 90.31249999863440792, -6.938893903907228378E-15 ) ) ;
#6472 = CARTESIAN_POINT ( 'NONE',  ( 97.50236033167490746, 117.6869444889999841, -50.02499999726882152 ) ) ;
#6473 = ORIENTED_EDGE ( 'NONE', *, *, #18158, .T. ) ;
#6474 = CARTESIAN_POINT ( 'NONE',  ( 2.493653234604083739E-15, 35.64218749999999147, 13.57481594606304576 ) ) ;
#6475 = CARTESIAN_POINT ( 'NONE',  ( -13.14518615778179900, 36.53515625108392584, -5.444914386472297529 ) ) ;
#6476 = CARTESIAN_POINT ( 'NONE',  ( 97.92893218813451028, -4.999999999999989342, 0.3125000027311853890 ) ) ;
#6477 = CARTESIAN_POINT ( 'NONE',  ( 135.4449143864723055, 34.94765625108394147, -13.14518615778179900 ) ) ;
#6478 = CARTESIAN_POINT ( 'NONE',  ( 74.29505027212704249, 32.31835937608393294, -9.295050272127046043 ) ) ;
#6479 = CIRCLE ( 'NONE', #9685, 13.57481594606304398 ) ;
#6480 = CARTESIAN_POINT ( 'NONE',  ( 208.1451861577817795, 37.22968750108393721, -5.444914386472297529 ) ) ;
#6481 = DIRECTION ( 'NONE',  ( 0.000000000000000000, 1.000000000000000000, 0.000000000000000000 ) ) ;
#6482 = CARTESIAN_POINT ( 'NONE',  ( 3.755638265659908104, 31.58960998161716560, -13.14518615778179900 ) ) ;
#6483 = CARTESIAN_POINT ( 'NONE',  ( 131.0141308260786559, 51.45790058219927232, -14.99999999999932676 ) ) ;
#6484 = LINE ( 'NONE', #27881, #3944 ) ;
#6485 = CARTESIAN_POINT ( 'NONE',  ( 13.14518615778179900, 33.16171875108393863, 5.444914386472293977 ) ) ;
#6486 = DIRECTION ( 'NONE',  ( -0.000000000000000000, 1.000000000000000000, -0.000000000000000000 ) ) ;
#6487 = CARTESIAN_POINT ( 'NONE',  ( -8.049105076161786076E-16, 34.79882812608393294, -13.14518615778179544 ) ) ;
#6488 = CARTESIAN_POINT ( 'NONE',  ( -15.00000000000000000, 55.00000000000000000, 10.00000000000000000 ) ) ;
#6489 = CARTESIAN_POINT ( 'NONE',  ( 99.99999999999998579, 123.7000000021849502, 2.499999999999978684 ) ) ;
#6490 = DIRECTION ( 'NONE',  ( -0.000000000000000000, -1.000000000000000000, -0.000000000000000000 ) ) ;
#6491 = CARTESIAN_POINT ( 'NONE',  ( -9.598844408820454532, 37.13046874999999147, 9.598844408820459861 ) ) ;
#6492 = CARTESIAN_POINT ( 'NONE',  ( 104.4587341249999639, 1.442382525525748735E-14, 8.937500001365592084 ) ) ;
#6493 = VERTEX_POINT ( 'NONE', #21197 ) ;
#6494 = CARTESIAN_POINT ( 'NONE',  ( 101.4615807364564546, 124.0500000010924850, 1.461580736456455476 ) ) ;
#6495 = CARTESIAN_POINT ( 'NONE',  ( 103.1528011352953342, 3.152801135295383084, 13.06250000136559208 ) ) ;
#6496 = CARTESIAN_POINT ( 'NONE',  ( 120.8198241863519939, 55.00000000000001421, 14.99999999999996625 ) ) ;
#6497 = CARTESIAN_POINT ( 'NONE',  ( -9.295050272127044266, 39.85898437608393152, 9.295050272127047819 ) ) ;
#6498 = CARTESIAN_POINT ( 'NONE',  ( 99.99999999999998579, 124.3999999999999915, 2.499999999999978684 ) ) ;
#6499 = CARTESIAN_POINT ( 'NONE',  ( 98.15313185440925281, 82.87500000136560629, 4.458734124999987891 ) ) ;
#6500 = CARTESIAN_POINT ( 'NONE',  ( 78.14518615778179367, 36.43593750108392726, -5.444914386472297529 ) ) ;
#6501 = CARTESIAN_POINT ( 'NONE',  ( 95.00472066334982912, 116.8754121666685393, -49.42500000273118133 ) ) ;
#6502 = CARTESIAN_POINT ( 'NONE',  ( 94.99999999999995737, 1.387778780781445676E-14, 12.00000000000000000 ) ) ;
#6503 = ORIENTED_EDGE ( 'NONE', *, *, #22032, .T. ) ;
#6504 = ADVANCED_FACE ( 'NONE', ( #8354 ), #6087, .T. ) ;
#6505 = DIRECTION ( 'NONE',  ( 0.000000000000000000, 0.000000000000000000, -1.000000000000000000 ) ) ;
#6506 = CARTESIAN_POINT ( 'NONE',  ( 0.000000000000000000, 36.00000000000000000, 0.000000000000000000 ) ) ;
#6507 = CARTESIAN_POINT ( 'NONE',  ( 116.4251840539369596, 36.23749999999999005, 0.000000000000000000 ) ) ;
#6508 = ORIENTED_EDGE ( 'NONE', *, *, #10913, .F. ) ;
#6509 = CARTESIAN_POINT ( 'NONE',  ( 0.000000000000000000, 40.99999999999999289, 0.000000000000000000 ) ) ;
#6510 = EDGE_CURVE ( 'NONE', #5706, #7474, #24539, .T. ) ;
#6511 = CARTESIAN_POINT ( 'NONE',  ( -9.295050272127046043, 35.89023437608393152, -9.295050272127046043 ) ) ;
#6512 = CARTESIAN_POINT ( 'NONE',  ( -8.312177448680279460E-16, 37.72578125216787726, -13.57481594606304576 ) ) ;
#6513 = CARTESIAN_POINT ( 'NONE',  ( 130.0000000000000000, 37.57695312608392868, 13.14518615778179544 ) ) ;
#6514 = CARTESIAN_POINT ( 'NONE',  ( 59.37712712842213136, 34.10429687716786873, 13.57481594606304753 ) ) ;
#6515 = CARTESIAN_POINT ( 'NONE',  ( 103.5355339059327093, 83.62500000000000000, -3.535533905932755072 ) ) ;
#6516 = CARTESIAN_POINT ( 'NONE',  ( -9.598844408820458085, 31.47500000216787441, -9.598844408820458085 ) ) ;
#6517 = CARTESIAN_POINT ( 'NONE',  ( 97.92893218813451028, 5.000000000000018652, 5.812500000000000000 ) ) ;
#6518 = EDGE_CURVE ( 'NONE', #23304, #19109, #12510, .T. ) ;
#6519 = CARTESIAN_POINT ( 'NONE',  ( 104.9952793366501567, 103.1245878333314465, -47.17499999726882010 ) ) ;
#6520 = CARTESIAN_POINT ( 'NONE',  ( 185.7049497278729575, 37.27929687608393294, -9.295050272127046043 ) ) ;
#6521 = DIRECTION ( 'NONE',  ( -1.000000000000000000, -3.469446951953617147E-16, 2.385244779468109755E-16 ) ) ;
#6522 = CARTESIAN_POINT ( 'NONE',  ( 101.0355339059327235, 122.9500000021849502, 2.499999999999977796 ) ) ;
#6523 = CARTESIAN_POINT ( 'NONE',  ( 99.99999999999998579, 90.00000000000000000, -6.938893903907228378E-15 ) ) ;
#6524 = CARTESIAN_POINT ( 'NONE',  ( 195.0000000000000000, 36.83281249999999574, -13.57481594606304576 ) ) ;
#6525 = CARTESIAN_POINT ( 'NONE',  ( -5.622872871577873077, 37.67617187499999432, -13.57481594606304753 ) ) ;
#6526 = CARTESIAN_POINT ( 'NONE',  ( 51.42518405393695957, 37.03124999999999289, 0.000000000000000000 ) ) ;
#6527 = CARTESIAN_POINT ( 'NONE',  ( -13.14518615778179189, 36.83281250108393579, 5.444914386472304635 ) ) ;
#6528 = CARTESIAN_POINT ( 'NONE',  ( -5.444914386472297529, 39.61093750108393152, -13.14518615778179900 ) ) ;
#6529 = CARTESIAN_POINT ( 'NONE',  ( 204.5988444088204687, 35.74140624999999716, 9.598844408820456309 ) ) ;
#6530 = EDGE_CURVE ( 'NONE', #23121, #26178, #21849, .T. ) ;
#6531 = CARTESIAN_POINT ( 'NONE',  ( 108.0825317500000153, 110.0000000000000000, -44.37500000273119838 ) ) ;
#6532 = CARTESIAN_POINT ( 'NONE',  ( -8.312177448680279460E-16, 32.86406249999999574, -13.57481594606304576 ) ) ;
#6533 = CARTESIAN_POINT ( 'NONE',  ( 59.55508561352770158, 36.43593750108392726, -13.14518615778179900 ) ) ;
#6534 = CARTESIAN_POINT ( 'NONE',  ( 96.84719886470459471, -3.152801135295355994, 2.562500001365592084 ) ) ;
#6535 = DIRECTION ( 'NONE',  ( 0.000000000000000000, -1.000000000000000000, 0.000000000000000000 ) ) ;
#6536 = CARTESIAN_POINT ( 'NONE',  ( 96.84719886470463734, 92.93749999863440792, 3.152801135295351997 ) ) ;
#6537 = CARTESIAN_POINT ( 'NONE',  ( 0.000000000000000000, 10.00000000000000000, 19.22649730810373470 ) ) ;
#6538 = CARTESIAN_POINT ( 'NONE',  ( -8.312177448680279460E-16, 36.83281249999999574, -13.57481594606304576 ) ) ;
#6539 = DIRECTION ( 'NONE',  ( -1.000000000000000000, 0.000000000000000000, 2.385244779468110248E-16 ) ) ;
#6540 = VERTEX_POINT ( 'NONE', #28169 ) ;
#6541 = CARTESIAN_POINT ( 'NONE',  ( 94.99999999999995737, 83.06250000000001421, 2.071067811865466624 ) ) ;
#6542 = CARTESIAN_POINT ( 'NONE',  ( 103.1528011352953484, 94.43749999863440792, -3.152801135295366208 ) ) ;
#6543 = CARTESIAN_POINT ( 'NONE',  ( 65.37454041347797329, 36.00000000000002842, -13.51869779562200691 ) ) ;
#6544 = ORIENTED_EDGE ( 'NONE', *, *, #14200, .T. ) ;
#6545 = EDGE_CURVE ( 'NONE', #9529, #23888, #3894, .T. ) ;
#6546 = CARTESIAN_POINT ( 'NONE',  ( 93.00000000000000000, 112.2744378736303332, -51.10000000000000142 ) ) ;
#6547 = CARTESIAN_POINT ( 'NONE',  ( 65.00000000000000000, 34.60039062608393579, 13.14518615778179544 ) ) ;
#6548 = EDGE_LOOP ( 'NONE', ( #22161, #16522, #12528, #3866 ) ) ;
#6549 =( BOUNDED_CURVE ( )  B_SPLINE_CURVE ( 2, ( #7538, #27367, #20667, #26947, #18525, #12080, #18380, #1151, #22948 ),
 .UNSPECIFIED., .F., .T. ) 
 B_SPLINE_CURVE_WITH_KNOTS ( ( 3, 2, 2, 2, 3 ),
 ( 0.2291666666666665741, 0.2395833333333332316, 0.2499999999999998335, 0.2604166666666665186, 0.2708333333333330928 ),
 .UNSPECIFIED. ) 
 CURVE ( )  GEOMETRIC_REPRESENTATION_ITEM ( )  RATIONAL_B_SPLINE_CURVE ( ( 1.000000000000000666, 0.9238795325112861834, 1.000000000000000000, 0.9238795325112867385, 1.000000000000000000, 0.9238795325112867385, 1.000000000000000000, 0.9238795325112884038, 0.9999999999999983347 ) ) 
 REPRESENTATION_ITEM ( '' )  );
#6550 = CARTESIAN_POINT ( 'NONE',  ( 98.15313185440925281, -4.458734124999987891, 3.875000001365592084 ) ) ;
#6551 = ORIENTED_EDGE ( 'NONE', *, *, #7742, .T. ) ;
#6552 = CARTESIAN_POINT ( 'NONE',  ( 13.14518615778179722, 33.95546875108394147, 5.444914386472293977 ) ) ;
#6553 = CARTESIAN_POINT ( 'NONE',  ( -5.444914386472299306, 40.10703125108393152, 13.14518615778179722 ) ) ;
#6554 = CARTESIAN_POINT ( 'NONE',  ( 181.4251840539369596, 37.08085937716786873, -5.622872871577873077 ) ) ;
#6555 = CARTESIAN_POINT ( 'NONE',  ( -5.444914386472299306, 35.14609375108393152, 13.14518615778179722 ) ) ;
#6556 = DIRECTION ( 'NONE',  ( 0.000000000000000000, 0.000000000000000000, -1.000000000000000000 ) ) ;
#6557 = CARTESIAN_POINT ( 'NONE',  ( 200.6228728715778971, 39.75976562716787299, 13.57481594606306174 ) ) ;
#6558 = ORIENTED_EDGE ( 'NONE', *, *, #14372, .F. ) ;
#6559 = CARTESIAN_POINT ( 'NONE',  ( -8.049105076161786076E-16, 38.17226562608394147, -13.14518615778179544 ) ) ;
#6560 = CARTESIAN_POINT ( 'NONE',  ( 143.1451861577818079, 36.18789062608393436, -1.609821015232357215E-15 ) ) ;
#6561 = CARTESIAN_POINT ( 'NONE',  ( 70.62287287157786864, 34.40195312499999858, -13.57481594606304753 ) ) ;
#6562 = CARTESIAN_POINT ( 'NONE',  ( 104.9999999999999716, 2.071067811865491937, 9.562499999999998224 ) ) ;
#6563 = CARTESIAN_POINT ( 'NONE',  ( 104.4587341249999781, -1.846868145590721655, 9.125000001365592084 ) ) ;
#6564 = CARTESIAN_POINT ( 'NONE',  ( 200.3649479647158671, 36.00000000000000000, 12.09311862596019260 ) ) ;
#6565 = CIRCLE ( 'NONE', #25675, 23.00000000000001421 ) ;
#6566 = CARTESIAN_POINT ( 'NONE',  ( 96.84719886470459471, 3.152801135295383084, 1.312500001365592750 ) ) ;
#6567 = CARTESIAN_POINT ( 'NONE',  ( 93.46109445667491400, 114.7507929638356785, -49.32500000273120122 ) ) ;
#6568 = CARTESIAN_POINT ( 'NONE',  ( 101.0355339059327235, 123.9500000000000028, -2.499999999999996447 ) ) ;
#6569 = CARTESIAN_POINT ( 'NONE',  ( 95.54126587499996504, 79.75000000136560629, 1.846868145590724986 ) ) ;
#6570 = CARTESIAN_POINT ( 'NONE',  ( 108.0825317499999869, 107.3738262389971680, -50.72499999726881725 ) ) ;
#6571 = CARTESIAN_POINT ( 'NONE',  ( -5.444914386472297529, 36.63437500108393152, -13.14518615778179900 ) ) ;
#6572 = CARTESIAN_POINT ( 'NONE',  ( 91.91746824999997045, 107.3738262389971538, -49.77499999726881441 ) ) ;
#6573 = ORIENTED_EDGE ( 'NONE', *, *, #2740, .T. ) ;
#6574 = CARTESIAN_POINT ( 'NONE',  ( 94.33688103937537051, 114.1144967660473242, -50.70000000546238539 ) ) ;
#6575 = CARTESIAN_POINT ( 'NONE',  ( 104.9999999999999716, 1.449011120738813565E-14, 10.49999999999999822 ) ) ;
#6576 = CARTESIAN_POINT ( 'NONE',  ( 99.55174954624675365, 123.0000000000000426, -2.068055351820230481 ) ) ;
#6577 = ADVANCED_FACE ( 'NONE', ( #10483 ), #21615, .F. ) ;
#6578 = CARTESIAN_POINT ( 'NONE',  ( 185.7049497278729575, 37.47773437608393010, 9.295050272127047819 ) ) ;
#6579 = ORIENTED_EDGE ( 'NONE', *, *, #9687, .T. ) ;
#6580 = CARTESIAN_POINT ( 'NONE',  ( 94.99999999999995737, -2.071067811865466624, 7.187500002731185056 ) ) ;
#6581 = PLANE ( 'NONE',  #10250 ) ;
#6582 = CARTESIAN_POINT ( 'NONE',  ( 95.54126587499995082, 1.846868145590750077, 13.62500000136559386 ) ) ;
#6583 = ORIENTED_EDGE ( 'NONE', *, *, #25568, .F. ) ;
#6584 = CARTESIAN_POINT ( 'NONE',  ( 104.3262379212492590, 115.9545556584642867, -48.70000000000000284 ) ) ;
#6585 = VECTOR ( 'NONE', #10404, 1000.000000000000000 ) ;
#6586 = CARTESIAN_POINT ( 'NONE',  ( 120.4011555911795455, 37.72578124999999005, -9.598844408820458085 ) ) ;
#6587 = CARTESIAN_POINT ( 'NONE',  ( 97.92893218813446765, 81.31250000273119838, 4.999999999999962697 ) ) ;
#6588 = CARTESIAN_POINT ( 'NONE',  ( 130.0000000000000000, 40.35507812608393152, -13.14518615778179544 ) ) ;
#6589 = CARTESIAN_POINT ( 'NONE',  ( -13.14518615778179722, 39.90859375108393436, -5.444914386472297529 ) ) ;
#6590 =( BOUNDED_CURVE ( )  B_SPLINE_CURVE ( 2, ( #22612, #18033, #3082, #17896, #26746, #7188, #18472, #15886, #24602 ),
 .UNSPECIFIED., .F., .F. ) 
 B_SPLINE_CURVE_WITH_KNOTS ( ( 3, 2, 2, 2, 3 ),
 ( 0.1875000000000001388, 0.1979166666666667407, 0.2083333333333333703, 0.2187499999999999722, 0.2291666666666665741 ),
 .UNSPECIFIED. ) 
 CURVE ( )  GEOMETRIC_REPRESENTATION_ITEM ( )  RATIONAL_B_SPLINE_CURVE ( ( 0.9999999999999990008, 0.9238795325112877377, 1.000000000000000000, 0.9238795325112867385, 1.000000000000000000, 0.9238795325112867385, 1.000000000000000000, 0.9238795325112872936, 0.9999999999999994449 ) ) 
 REPRESENTATION_ITEM ( '' )  );
#6591 = CARTESIAN_POINT ( 'NONE',  ( 96.46446609406726225, 92.49999999726880162, 3.535533905932723986 ) ) ;
#6592 = CARTESIAN_POINT ( 'NONE',  ( 59.55508561352770158, 39.31328125108394289, 13.14518615778179722 ) ) ;
#6593 = DIRECTION ( 'NONE',  ( 1.000000000000000000, 0.000000000000000000, 0.000000000000000000 ) ) ;
#6594 = CARTESIAN_POINT ( 'NONE',  ( 185.7049497278729575, 33.50898437608393010, -9.295050272127046043 ) ) ;
#6595 = ORIENTED_EDGE ( 'NONE', *, *, #27563, .T. ) ;
#6596 = ORIENTED_EDGE ( 'NONE', *, *, #6276, .T. ) ;
#6597 = ORIENTED_EDGE ( 'NONE', *, *, #22907, .F. ) ;
#6598 = CARTESIAN_POINT ( 'NONE',  ( 9.295050272127047819, 37.87460937608393863, 9.295050272127046043 ) ) ;
#6599 = CARTESIAN_POINT ( 'NONE',  ( 101.8468681455907046, -4.458734124999987891, 10.00000000136559386 ) ) ;
#6600 = CARTESIAN_POINT ( 'NONE',  ( 74.29505027212704249, 39.46210937608393010, -9.295050272127046043 ) ) ;
#6601 = CARTESIAN_POINT ( 'NONE',  ( 98.15313185440923860, 81.25000000136559208, -4.458734125000016313 ) ) ;
#6602 = CARTESIAN_POINT ( 'NONE',  ( 181.8548138422182205, 39.80937500108393579, 5.444914386472304635 ) ) ;
#6603 = CARTESIAN_POINT ( 'NONE',  ( -13.14518615778179722, 39.11484375108393863, -5.444914386472297529 ) ) ;
#6604 = CARTESIAN_POINT ( 'NONE',  ( 188.5491206573239253, 50.00000000106884102, 11.97362904074905998 ) ) ;
#6605 = DIRECTION ( 'NONE',  ( 0.000000000000000000, -1.000000000000000000, 0.000000000000000000 ) ) ;
#6606 = CARTESIAN_POINT ( 'NONE',  ( 107.0000000000000000, 107.7255621263696241, -49.10000000000000853 ) ) ;
#6607 = CARTESIAN_POINT ( 'NONE',  ( 97.50236033167490746, 117.6869444889999841, -46.27499999726882152 ) ) ;
#6608 = ORIENTED_EDGE ( 'NONE', *, *, #6865, .T. ) ;
#6609 = CARTESIAN_POINT ( 'NONE',  ( -13.57481594606304576, 37.87460937499999147, 5.622872871577880183 ) ) ;
#6610 = CARTESIAN_POINT ( 'NONE',  ( 5.444914386472297529, 37.13046875108393152, -13.14518615778179900 ) ) ;
#6611 = COLOUR_RGB ( '', 0.40784314, 0.44705882, 0.49803922) ;
#6612 = AXIS2_PLACEMENT_3D ( 'NONE', #6236, #16647, #7818 ) ;
#6613 = CARTESIAN_POINT ( 'NONE',  ( 104.9999999999999716, 1.449011120738813565E-14, 1.625000002731184834 ) ) ;
#6614 = CARTESIAN_POINT ( 'NONE',  ( 120.7049497278729575, 37.67617187608393436, 9.295050272127047819 ) ) ;
#6615 = CARTESIAN_POINT ( 'NONE',  ( 59.55508561352770158, 32.46718750108393436, -13.14518615778179900 ) ) ;
#6616 = CARTESIAN_POINT ( 'NONE',  ( 189.5550856135277229, 37.42812500108394147, -13.14518615778179900 ) ) ;
#6617 = EDGE_LOOP ( 'NONE', ( #27946, #26541, #2874 ) ) ;
#6618 = CARTESIAN_POINT ( 'NONE',  ( 65.70502410996888898, 35.99999999999997158, 13.13343125082108287 ) ) ;
#6619 = CARTESIAN_POINT ( 'NONE',  ( 132.1699565831061420, 49.99999999883939950, -13.43548448457870670 ) ) ;
#6620 = CARTESIAN_POINT ( 'NONE',  ( -8.312177448680279460E-16, 39.21406249999999716, -13.57481594606304576 ) ) ;
#6621 = DIRECTION ( 'NONE',  ( 0.000000000000000000, 1.000000000000000000, 0.000000000000000000 ) ) ;
#6622 = DIRECTION ( 'NONE',  ( 0.000000000000000000, -1.000000000000000000, 0.000000000000000000 ) ) ;
#6623 = ADVANCED_FACE ( 'NONE', ( #2091 ), #9103, .F. ) ;
#6624 = CARTESIAN_POINT ( 'NONE',  ( 13.14518615778179544, 35.39414062608393152, -1.609821015232357215E-15 ) ) ;
#6625 = FACE_BOUND ( 'NONE', #1652, .T. ) ;
#6626 = CARTESIAN_POINT ( 'NONE',  ( 98.96446609406727646, 124.1500000021849672, -2.499999999999997780 ) ) ;
#6627 = CARTESIAN_POINT ( 'NONE',  ( 98.23223304703363112, 124.1000000000000085, -1.767766952966370209 ) ) ;
#6628 = CARTESIAN_POINT ( 'NONE',  ( -9.598844408820458085, 36.93203124999999432, -9.598844408820458085 ) ) ;
#6629 = CARTESIAN_POINT ( 'NONE',  ( 101.8468681455906903, 4.458734125000016313, 10.12500000136559208 ) ) ;
#6630 = VECTOR ( 'NONE', #20480, 1000.000000000000000 ) ;
#6631 = ORIENTED_EDGE ( 'NONE', *, *, #9856, .F. ) ;
#6632 = CARTESIAN_POINT ( 'NONE',  ( 101.7677669529663547, 123.0000000021849615, 1.767766952966350891 ) ) ;
#6633 = CARTESIAN_POINT ( 'NONE',  ( 95.54126587499996504, 1.387778780781445676E-14, 13.43750000136559386 ) ) ;
#6634 = FACE_OUTER_BOUND ( 'NONE', #21300, .T. ) ;
#6635 = CARTESIAN_POINT ( 'NONE',  ( 5.444914386472302859, 38.42031250108393436, 13.14518615778179189 ) ) ;
#6636 = CARTESIAN_POINT ( 'NONE',  ( 92.99999999999998579, 110.0000000000000000, -145.0000000000000284 ) ) ;
#6637 = DIRECTION ( 'NONE',  ( -0.000000000000000000, 1.000000000000000000, -0.000000000000000000 ) ) ;
#6638 = CARTESIAN_POINT ( 'NONE',  ( 74.29505027212704249, 33.90585937608393863, 9.295050272127046043 ) ) ;
#6639 = CARTESIAN_POINT ( 'NONE',  ( 91.91746824999998466, 107.3738262389971538, -49.02500000273119696 ) ) ;
#6640 = CARTESIAN_POINT ( 'NONE',  ( -8.049105076161786076E-16, 36.38632812608393152, -13.14518615778179544 ) ) ;
#6641 = CARTESIAN_POINT ( 'NONE',  ( 107.0000000000000142, 110.0000000000000000, -49.00000000000000711 ) ) ;
#6642 = CARTESIAN_POINT ( 'NONE',  ( 120.4011555911795455, 36.33671874999999574, 9.598844408820459861 ) ) ;
#6643 = CARTESIAN_POINT ( 'NONE',  ( 116.4251840539369596, 38.61874999999999147, 0.000000000000000000 ) ) ;
#6644 = VERTEX_POINT ( 'NONE', #24600 ) ;
#6645 = CARTESIAN_POINT ( 'NONE',  ( 103.5355339059327093, -3.535533905932726206, 8.375000000000000000 ) ) ;
#6646 = CARTESIAN_POINT ( 'NONE',  ( 13.14518615778179900, 38.02343750108395426, -5.444914386472297529 ) ) ;
#6647 = CARTESIAN_POINT ( 'NONE',  ( 13.57481594606304931, 38.27148437716787299, 5.622872871577869525 ) ) ;
#6648 = CARTESIAN_POINT ( 'NONE',  ( 135.4449143864723055, 37.13046875108393152, -13.14518615778179900 ) ) ;
#6649 = CARTESIAN_POINT ( 'NONE',  ( 51.42518405393695957, 34.74921875216787726, 0.000000000000000000 ) ) ;
#6650 = ORIENTED_EDGE ( 'NONE', *, *, #18893, .T. ) ;
#6651 = FACE_OUTER_BOUND ( 'NONE', #342, .T. ) ;
#6652 = CARTESIAN_POINT ( 'NONE',  ( -5.622872871577873077, 32.21914062716787441, -13.57481594606304753 ) ) ;
#6653 = CARTESIAN_POINT ( 'NONE',  ( 96.46446609406721961, 3.535533905932755072, 5.875000000000000000 ) ) ;
#6654 = CARTESIAN_POINT ( 'NONE',  ( 93.46109445667489979, 105.2492070361643215, -47.67499999726882720 ) ) ;
#6655 = CARTESIAN_POINT ( 'NONE',  ( 189.5550856135277229, 35.64218750108392442, -13.14518615778179900 ) ) ;
#6656 = FACE_OUTER_BOUND ( 'NONE', #18420, .T. ) ;
#6657 = CARTESIAN_POINT ( 'NONE',  ( 2.493653234604083739E-15, 34.15390625216787157, 13.57481594606304576 ) ) ;
#6659 = ORIENTED_EDGE ( 'NONE', *, *, #14238, .F. ) ;
#6658 = LINE ( 'NONE', #22494, #11409 ) ;
#6660 = EDGE_CURVE ( 'NONE', #17678, #2842, #2112, .T. ) ;
#6661 = DIRECTION ( 'NONE',  ( -0.000000000000000000, 1.000000000000000000, -0.000000000000000000 ) ) ;
#6662 = CARTESIAN_POINT ( 'NONE',  ( -13.57481594606304753, 32.31835937716787299, -5.622872871577872189 ) ) ;
#6663 = CARTESIAN_POINT ( 'NONE',  ( 5.622872871577878406, 38.86679687499999858, 13.57481594606304576 ) ) ;
#6664 = DIRECTION ( 'NONE',  ( 0.000000000000000000, 0.000000000000000000, 1.000000000000000000 ) ) ;
#6665 = CARTESIAN_POINT ( 'NONE',  ( -9.295050272127046043, 39.06523437608392868, -9.295050272127046043 ) ) ;
#6666 = CARTESIAN_POINT ( 'NONE',  ( -9.295050272127044266, 35.89023437608393152, 9.295050272127047819 ) ) ;
#6667 = CARTESIAN_POINT ( 'NONE',  ( 189.3771271284221314, 34.79882812499998579, 13.57481594606304753 ) ) ;
#6668 = CARTESIAN_POINT ( 'NONE',  ( 105.0000000000000000, 110.0000000000000000, 15.00099999999999412 ) ) ;
#6669 = CARTESIAN_POINT ( 'NONE',  ( 130.0000000000000000, 36.83281249999999574, -13.57481594606304576 ) ) ;
#6670 = CARTESIAN_POINT ( 'NONE',  ( 51.85481384221820633, 34.20351562608393436, 0.000000000000000000 ) ) ;
#6671 = CARTESIAN_POINT ( 'NONE',  ( 104.4587341249999781, -1.846868145590721655, 2.875000001365592528 ) ) ;
#6672 = FACE_OUTER_BOUND ( 'NONE', #20087, .T. ) ;
#6673 = CARTESIAN_POINT ( 'NONE',  ( 96.84719886470463734, 91.68749999863440792, -3.152801135295366208 ) ) ;
#6674 = CARTESIAN_POINT ( 'NONE',  ( -13.57481594606304753, 35.39414062499999147, -5.622872871577873077 ) ) ;
#6675 = CARTESIAN_POINT ( 'NONE',  ( 124.5550856135277087, 36.63437500108393152, -13.14518615778179900 ) ) ;
#6676 = ORIENTED_EDGE ( 'NONE', *, *, #5320, .T. ) ;
#6677 = ORIENTED_EDGE ( 'NONE', *, *, #5495, .F. ) ;
#6678 = CARTESIAN_POINT ( 'NONE',  ( 102.0710678118654329, 84.68750000000001421, -5.000000000000018652 ) ) ;
#6679 = CARTESIAN_POINT ( 'NONE',  ( 102.0710678118654329, 80.81250000273119838, -5.000000000000018652 ) ) ;
#6680 = CARTESIAN_POINT ( 'NONE',  ( 104.4587341249999923, 92.24999999863439371, 1.846868145590726318 ) ) ;
#6681 = CARTESIAN_POINT ( 'NONE',  ( 54.45404289489643190, 35.99999999999996447, -8.172591786207583198 ) ) ;
#6682 = EDGE_CURVE ( 'NONE', #15854, #12047, #19837, .T. ) ;
#6683 = CARTESIAN_POINT ( 'NONE',  ( 107.0000000000000000, 110.0000000000000000, -52.00000000000001421 ) ) ;
#6684 = CARTESIAN_POINT ( 'NONE',  ( 78.14518615778179367, 34.84843750108393579, -5.444914386472297529 ) ) ;
#6685 = ORIENTED_EDGE ( 'NONE', *, *, #26223, .F. ) ;
#6686 = CARTESIAN_POINT ( 'NONE',  ( 95.00000000000000000, 95.43749999726878741, 2.071067811865463959 ) ) ;
#6687 = CARTESIAN_POINT ( 'NONE',  ( 95.54126587499996504, 1.387778780781445676E-14, 4.687500001365592084 ) ) ;
#6688 = ORIENTED_EDGE ( 'NONE', *, *, #16115, .F. ) ;
#6689 = CARTESIAN_POINT ( 'NONE',  ( -8.049105076161786076E-16, 31.62382812608393579, -13.14518615778179544 ) ) ;
#6690 = CARTESIAN_POINT ( 'NONE',  ( 208.5748159460630688, 34.35234375216787583, -1.662435489736055892E-15 ) ) ;
#6691 = EDGE_CURVE ( 'NONE', #11663, #1369, #23005, .T. ) ;
#6692 = CARTESIAN_POINT ( 'NONE',  ( -5.444914386472297529, 34.84843750108393579, -13.14518615778179722 ) ) ;
#6693 = CARTESIAN_POINT ( 'NONE',  ( -9.598844408820458085, 40.90078124999999432, -9.598844408820458085 ) ) ;
#6694 = CARTESIAN_POINT ( 'NONE',  ( 195.0000000000000000, 40.10703125216787157, -13.57481594606304576 ) ) ;
#6695 = ORIENTED_EDGE ( 'NONE', *, *, #26955, .F. ) ;
#6696 = CARTESIAN_POINT ( 'NONE',  ( -9.295050272127046043, 39.06523437608392868, -9.295050272127046043 ) ) ;
#6697 = EDGE_CURVE ( 'NONE', #499, #1922, #22610, .T. ) ;
#6698 = CARTESIAN_POINT ( 'NONE',  ( 120.7049497278729575, 35.09648437608392868, 9.295050272127047819 ) ) ;
#6699 = CARTESIAN_POINT ( 'NONE',  ( 59.37712712842213136, 34.50117187499999005, -13.57481594606304753 ) ) ;
#6700 = CARTESIAN_POINT ( 'NONE',  ( 13.57481594606304576, 38.32109375216786873, -1.662435489736055892E-15 ) ) ;
#6701 = EDGE_CURVE ( 'NONE', #19839, #21429, #23027, .T. ) ;
#6702 = CARTESIAN_POINT ( 'NONE',  ( 98.15313185440925281, -4.458734124999987891, 12.87500000136559208 ) ) ;
#6703 = CARTESIAN_POINT ( 'NONE',  ( 189.3771271284221882, 37.18007812499999432, 13.57481594606311504 ) ) ;
#6704 = CARTESIAN_POINT ( 'NONE',  ( 99.99999999999995737, 4.458734125000016313, 14.18750000136559208 ) ) ;
#6705 = DIRECTION ( 'NONE',  ( -0.000000000000000000, -1.000000000000000000, -0.000000000000000000 ) ) ;
#6706 = CARTESIAN_POINT ( 'NONE',  ( 99.99999999999995737, -4.458734124999988779, 0.9375000013655925279 ) ) ;
#6707 = VECTOR ( 'NONE', #24443, 1000.000000000000000 ) ;
#6708 = CIRCLE ( 'NONE', #26296, 3.000000000000004441 ) ;
#6709 = CARTESIAN_POINT ( 'NONE',  ( 130.0000000000000000, 37.62656249999999858, -13.57481594606304576 ) ) ;
#6710 = CARTESIAN_POINT ( 'NONE',  ( 91.91746824999997045, 107.3738262389971680, -47.52499999726881441 ) ) ;
#6711 = CARTESIAN_POINT ( 'NONE',  ( -13.14518615778179900, 35.14609375108393152, -5.444914386472297529 ) ) ;
#6712 = EDGE_CURVE ( 'NONE', #7853, #7171, #15784, .T. ) ;
#6713 = CARTESIAN_POINT ( 'NONE',  ( 99.99999999999997158, 101.5015231886685854, -51.37499999726882294 ) ) ;
#6714 = ORIENTED_EDGE ( 'NONE', *, *, #26414, .T. ) ;
#6715 = DIRECTION ( 'NONE',  ( -0.000000000000000000, -0.000000000000000000, -1.000000000000000000 ) ) ;
#6716 =( BOUNDED_CURVE ( )  B_SPLINE_CURVE ( 2, ( #17765, #6922, #8650, #17338, #24318, #13034, #4804, #26034, #15326 ),
 .UNSPECIFIED., .F., .T. ) 
 B_SPLINE_CURVE_WITH_KNOTS ( ( 3, 2, 2, 2, 3 ),
 ( 0.6500000000000005773, 0.6750000000000005995, 0.7000000000000006217, 0.7250000000000006439, 0.7500000000000006661 ),
 .UNSPECIFIED. ) 
 CURVE ( )  GEOMETRIC_REPRESENTATION_ITEM ( )  RATIONAL_B_SPLINE_CURVE ( ( 0.9999999999999983347, 0.9238795325112884038, 1.000000000000000000, 0.9238795325112867385, 1.000000000000000000, 0.9238795325112867385, 1.000000000000000000, 0.9238795325112847401, 1.000000000000001998 ) ) 
 REPRESENTATION_ITEM ( '' )  );
#6717 = CARTESIAN_POINT ( 'NONE',  ( 114.9999999999999858, 125.0000000000000000, -15.00000000000001066 ) ) ;
#6718 = PLANE ( 'NONE',  #17949 ) ;
#6719 = CARTESIAN_POINT ( 'NONE',  ( 181.8548138422182205, 40.55351562608393579, 0.000000000000000000 ) ) ;
#6720 = ORIENTED_EDGE ( 'NONE', *, *, #802, .T. ) ;
#6721 = CARTESIAN_POINT ( 'NONE',  ( 51.90409344636400846, 35.99999999999999289, 1.137167824541468031 ) ) ;
#6722 = CARTESIAN_POINT ( 'NONE',  ( 99.99999999999995737, 85.00000000000000000, 4.999999999999990230 ) ) ;
#6723 = CARTESIAN_POINT ( 'NONE',  ( 101.8468681455906903, -4.458734124999987891, 14.00000000136559208 ) ) ;
#6724 = VERTEX_POINT ( 'NONE', #25022 ) ;
#6725 = CARTESIAN_POINT ( 'NONE',  ( 99.99999999999998579, 117.3602355696678501, -50.49999999999999289 ) ) ;
#6726 = CARTESIAN_POINT ( 'NONE',  ( -9.295050272127046043, 38.86679687608393863, -9.295050272127046043 ) ) ;
#6727 = CARTESIAN_POINT ( 'NONE',  ( 102.0669872999999939, 124.3000000010924566, 0.8561741729129311862 ) ) ;
#6728 = VECTOR ( 'NONE', #22651, 1000.000000000000000 ) ;
#6729 = ADVANCED_FACE ( 'NONE', ( #5503 ), #3354, .F. ) ;
#6730 = CARTESIAN_POINT ( 'NONE',  ( 135.6228728715778971, 32.61601562716786873, 13.57481594606304576 ) ) ;
#6731 = CARTESIAN_POINT ( 'NONE',  ( 195.0000000000000000, 38.91640625216786731, 13.57481594606304576 ) ) ;
#6732 = CARTESIAN_POINT ( 'NONE',  ( 104.9999999999999716, 93.81249999726880162, 2.071067811865467956 ) ) ;
#6733 = CARTESIAN_POINT ( 'NONE',  ( 78.14518615778179367, 37.18007812608393436, -1.609821015232357215E-15 ) ) ;
#6734 = CARTESIAN_POINT ( 'NONE',  ( 13.57481594606304931, 37.37851562499999858, 5.622872871577868636 ) ) ;
#6735 = EDGE_CURVE ( 'NONE', #19811, #444, #713, .T. ) ;
#6736 = CARTESIAN_POINT ( 'NONE',  ( 189.5550856135277229, 35.84062500108394289, -13.14518615778179900 ) ) ;
#6737 = ORIENTED_EDGE ( 'NONE', *, *, #9118, .T. ) ;
#6738 = ORIENTED_EDGE ( 'NONE', *, *, #20293, .T. ) ;
#6739 = CARTESIAN_POINT ( 'NONE',  ( 9.295050272127047819, 39.46210937608393721, 9.295050272127046043 ) ) ;
#6740 = DIRECTION ( 'NONE',  ( 1.000000000000000000, 0.000000000000000000, 0.000000000000000000 ) ) ;
#6741 = CARTESIAN_POINT ( 'NONE',  ( 101.8468681455907046, 4.458734125000016313, 9.375000001365593860 ) ) ;
#6742 = CARTESIAN_POINT ( 'NONE',  ( 104.9999999999999716, 94.93750000000000000, 2.071067811865467956 ) ) ;
#6743 = CARTESIAN_POINT ( 'NONE',  ( 95.54126587499996504, 80.43750000136559208, -1.387778780781445676E-14 ) ) ;
#6744 = CARTESIAN_POINT ( 'NONE',  ( 208.1451861577818079, 40.20625000108393010, -5.444914386472297529 ) ) ;
#6745 = CARTESIAN_POINT ( 'NONE',  ( 2.414731522848535132E-15, 39.36289062608393152, 13.14518615778179544 ) ) ;
#6746 = CARTESIAN_POINT ( 'NONE',  ( -9.598844408820454532, 39.61093750216787868, 9.598844408820459861 ) ) ;
#6747 = CARTESIAN_POINT ( 'NONE',  ( -8.312177448680279460E-16, 36.93203125216787441, -13.57481594606304576 ) ) ;
#6748 = CARTESIAN_POINT ( 'NONE',  ( 78.57481594606305464, 39.85898437499999858, -5.622872871577873966 ) ) ;
#6749 = CARTESIAN_POINT ( 'NONE',  ( 93.46109445667489979, 114.7507929638356785, -49.82499999726882578 ) ) ;
#6750 = AXIS2_PLACEMENT_3D ( 'NONE', #25302, #3926, #3361 ) ;
#6751 = AXIS2_PLACEMENT_3D ( 'NONE', #6212, #17451, #4079 ) ;
#6752 = ORIENTED_EDGE ( 'NONE', *, *, #8600, .F. ) ;
#6753 = CARTESIAN_POINT ( 'NONE',  ( -13.57481594606304576, 36.28710937499999289, 5.622872871577880183 ) ) ;
#6754 = CARTESIAN_POINT ( 'NONE',  ( 13.14518615778179900, 38.61875000108393152, -5.444914386472297529 ) ) ;
#6755 = AXIS2_PLACEMENT_3D ( 'NONE', #4684, #7083, #7367 ) ;
#6756 = ORIENTED_EDGE ( 'NONE', *, *, #1361, .F. ) ;
#6757 = CARTESIAN_POINT ( 'NONE',  ( 143.1451861577818079, 37.22968750108393721, -5.444914386472297529 ) ) ;
#6758 = CARTESIAN_POINT ( 'NONE',  ( 51.85481384221819923, 33.36015625108393579, -5.444914386472297529 ) ) ;
#6759 = CARTESIAN_POINT ( 'NONE',  ( 189.5550856135277229, 38.22187500108393010, -13.14518615778179900 ) ) ;
#6760 =( BOUNDED_CURVE ( )  B_SPLINE_CURVE ( 2, ( #18456, #7614, #25007, #16441, #14434, #7890, #3341, #12425, #21143 ),
 .UNSPECIFIED., .F., .F. ) 
 B_SPLINE_CURVE_WITH_KNOTS ( ( 3, 2, 2, 2, 3 ),
 ( 0.7708333333333333703, 0.7812500000000000000, 0.7916666666666665186, 0.8020833333333332593, 0.8124999999999998890 ),
 .UNSPECIFIED. ) 
 CURVE ( )  GEOMETRIC_REPRESENTATION_ITEM ( )  RATIONAL_B_SPLINE_CURVE ( ( 1.000000000000000000, 0.9238795325112867385, 1.000000000000000000, 0.9238795325112867385, 1.000000000000000000, 0.9238795325112867385, 1.000000000000000000, 0.9238795325112875156, 0.9999999999999992228 ) ) 
 REPRESENTATION_ITEM ( '' )  );
#6761 = ORIENTED_EDGE ( 'NONE', *, *, #10331, .T. ) ;
#6762 = CARTESIAN_POINT ( 'NONE',  ( 2.493653234604083739E-15, 37.32890625216786873, 13.57481594606304576 ) ) ;
#6763 = CARTESIAN_POINT ( 'NONE',  ( 13.14518615778179900, 33.85625000108393579, -5.444914386472297529 ) ) ;
#6764 = CARTESIAN_POINT ( 'NONE',  ( 137.6362410679823540, 54.91786508990713855, -15.00000000000000355 ) ) ;
#6765 = CARTESIAN_POINT ( 'NONE',  ( 9.598844408820456309, 39.11484374999999858, -9.598844408820458085 ) ) ;
#6766 = CARTESIAN_POINT ( 'NONE',  ( 116.4251840539369596, 39.51171875216787299, 0.000000000000000000 ) ) ;
#6767 = CARTESIAN_POINT ( 'NONE',  ( 106.5389055433251002, 114.7507929638356785, -53.92500000273119554 ) ) ;
#6768 = CYLINDRICAL_SURFACE ( 'NONE', #26517, 5.000000000000004441 ) ;
#6769 = CARTESIAN_POINT ( 'NONE',  ( 98.23223304703363112, 122.8000000021849587, 1.767766952966351557 ) ) ;
#6770 = ORIENTED_EDGE ( 'NONE', *, *, #4109, .F. ) ;
#6771 = STYLED_ITEM ( 'NONE', ( #3077 ), #15807 ) ;
#6772 = CARTESIAN_POINT ( 'NONE',  ( 101.8468681455906903, -4.458734124999987891, 10.75000000136559208 ) ) ;
#6773 = CARTESIAN_POINT ( 'NONE',  ( 99.99999999999998579, 123.3000000021849587, -2.499999999999997780 ) ) ;
#6774 = CARTESIAN_POINT ( 'NONE',  ( 104.4587341249999781, 1.846868145590750299, 13.00000000136559386 ) ) ;
#6775 = CARTESIAN_POINT ( 'NONE',  ( 131.5054921815522277, 53.60078691996476863, 14.99999999999996447 ) ) ;
#6776 = AXIS2_PLACEMENT_3D ( 'NONE', #7774, #14033, #3503 ) ;
#6777 = CARTESIAN_POINT ( 'NONE',  ( 5.444914386472297529, 37.92421875108392726, -13.14518615778179900 ) ) ;
#6778 = FACE_OUTER_BOUND ( 'NONE', #8601, .T. ) ;
#6779 = CARTESIAN_POINT ( 'NONE',  ( 104.4587341249999639, 80.18750000136559208, -1.442382525525748735E-14 ) ) ;
#6780 = CARTESIAN_POINT ( 'NONE',  ( 65.00000000000000000, 34.20351562608394147, -13.14518615778179544 ) ) ;
#6781 = CARTESIAN_POINT ( 'NONE',  ( 95.00472066334982912, 116.8754121666685393, -53.42500000273118843 ) ) ;
#6782 = CARTESIAN_POINT ( 'NONE',  ( 9.295050272127047819, 37.67617187608393436, 9.295050272127046043 ) ) ;
#6783 = CARTESIAN_POINT ( 'NONE',  ( 2.493653234604083739E-15, 39.61093749999999147, 13.57481594606304576 ) ) ;
#6784 = CARTESIAN_POINT ( 'NONE',  ( 96.46446609406721961, -3.535533905932727539, 11.25000000273118594 ) ) ;
#6785 = CARTESIAN_POINT ( 'NONE',  ( 135.6228728715779823, 40.75195312499999289, -13.57481594606294095 ) ) ;
#6786 = CARTESIAN_POINT ( 'NONE',  ( 143.5748159460630404, 38.27148437500000711, -5.622872871577873077 ) ) ;
#6787 = ORIENTED_EDGE ( 'NONE', *, *, #7622, .T. ) ;
#6788 = LINE ( 'NONE', #19486, #19093 ) ;
#6789 = CARTESIAN_POINT ( 'NONE',  ( 13.14518615778179544, 36.38632812608393863, -1.609821015232357215E-15 ) ) ;
#6790 = CARTESIAN_POINT ( 'NONE',  ( 13.57481594606304753, 35.98945312716787015, -5.622872871577873077 ) ) ;
#6791 = CARTESIAN_POINT ( 'NONE',  ( 96.46446609406721961, 3.535533905932755072, 9.000000002731184168 ) ) ;
#6792 = CARTESIAN_POINT ( 'NONE',  ( 130.0000000000000000, 36.78320312608393294, 13.14518615778179544 ) ) ;
#6793 = CARTESIAN_POINT ( 'NONE',  ( 65.00000000000000000, 33.75703125216787726, -13.57481594606304576 ) ) ;
#6794 = CARTESIAN_POINT ( 'NONE',  ( 12.00957333851164854, 36.00000000000000000, 5.901833544881618820 ) ) ;
#6795 = CARTESIAN_POINT ( 'NONE',  ( 2.493653234604083739E-15, 31.77265625216787370, 13.57481594606304576 ) ) ;
#6796 = AXIS2_PLACEMENT_3D ( 'NONE', #10354, #14224, #14500 ) ;
#6797 = CARTESIAN_POINT ( 'NONE',  ( 103.5355339059327093, 3.535533905932755072, 1.624999999999999778 ) ) ;
#6798 = CARTESIAN_POINT ( 'NONE',  ( 106.5389055433250860, 105.2492070361643215, -47.07499999726882578 ) ) ;
#6799 = CARTESIAN_POINT ( 'NONE',  ( 204.2950502721270425, 34.69960937608393436, -9.295050272127046043 ) ) ;
#6800 = CYLINDRICAL_SURFACE ( 'NONE', #9274, 5.000000000000000888 ) ;
#6801 = AXIS2_PLACEMENT_3D ( 'NONE', #3250, #27206, #22492 ) ;
#6802 = CARTESIAN_POINT ( 'NONE',  ( 84.99999999999998579, 100.0000000000000000, -15.00000000000000533 ) ) ;
#6804 = ORIENTED_EDGE ( 'NONE', *, *, #24079, .F. ) ;
#6803 = CARTESIAN_POINT ( 'NONE',  ( 195.0000000000000000, 40.40468749999999432, 13.57481594606304576 ) ) ;
#6805 = DIRECTION ( 'NONE',  ( 0.000000000000000000, -1.000000000000000000, 0.000000000000000000 ) ) ;
#6806 = CARTESIAN_POINT ( 'NONE',  ( 135.3173515774758187, 54.47013368152368429, 14.99999999999996092 ) ) ;
#6807 = CARTESIAN_POINT ( 'NONE',  ( -5.622872871577873077, 37.18007812500000853, 13.57481594606304753 ) ) ;
#6808 = CARTESIAN_POINT ( 'NONE',  ( -1.816500417285228597, 36.00000000000000711, -13.35830014193482285 ) ) ;
#6809 = CARTESIAN_POINT ( 'NONE',  ( 5.444914386472302859, 38.61875000108393152, 13.14518615778179189 ) ) ;
#6810 = CARTESIAN_POINT ( 'NONE',  ( 13.14518615778179900, 36.13828125108393863, 5.444914386472293977 ) ) ;
#6811 = CARTESIAN_POINT ( 'NONE',  ( 181.4251840539369596, 35.44374999999999432, 0.000000000000000000 ) ) ;
#6812 = LINE ( 'NONE', #23928, #12188 ) ;
#6813 = CARTESIAN_POINT ( 'NONE',  ( 0.000000000000000000, 40.99999999999999289, 0.000000000000000000 ) ) ;
#6814 = CARTESIAN_POINT ( 'NONE',  ( 78.14518615778179367, 36.98164062608393010, -1.609821015232357215E-15 ) ) ;
#6815 = CARTESIAN_POINT ( 'NONE',  ( 101.8468681455907046, 4.458734125000016313, 1.125000001365592750 ) ) ;
#6816 = CARTESIAN_POINT ( 'NONE',  ( 100.1038569895340657, 123.0000000000000284, 2.502009621290390839 ) ) ;
#6817 = ORIENTED_EDGE ( 'NONE', *, *, #26815, .F. ) ;
#6818 = CARTESIAN_POINT ( 'NONE',  ( 102.0710678118654329, 5.000000000000018652, 4.687500000000000000 ) ) ;
#6819 = CARTESIAN_POINT ( 'NONE',  ( -13.57481594606304576, 36.28710937499999289, 5.622872871577880183 ) ) ;
#6820 = CARTESIAN_POINT ( 'NONE',  ( 130.0000000000000000, 36.18789062608393436, 13.14518615778179544 ) ) ;
#6821 = ORIENTED_EDGE ( 'NONE', *, *, #21889, .F. ) ;
#6822 = CARTESIAN_POINT ( 'NONE',  ( 104.9999999999999574, 84.43750000000002842, 2.071067811865462627 ) ) ;
#6823 = AXIS2_PLACEMENT_3D ( 'NONE', #28141, #1647, #19163 ) ;
#6824 = EDGE_CURVE ( 'NONE', #12157, #8417, #18926, .T. ) ;
#6825 = CARTESIAN_POINT ( 'NONE',  ( 103.5355339059327093, 82.50000000273119838, 3.535533905932726206 ) ) ;
#6826 = CARTESIAN_POINT ( 'NONE',  ( 95.54126587500000767, 92.81249999863440792, -7.484931351350258973E-15 ) ) ;
#6827 = CARTESIAN_POINT ( 'NONE',  ( 95.54126587500000767, 95.06249999863440792, -7.484931351350258973E-15 ) ) ;
#6828 = CARTESIAN_POINT ( 'NONE',  ( 97.83688103937535629, 116.6573956140660897, -47.40000000000001279 ) ) ;
#6829 = CARTESIAN_POINT ( 'NONE',  ( 55.40115559117954547, 40.90078124999999432, -9.598844408820458085 ) ) ;
#6830 = ORIENTED_EDGE ( 'NONE', *, *, #19411, .F. ) ;
#6831 = DIRECTION ( 'NONE',  ( 0.000000000000000000, 1.000000000000000000, 0.000000000000000000 ) ) ;
#6832 = CARTESIAN_POINT ( 'NONE',  ( 103.5355339059327093, -3.535533905932726206, 12.37499999999999822 ) ) ;
#6833 = ORIENTED_EDGE ( 'NONE', *, *, #13516, .T. ) ;
#6834 = CARTESIAN_POINT ( 'NONE',  ( 5.444914386472302859, 33.85625000108393579, 13.14518615778179189 ) ) ;
#6835 = CARTESIAN_POINT ( 'NONE',  ( 13.14518615778179900, 40.40468750108393436, -5.444914386472297529 ) ) ;
#6836 = CARTESIAN_POINT ( 'NONE',  ( 204.5988444088204403, 33.65781250216787157, -9.598844408820458085 ) ) ;
#6837 = CARTESIAN_POINT ( 'NONE',  ( 13.14518615778179544, 35.39414062608393152, -1.609821015232357215E-15 ) ) ;
#6838 = DIRECTION ( 'NONE',  ( 0.000000000000000000, 1.000000000000000000, 0.000000000000000000 ) ) ;
#6839 = CARTESIAN_POINT ( 'NONE',  ( 120.7049497278729575, 37.67617187608393436, 9.295050272127047819 ) ) ;
#6841 = VECTOR ( 'NONE', #17538, 1000.000000000000000 ) ;
#6840 = CARTESIAN_POINT ( 'NONE',  ( -8.049105076161786076E-16, 34.99726562608393721, -13.14518615778179544 ) ) ;
#6842 = CARTESIAN_POINT ( 'NONE',  ( 116.8548138422182205, 34.99726562608393721, 0.000000000000000000 ) ) ;
#6843 = CARTESIAN_POINT ( 'NONE',  ( 51.42518405393695957, 33.90585937500000568, 5.622872871577880183 ) ) ;
#6844 = CARTESIAN_POINT ( 'NONE',  ( 130.0000000000000000, -7.395377635281828788, -1.503427012513233026E-14 ) ) ;
#6845 = CARTESIAN_POINT ( 'NONE',  ( 95.54126587499995082, -1.846868145590724986, 11.75000000136559208 ) ) ;
#6846 = CARTESIAN_POINT ( 'NONE',  ( 208.4064236467344813, 36.00000000000002132, 1.227293221035586912 ) ) ;
#6847 = EDGE_CURVE ( 'NONE', #15313, #8172, #15721, .T. ) ;
#6848 = CARTESIAN_POINT ( 'NONE',  ( 96.84719886470459471, -3.152801135295355994, 12.56250000136559208 ) ) ;
#6849 = CARTESIAN_POINT ( 'NONE',  ( 105.6631189606246295, 114.1144967660473242, -53.30000000546237970 ) ) ;
#6850 = CARTESIAN_POINT ( 'NONE',  ( 74.18017581364799184, 55.00000000000000000, 9.999999999999978684 ) ) ;
#6851 = FACE_OUTER_BOUND ( 'NONE', #10998, .T. ) ;
#6852 = CARTESIAN_POINT ( 'NONE',  ( 91.91746824999998466, 110.0000000000000000, -47.62499999726882294 ) ) ;
#6853 = CARTESIAN_POINT ( 'NONE',  ( -5.444914386472299306, 36.93203125108394147, 13.14518615778179722 ) ) ;
#6854 = CARTESIAN_POINT ( 'NONE',  ( 108.0825317499999869, 112.6261737610028320, -52.77499999726883573 ) ) ;
#6855 = ORIENTED_EDGE ( 'NONE', *, *, #22226, .F. ) ;
#6856 = CARTESIAN_POINT ( 'NONE',  ( 99.99999999999998579, 124.5500000010924708, -2.066987299999998751 ) ) ;
#6858 = EDGE_CURVE ( 'NONE', #19690, #3877, #14999, .T. ) ;
#6857 = CARTESIAN_POINT ( 'NONE',  ( 103.5355339059327093, -3.535533905932726206, 12.50000000273118594 ) ) ;
#6859 = DIRECTION ( 'NONE',  ( -0.000000000000000000, -1.000000000000000000, -0.000000000000000000 ) ) ;
#6860 = CIRCLE ( 'NONE', #15974, 9.000000000000007105 ) ;
#6861 = ADVANCED_FACE ( 'NONE', ( #12435 ), #10163, .T. ) ;
#6862 = CARTESIAN_POINT ( 'NONE',  ( 189.5550856135277229, 38.32109375108394289, 13.14518615778179722 ) ) ;
#6863 = ORIENTED_EDGE ( 'NONE', *, *, #15915, .T. ) ;
#6864 = CARTESIAN_POINT ( 'NONE',  ( 100.0000000000000000, 110.0000000000000000, -55.00000000000000711 ) ) ;
#6865 = EDGE_CURVE ( 'NONE', #19382, #22143, #3640, .T. ) ;
#6866 = CARTESIAN_POINT ( 'NONE',  ( 94.33688103937534208, 114.1144967660473242, -48.69999999453764161 ) ) ;
#6867 = CARTESIAN_POINT ( 'NONE',  ( 99.99999999999995737, -4.458734124999988779, 12.93750000136559208 ) ) ;
#6868 = ORIENTED_EDGE ( 'NONE', *, *, #2814, .F. ) ;
#6869 = CARTESIAN_POINT ( 'NONE',  ( 107.0000000000000142, 112.2744378736303332, -46.90000000000001279 ) ) ;
#6870 = AXIS2_PLACEMENT_3D ( 'NONE', #14683, #16706, #3461 ) ;
#6871 = CARTESIAN_POINT ( 'NONE',  ( -5.444914386472297529, 40.40468750108393436, -13.14518615778179900 ) ) ;
#6872 = CARTESIAN_POINT ( 'NONE',  ( 0.000000000000000000, 20.00000000000000000, 25.00000000000000711 ) ) ;
#6873 = EDGE_CURVE ( 'NONE', #4508, #23121, #14862, .T. ) ;
#6874 = CARTESIAN_POINT ( 'NONE',  ( 130.0000000000000000, 32.56640625216787299, 13.57481594606304576 ) ) ;
#6875 = DIRECTION ( 'NONE',  ( 5.782411586589358625E-17, -0.000000000000000000, 1.000000000000000000 ) ) ;
#6876 = CARTESIAN_POINT ( 'NONE',  ( 104.9999999999999716, 92.81249999726880162, 2.071067811865467956 ) ) ;
#6877 = CARTESIAN_POINT ( 'NONE',  ( 59.55508561352770158, 37.42812500108394147, -13.14518615778179900 ) ) ;
#6878 = CARTESIAN_POINT ( 'NONE',  ( 71.90237857378353681, 51.13402819306926972, -15.00000000000000178 ) ) ;
#6879 = CARTESIAN_POINT ( 'NONE',  ( 181.4251840539369596, 40.95039062499999005, -5.622872871577873077 ) ) ;
#6880 = SPHERICAL_SURFACE ( 'NONE', #10280, 5.000000000000000000 ) ;
#6881 = ORIENTED_EDGE ( 'NONE', *, *, #3086, .T. ) ;
#6882 = ORIENTED_EDGE ( 'NONE', *, *, #1003, .F. ) ;
#6883 = CARTESIAN_POINT ( 'NONE',  ( 13.14518615778179544, 40.35507812608393863, -1.609821015232357215E-15 ) ) ;
#6884 = CARTESIAN_POINT ( 'NONE',  ( 96.84719886470459471, -3.152801135295355994, 12.81250000136559208 ) ) ;
#6885 =( BOUNDED_CURVE ( )  B_SPLINE_CURVE ( 2, ( #68, #12728, #13140, #23862, #25999, #2065, #23727, #11149, #26139 ),
 .UNSPECIFIED., .F., .F. ) 
 B_SPLINE_CURVE_WITH_KNOTS ( ( 3, 2, 2, 2, 3 ),
 ( 0.3125000000000002220, 0.3229166666666668517, 0.3333333333333334259, 0.3437500000000000555, 0.3541666666666666852 ),
 .UNSPECIFIED. ) 
 CURVE ( )  GEOMETRIC_REPRESENTATION_ITEM ( )  RATIONAL_B_SPLINE_CURVE ( ( 0.9999999999999983347, 0.9238795325112884038, 1.000000000000000000, 0.9238795325112867385, 1.000000000000000000, 0.9238795325112867385, 1.000000000000000000, 0.9238795325112867385, 1.000000000000000000 ) ) 
 REPRESENTATION_ITEM ( '' )  );
#6886 = CARTESIAN_POINT ( 'NONE',  ( 78.14518615778180788, 40.10703125108393152, 5.444914386472293977 ) ) ;
#6887 = EDGE_CURVE ( 'NONE', #2879, #22694, #3917, .T. ) ;
#6888 = CARTESIAN_POINT ( 'NONE',  ( 104.4587341249999639, 81.93750000136559208, -1.442382525525748735E-14 ) ) ;
#6889 = CARTESIAN_POINT ( 'NONE',  ( 200.4449143864723055, 40.00781250108393294, 13.14518615778179189 ) ) ;
#6890 = CARTESIAN_POINT ( 'NONE',  ( -8.049105076161786076E-16, 38.17226562608394147, -13.14518615778179544 ) ) ;
#6891 = CARTESIAN_POINT ( 'NONE',  ( 103.1528011352953484, 90.68749999863440792, -3.152801135295366208 ) ) ;
#6892 = CARTESIAN_POINT ( 'NONE',  ( 200.4449143864723055, 38.91640625108393436, -13.14518615778179722 ) ) ;
#6893 = CARTESIAN_POINT ( 'NONE',  ( 106.5389055433250860, 114.7507929638356785, -50.42499999726882010 ) ) ;
#6894 = ORIENTED_EDGE ( 'NONE', *, *, #27480, .T. ) ;
#6895 = CARTESIAN_POINT ( 'NONE',  ( -5.622872871577873077, 35.59257812499999574, 13.57481594606304753 ) ) ;
#6896 = CARTESIAN_POINT ( 'NONE',  ( -9.295050272127044266, 37.47773437608393010, 9.295050272127047819 ) ) ;
#6897 = VERTEX_POINT ( 'NONE', #25437 ) ;
#6898 = CARTESIAN_POINT ( 'NONE',  ( 116.8548138422182205, 34.40195312608393152, 0.000000000000000000 ) ) ;
#6899 = CARTESIAN_POINT ( 'NONE',  ( 55.70494972787295751, 35.09648437608392868, 9.295050272127047819 ) ) ;
#6900 = EDGE_CURVE ( 'NONE', #22247, #25944, #22772, .T. ) ;
#6901 = CARTESIAN_POINT ( 'NONE',  ( 195.0000000000000000, 37.77539062608393294, 13.14518615778179544 ) ) ;
#6902 = ORIENTED_EDGE ( 'NONE', *, *, #15277, .T. ) ;
#6903 = CARTESIAN_POINT ( 'NONE',  ( 102.0669873000000081, 124.1000000010924822, 0.8561741729129311862 ) ) ;
#6904 = CARTESIAN_POINT ( 'NONE',  ( 181.8548138422182205, 40.75195312608393294, 0.000000000000000000 ) ) ;
#6905 = DIRECTION ( 'NONE',  ( 1.000000000000000000, 0.000000000000000000, 0.000000000000000000 ) ) ;
#6906 = CARTESIAN_POINT ( 'NONE',  ( 95.00472066334981491, 116.8754121666685393, -53.42500000273118843 ) ) ;
#6907 = ADVANCED_FACE ( 'NONE', ( #8854 ), #2028, .T. ) ;
#6908 = CARTESIAN_POINT ( 'NONE',  ( 94.99999999999995737, 1.387778780781445676E-14, 8.125000002731185944 ) ) ;
#6909 = DIRECTION ( 'NONE',  ( 0.000000000000000000, 0.000000000000000000, 1.000000000000000000 ) ) ;
#6910 = ORIENTED_EDGE ( 'NONE', *, *, #20818, .F. ) ;
#6911 = CARTESIAN_POINT ( 'NONE',  ( 95.54126587499995082, 1.846868145590750077, 6.375000001365592084 ) ) ;
#6912 = ORIENTED_EDGE ( 'NONE', *, *, #23294, .F. ) ;
#6913 = CARTESIAN_POINT ( 'NONE',  ( 100.8561741729129153, 123.5000000010924737, -2.066987299999999195 ) ) ;
#6914 = CARTESIAN_POINT ( 'NONE',  ( 99.99999999999995737, 4.458734125000016313, 7.187500001365592084 ) ) ;
#6915 = CARTESIAN_POINT ( 'NONE',  ( 1.662435489736055892E-15, 40.99999999999999289, 13.57481594606304576 ) ) ;
#6916 = CARTESIAN_POINT ( 'NONE',  ( -5.444914386472297529, 36.43593750108392726, -13.14518615778179900 ) ) ;
#6917 = CARTESIAN_POINT ( 'NONE',  ( 94.99999999999995737, 2.071067811865491493, 7.062500002731185056 ) ) ;
#6918 = CARTESIAN_POINT ( 'NONE',  ( 98.15313185440925281, 81.50000000136560629, -4.458734125000016313 ) ) ;
#6919 = CARTESIAN_POINT ( 'NONE',  ( 70.44491438647230552, 36.53515625108393294, -13.14518615778179900 ) ) ;
#6920 = CARTESIAN_POINT ( 'NONE',  ( 108.0825317500000153, 110.0000000000000000, -52.12500000273119838 ) ) ;
#6921 = CARTESIAN_POINT ( 'NONE',  ( 9.295050272127047819, 38.46992187608393010, 9.295050272127046043 ) ) ;
#6922 = CARTESIAN_POINT ( 'NONE',  ( 102.0710678118654755, 80.81250000273119838, -4.999999999999983125 ) ) ;
#6923 = CARTESIAN_POINT ( 'NONE',  ( 5.622872871577924592, 33.31054687499999289, 13.57481594606299957 ) ) ;
#6924 = CARTESIAN_POINT ( 'NONE',  ( 104.3262379212492448, 104.0454443415356991, -55.79999999453763593 ) ) ;
#6925 = CARTESIAN_POINT ( 'NONE',  ( 135.6228728715778971, 37.27929687499999289, 13.57481594606304576 ) ) ;
#6926 = VECTOR ( 'NONE', #27375, 1000.000000000000114 ) ;
#6927 = EDGE_CURVE ( 'NONE', #3337, #11248, #19368, .T. ) ;
#6928 = ORIENTED_EDGE ( 'NONE', *, *, #5500, .T. ) ;
#6929 = FACE_OUTER_BOUND ( 'NONE', #4631, .T. ) ;
#6930 =( BOUNDED_CURVE ( )  B_SPLINE_CURVE ( 2, ( #4787, #17889, #26596, #7042, #24445, #24733, #13594, #5213, #2790 ),
 .UNSPECIFIED., .F., .F. ) 
 B_SPLINE_CURVE_WITH_KNOTS ( ( 3, 2, 2, 2, 3 ),
 ( 0.4375000000000003331, 0.4479166666666669627, 0.4583333333333335369, 0.4687500000000001665, 0.4791666666666667962 ),
 .UNSPECIFIED. ) 
 CURVE ( )  GEOMETRIC_REPRESENTATION_ITEM ( )  RATIONAL_B_SPLINE_CURVE ( ( 0.9999999999999975575, 0.9238795325112891810, 1.000000000000000000, 0.9238795325112867385, 1.000000000000000000, 0.9238795325112867385, 1.000000000000000000, 0.9238795325112859613, 1.000000000000000888 ) ) 
 REPRESENTATION_ITEM ( '' )  );
#6931 = CARTESIAN_POINT ( 'NONE',  ( 5.444914386472297529, 37.32890625108393579, -13.14518615778179900 ) ) ;
#6932 = CARTESIAN_POINT ( 'NONE',  ( 5.622872871577878406, 36.58476562716787583, 13.57481594606304576 ) ) ;
#6933 = CARTESIAN_POINT ( 'NONE',  ( 94.99999999999995737, 1.387778780781445676E-14, 11.12500000273118594 ) ) ;
#6934 = CARTESIAN_POINT ( 'NONE',  ( 120.7049497278729575, 32.71523437608393436, 9.295050272127047819 ) ) ;
#6935 = CARTESIAN_POINT ( 'NONE',  ( 70.62287287157788285, 34.99726562716787726, 13.57481594606304576 ) ) ;
#6936 = CARTESIAN_POINT ( 'NONE',  ( 99.99999999999998579, 128.0000000000000000, -5.204170427930421283E-15 ) ) ;
#6937 = CARTESIAN_POINT ( 'NONE',  ( 13.57481594606304576, 33.55859375216787299, -1.662435489736055892E-15 ) ) ;
#6938 = CARTESIAN_POINT ( 'NONE',  ( 97.92893218813451028, 5.000000000000018652, 1.812500000000000000 ) ) ;
#6939 = CARTESIAN_POINT ( 'NONE',  ( 95.00472066334981491, 116.8754121666685393, -48.17499999726882010 ) ) ;
#6940 = CARTESIAN_POINT ( 'NONE',  ( -13.57481594606304753, 37.87460937716787868, -5.622872871577873077 ) ) ;
#6941 = CARTESIAN_POINT ( 'NONE',  ( 185.7049497278729575, 35.09648437608392868, 9.295050272127047819 ) ) ;
#6942 = FACE_OUTER_BOUND ( 'NONE', #26574, .T. ) ;
#6943 = CARTESIAN_POINT ( 'NONE',  ( 202.0894172723214126, 49.99999999943664619, 11.59823041029769541 ) ) ;
#6944 = AXIS2_PLACEMENT_3D ( 'NONE', #5550, #7377, #704 ) ;
#6945 = CARTESIAN_POINT ( 'NONE',  ( 103.5355339059327093, 81.37500000000000000, 3.535533905932726206 ) ) ;
#6946 = CARTESIAN_POINT ( 'NONE',  ( 208.5748159460630688, 38.96601562499999005, 5.622872871577868636 ) ) ;
#6947 = CARTESIAN_POINT ( 'NONE',  ( 96.46446609406721961, -3.535533905932727539, 10.25000000273118594 ) ) ;
#6948 = CARTESIAN_POINT ( 'NONE',  ( 51.42518405393695957, 40.30546875216787583, 0.000000000000000000 ) ) ;
#6949 = CARTESIAN_POINT ( 'NONE',  ( 5.622872871577871301, 37.57695312499998863, -13.57481594606304753 ) ) ;
#6950 = DIRECTION ( 'NONE',  ( 0.000000000000000000, 0.000000000000000000, -1.000000000000000000 ) ) ;
#6951 = CARTESIAN_POINT ( 'NONE',  ( 2.414731522848535132E-15, 33.80664062608393294, 13.14518615778179544 ) ) ;
#6952 = CARTESIAN_POINT ( 'NONE',  ( -5.444914386472299306, 36.73359375108393010, 13.14518615778179722 ) ) ;
#6953 = CARTESIAN_POINT ( 'NONE',  ( 189.3771271284221314, 35.59257812499999574, 13.57481594606304753 ) ) ;
#6954 = CARTESIAN_POINT ( 'NONE',  ( 99.99999999999998579, 101.5015231886685712, -46.87500000273119838 ) ) ;
#6955 = CARTESIAN_POINT ( 'NONE',  ( 135.6228728715778118, 36.48554687499999716, 13.57481594606309194 ) ) ;
#6956 = CARTESIAN_POINT ( 'NONE',  ( 55.70494972787295751, 36.68398437608392726, 9.295050272127047819 ) ) ;
#6957 = CARTESIAN_POINT ( 'NONE',  ( 95.54126587499996504, 1.846868145590750077, 1.375000001365592972 ) ) ;
#6958 = CARTESIAN_POINT ( 'NONE',  ( 100.3882422504498493, 123.0000000000000000, 2.474292135181528351 ) ) ;
#6959 = EDGE_LOOP ( 'NONE', ( #17524, #21105, #20037, #25056 ) ) ;
#6960 = CARTESIAN_POINT ( 'NONE',  ( 101.0355339059327093, 123.6500000000000057, 2.499999999999984457 ) ) ;
#6961 = CARTESIAN_POINT ( 'NONE',  ( 13.57481594606304931, 36.58476562499999574, 5.622872871577869525 ) ) ;
#6962 = CARTESIAN_POINT ( 'NONE',  ( 120.7049497278729575, 38.27148437608393294, -9.295050272127046043 ) ) ;
#6963 = VERTEX_POINT ( 'NONE', #25963 ) ;
#6964 = CARTESIAN_POINT ( 'NONE',  ( 103.5355339059327093, 81.37500000000000000, 3.535533905932726206 ) ) ;
#6965 = CARTESIAN_POINT ( 'NONE',  ( 98.21999331106005116, 123.0000000000000426, 1.143679003824301876 ) ) ;
#6966 = CARTESIAN_POINT ( 'NONE',  ( 104.9999999999999574, 80.56250000273119838, 2.071067811865462627 ) ) ;
#6967 = CARTESIAN_POINT ( 'NONE',  ( 103.1528011352953484, 94.18749999863440792, 3.152801135295352886 ) ) ;
#6968 = CARTESIAN_POINT ( 'NONE',  ( 5.622872871577780707, 34.40195312499999858, -13.57481594606313990 ) ) ;
#6969 = CIRCLE ( 'NONE', #12404, 11.57481594606304576 ) ;
#6970 = CARTESIAN_POINT ( 'NONE',  ( 94.33688103937535629, 105.8855032339526758, -46.80000000000001847 ) ) ;
#6971 = CARTESIAN_POINT ( 'NONE',  ( 51.42518405393695957, 40.95039062499999005, -5.622872871577873077 ) ) ;
#6972 = ORIENTED_EDGE ( 'NONE', *, *, #8464, .F. ) ;
#6973 = DIRECTION ( 'NONE',  ( 0.000000000000000000, 0.000000000000000000, -1.000000000000000000 ) ) ;
#6974 = CARTESIAN_POINT ( 'NONE',  ( 103.5355339059327093, -3.535533905932726206, 14.37499999999999822 ) ) ;
#6975 = VERTEX_POINT ( 'NONE', #313 ) ;
#6976 = CARTESIAN_POINT ( 'NONE',  ( -13.14518615778179189, 36.83281250108393579, 5.444914386472304635 ) ) ;
#6977 = CARTESIAN_POINT ( 'NONE',  ( 200.6228728715778686, 33.70742187716787441, -13.57481594606304753 ) ) ;
#6978 = CARTESIAN_POINT ( 'NONE',  ( 5.444914386472297529, 33.16171875108393152, -13.14518615778179722 ) ) ;
#6979 = CARTESIAN_POINT ( 'NONE',  ( -9.598844408820458085, 32.16953124999999147, -9.598844408820458085 ) ) ;
#6980 = CARTESIAN_POINT ( 'NONE',  ( 124.5550856135277087, 36.63437500108393863, -13.14518615778179722 ) ) ;
#6981 = EDGE_LOOP ( 'NONE', ( #25937, #23499, #17064, #16760 ) ) ;
#6982 = CARTESIAN_POINT ( 'NONE',  ( -13.14518615778179189, 34.45156250108394147, 5.444914386472304635 ) ) ;
#6983 = EDGE_CURVE ( 'NONE', #12084, #12988, #12687, .T. ) ;
#6984 = CARTESIAN_POINT ( 'NONE',  ( 139.2950502721270425, 32.91367187608393152, 9.295050272127046043 ) ) ;
#6985 = CARTESIAN_POINT ( 'NONE',  ( 51.42518405393695957, 34.60039062499999574, -5.622872871577873077 ) ) ;
#6986 = DIRECTION ( 'NONE',  ( 0.000000000000000000, 0.000000000000000000, -1.000000000000000000 ) ) ;
#6987 = CARTESIAN_POINT ( 'NONE',  ( 95.54126587499996504, 1.387778780781445676E-14, 9.687500001365593860 ) ) ;
#6989 = DIRECTION ( 'NONE',  ( 0.000000000000000000, 0.000000000000000000, 1.000000000000000000 ) ) ;
#6988 = VECTOR ( 'NONE', #1398, 1000.000000000000000 ) ;
#6990 = CARTESIAN_POINT ( 'NONE',  ( 103.1528011352953342, 3.152801135295383084, 1.062500001365592528 ) ) ;
#6991 = CARTESIAN_POINT ( 'NONE',  ( 108.0825317500000153, 110.0000000000000000, -44.12500000273119127 ) ) ;
#6992 = DIRECTION ( 'NONE',  ( 1.000000000000000000, 0.000000000000000000, 0.000000000000000000 ) ) ;
#6993 = LINE ( 'NONE', #15540, #16637 ) ;
#6994 = CARTESIAN_POINT ( 'NONE',  ( 108.0825317499999869, 112.6261737610028320, -46.52499999726882152 ) ) ;
#6995 = CARTESIAN_POINT ( 'NONE',  ( -13.14518615778179900, 35.93984375108393436, -5.444914386472297529 ) ) ;
#6996 = CARTESIAN_POINT ( 'NONE',  ( 95.67376207875069838, 115.9545556584642867, -46.79999999453764303 ) ) ;
#6997 = VERTEX_POINT ( 'NONE', #8999 ) ;
#6998 = CARTESIAN_POINT ( 'NONE',  ( 99.99999999999998579, 123.3500000010924680, 2.066987299999980099 ) ) ;
#6999 = CARTESIAN_POINT ( 'NONE',  ( -14.99999999999999822, 75.00000000000000000, 15.00000000000000000 ) ) ;
#7000 = CARTESIAN_POINT ( 'NONE',  ( -15.00000000000000000, 75.00000000000000000, 9.999999999999998224 ) ) ;
#7001 = CARTESIAN_POINT ( 'NONE',  ( 195.0000000000000000, 34.79882812608393294, -13.14518615778179544 ) ) ;
#7002 = VERTEX_POINT ( 'NONE', #15248 ) ;
#7003 = CARTESIAN_POINT ( 'NONE',  ( 99.99999999999997158, 117.3602355696678643, -48.99999999453763877 ) ) ;
#7004 = CARTESIAN_POINT ( 'NONE',  ( 98.15313185440925281, -4.458734124999987891, 10.87500000136559386 ) ) ;
#7005 = ORIENTED_EDGE ( 'NONE', *, *, #9687, .F. ) ;
#7006 = CARTESIAN_POINT ( 'NONE',  ( 97.50236033167492167, 102.3130555110000159, -52.97500000273119980 ) ) ;
#7007 = CARTESIAN_POINT ( 'NONE',  ( -13.14518615778179189, 37.42812500108393436, 5.444914386472304635 ) ) ;
#7008 = CARTESIAN_POINT ( 'NONE',  ( 102.4999999999999716, 124.5500000000000114, 1.035533905932722876 ) ) ;
#7009 = CARTESIAN_POINT ( 'NONE',  ( 120.4011555911795455, 32.46718750216787441, 9.598844408820459861 ) ) ;
#7010 = CARTESIAN_POINT ( 'NONE',  ( 0.000000000000000000, 23.00000000000000000, -23.00000000000001421 ) ) ;
#7011 = CARTESIAN_POINT ( 'NONE',  ( 97.92893218813452449, 93.18749999726878741, -4.999999999999997335 ) ) ;
#7012 = CARTESIAN_POINT ( 'NONE',  ( 51.85481384221820633, 36.78320312608393294, 0.000000000000000000 ) ) ;
#7013 = CARTESIAN_POINT ( 'NONE',  ( 59.67620903604532145, 54.47170356488064868, -15.00000000000000000 ) ) ;
#7014 = CARTESIAN_POINT ( 'NONE',  ( 102.4976396683250925, 117.6869444889999841, -51.97500000273119980 ) ) ;
#7015 = CARTESIAN_POINT ( 'NONE',  ( 200.4449143864723055, 32.26875000108393721, 13.14518615778179189 ) ) ;
#7016 = EDGE_CURVE ( 'NONE', #20608, #19588, #17692, .T. ) ;
#7017 = CARTESIAN_POINT ( 'NONE',  ( 99.99999999999998579, 130.0000000000000000, -10.50000000000002132 ) ) ;
#7018 = ORIENTED_EDGE ( 'NONE', *, *, #26568, .T. ) ;
#7019 = CARTESIAN_POINT ( 'NONE',  ( 2.414731522848535132E-15, 35.39414062608393863, 13.14518615778179544 ) ) ;
#7020 = CARTESIAN_POINT ( 'NONE',  ( 103.1528011352953342, 3.152801135295383084, 11.31250000136559386 ) ) ;
#7021 = CARTESIAN_POINT ( 'NONE',  ( 78.14518615778180788, 37.03125000108393294, -5.444914386472297529 ) ) ;
#7022 = FACE_OUTER_BOUND ( 'NONE', #16990, .T. ) ;
#7023 = CARTESIAN_POINT ( 'NONE',  ( 0.000000000000000000, 30.99999999999999645, -15.57481594606304576 ) ) ;
#7024 = CARTESIAN_POINT ( 'NONE',  ( 2.414731522848535132E-15, 38.56914062608393579, 13.14518615778179544 ) ) ;
#7025 = CARTESIAN_POINT ( 'NONE',  ( 200.4449143864723055, 37.82500000108392868, 13.14518615778179189 ) ) ;
#7026 = CARTESIAN_POINT ( 'NONE',  ( 91.91746824999998466, 110.0000000000000000, -45.87499999726882294 ) ) ;
#7027 = ORIENTED_EDGE ( 'NONE', *, *, #16450, .T. ) ;
#7028 = CIRCLE ( 'NONE', #16152, 12.50000000000001599 ) ;
#7029 = CARTESIAN_POINT ( 'NONE',  ( -13.57481594606304576, 33.06249999999999289, 0.000000000000000000 ) ) ;
#7030 = CARTESIAN_POINT ( 'NONE',  ( 2.414731522848535132E-15, 33.60820312608392868, 13.14518615778179544 ) ) ;
#7031 = ORIENTED_EDGE ( 'NONE', *, *, #9332, .F. ) ;
#7032 = CARTESIAN_POINT ( 'NONE',  ( 116.8548138422182205, 32.02070312608393010, 0.000000000000000000 ) ) ;
#7033 = CARTESIAN_POINT ( 'NONE',  ( 2.493653234604083739E-15, 35.74140625216787015, 13.57481594606304576 ) ) ;
#7034 = CARTESIAN_POINT ( 'NONE',  ( 185.7049497278729575, 33.50898437608393010, -9.295050272127046043 ) ) ;
#7035 = ORIENTED_EDGE ( 'NONE', *, *, #13115, .F. ) ;
#7036 = CARTESIAN_POINT ( 'NONE',  ( 5.444914386472297529, 32.36796875108393579, -13.14518615778179900 ) ) ;
#7037 =( BOUNDED_CURVE ( )  B_SPLINE_CURVE ( 2, ( #15496, #24489, #699, #22076, #7228, #19929, #15919, #9096, #19785, #13494, #17791 ),
 .UNSPECIFIED., .F., .T. ) 
 B_SPLINE_CURVE_WITH_KNOTS ( ( 3, 2, 2, 2, 2, 3 ),
 ( 0.000000000000000000, 0.02000000000000000042, 0.04000000000000000083, 0.05999999999999999778, 0.08000000000000000167, 0.1000000000000000194 ),
 .UNSPECIFIED. ) 
 CURVE ( )  GEOMETRIC_REPRESENTATION_ITEM ( )  RATIONAL_B_SPLINE_CURVE ( ( 1.000000000000000000, 0.9510565162951535312, 1.000000000000000000, 0.9510565162951535312, 1.000000000000000000, 0.9510565162951535312, 1.000000000000000000, 0.9510565162951535312, 1.000000000000000000, 0.9510565162951535312, 1.000000000000000000 ) ) 
 REPRESENTATION_ITEM ( '' )  );
#7038 = CARTESIAN_POINT ( 'NONE',  ( 102.0710678118654329, -4.999999999999989342, 5.437500002731185056 ) ) ;
#7039 = LINE ( 'NONE', #2370, #6249 ) ;
#7040 = CARTESIAN_POINT ( 'NONE',  ( 104.9999999999999716, -2.071067811865462627, 2.562500002731185500 ) ) ;
#7041 = EDGE_CURVE ( 'NONE', #8293, #27581, #18710, .T. ) ;
#7042 = CARTESIAN_POINT ( 'NONE',  ( 13.57481594606304753, 36.68398437500000142, -5.622872871577873966 ) ) ;
#7043 = CARTESIAN_POINT ( 'NONE',  ( 208.1451861577818079, 39.56132812608393579, -1.609821015232357215E-15 ) ) ;
#7044 = VECTOR ( 'NONE', #25416, 1000.000000000000000 ) ;
#7045 = ORIENTED_EDGE ( 'NONE', *, *, #23457, .T. ) ;
#7046 = CARTESIAN_POINT ( 'NONE',  ( 95.54126587499996504, 1.387778780781445676E-14, 4.437500001365592084 ) ) ;
#7047 = ORIENTED_EDGE ( 'NONE', *, *, #25412, .T. ) ;
#7048 = CARTESIAN_POINT ( 'NONE',  ( 98.23223304703363112, 122.8000000021849587, 1.767766952966351557 ) ) ;
#7049 = CARTESIAN_POINT ( 'NONE',  ( 103.1528011352953342, 3.152801135295383084, 7.062500001365592084 ) ) ;
#7050 = CARTESIAN_POINT ( 'NONE',  ( 138.7693896720707301, 50.37710889400712233, 14.99999999999734079 ) ) ;
#7051 = EDGE_CURVE ( 'NONE', #23888, #9529, #16819, .T. ) ;
#7052 = CARTESIAN_POINT ( 'NONE',  ( 9.295050272127047819, 36.08867187608392868, 9.295050272127046043 ) ) ;
#7053 = DIRECTION ( 'NONE',  ( 0.000000000000000000, -0.000000000000000000, 1.000000000000000000 ) ) ;
#7054 = CYLINDRICAL_SURFACE ( 'NONE', #18354, 13.57481594606304398 ) ;
#7055 = CARTESIAN_POINT ( 'NONE',  ( 51.85481384221819923, 35.14609375108393152, -5.444914386472297529 ) ) ;
#7056 = CARTESIAN_POINT ( 'NONE',  ( 91.91746824999998466, 107.3738262389971538, -45.02500000273118985 ) ) ;
#7057 = CARTESIAN_POINT ( 'NONE',  ( -8.049105076161786076E-16, 37.18007812608393436, -13.14518615778179544 ) ) ;
#7058 = STYLED_ITEM ( 'NONE', ( #3800 ), #16871 ) ;
#7059 = AXIS2_PLACEMENT_3D ( 'NONE', #30, #17263, #25964 ) ;
#7060 = CARTESIAN_POINT ( 'NONE',  ( 102.1631189606246295, 116.6573956140660897, -49.10000000546237686 ) ) ;
#7061 = CARTESIAN_POINT ( 'NONE',  ( 1.892183357089636475, 53.66387243067953960, 14.99999999999999645 ) ) ;
#7062 = CARTESIAN_POINT ( 'NONE',  ( 105.6631189606246153, 114.1144967660473242, -55.29999999453764303 ) ) ;
#7063 = CARTESIAN_POINT ( 'NONE',  ( 124.3771271284221314, 37.97382812499999716, 13.57481594606304753 ) ) ;
#7064 = ORIENTED_EDGE ( 'NONE', *, *, #8116, .F. ) ;
#7065 = EDGE_CURVE ( 'NONE', #19120, #19945, #15539, .T. ) ;
#7066 = ORIENTED_EDGE ( 'NONE', *, *, #1945, .T. ) ;
#7067 = CARTESIAN_POINT ( 'NONE',  ( -13.57481594606304576, 40.30546875216787583, 0.000000000000000000 ) ) ;
#7068 = CARTESIAN_POINT ( 'NONE',  ( -13.14518615778179189, 33.65781250108393152, 5.444914386472304635 ) ) ;
#7069 = CARTESIAN_POINT ( 'NONE',  ( -9.598844408820454532, 34.84843750216787583, 9.598844408820459861 ) ) ;
#7070 = CARTESIAN_POINT ( 'NONE',  ( 104.9999999999999716, 1.449011120738813565E-14, 8.625000002731185944 ) ) ;
#7071 = CARTESIAN_POINT ( 'NONE',  ( 135.4449143864723055, 33.95546875108393436, -13.14518615778179900 ) ) ;
#7072 = CARTESIAN_POINT ( 'NONE',  ( 74.59884440882045453, 33.45937500216787441, 9.598844408820456309 ) ) ;
#7073 = AXIS2_PLACEMENT_3D ( 'NONE', #18872, #23720, #12576 ) ;
#7074 = FACE_OUTER_BOUND ( 'NONE', #14902, .T. ) ;
#7075 = CARTESIAN_POINT ( 'NONE',  ( -13.57481594606304576, 33.21132812716787441, 5.622872871577880183 ) ) ;
#7076 = CARTESIAN_POINT ( 'NONE',  ( 97.92893218813451028, 5.000000000000018652, 2.812499999999999112 ) ) ;
#7077 = CARTESIAN_POINT ( 'NONE',  ( 108.0825317500000011, 110.0000000000000000, -48.87499999726882294 ) ) ;
#7078 = CARTESIAN_POINT ( 'NONE',  ( 9.598844408820459861, 39.01562500216787299, 9.598844408820456309 ) ) ;
#7079 = CARTESIAN_POINT ( 'NONE',  ( 204.2950502721270425, 35.49335937608393010, -9.295050272127046043 ) ) ;
#7080 = CARTESIAN_POINT ( 'NONE',  ( 99.99999999999995737, 1.387778780781445676E-14, 15.00000000000000000 ) ) ;
#7081 = DIRECTION ( 'NONE',  ( 0.000000000000000000, 0.000000000000000000, 1.000000000000000000 ) ) ;
#7082 = CARTESIAN_POINT ( 'NONE',  ( 0.000000000000000000, 23.00000000000000000, 0.000000000000000000 ) ) ;
#7083 = DIRECTION ( 'NONE',  ( 0.000000000000000000, 1.000000000000000000, 0.000000000000000000 ) ) ;
#7084 = CARTESIAN_POINT ( 'NONE',  ( 102.4999999999999858, 123.1000000021849416, -9.847140817659276890E-15 ) ) ;
#7085 = CARTESIAN_POINT ( 'NONE',  ( -13.57481594606304753, 33.80664062500000000, -5.622872871577873077 ) ) ;
#7086 = CARTESIAN_POINT ( 'NONE',  ( 130.0000000000000000, 38.02343749999999289, 13.57481594606304576 ) ) ;
#7087 = CARTESIAN_POINT ( 'NONE',  ( -13.14518615778179189, 32.86406250108393579, 5.444914386472304635 ) ) ;
#7088 = CARTESIAN_POINT ( 'NONE',  ( -8.049105076161786076E-16, 34.79882812608393294, -13.14518615778179544 ) ) ;
#7089 = CARTESIAN_POINT ( 'NONE',  ( 208.5748159460630120, 35.79101562499999289, 5.622872871577869525 ) ) ;
#7090 = EDGE_CURVE ( 'NONE', #12549, #11568, #5907, .T. ) ;
#7091 = CARTESIAN_POINT ( 'NONE',  ( -5.622872871577873077, 36.48554687716787015, 13.57481594606304753 ) ) ;
#7092 = CARTESIAN_POINT ( 'NONE',  ( 99.99999999999998579, 110.0000000000000000, -45.00000000000000711 ) ) ;
#7093 = CARTESIAN_POINT ( 'NONE',  ( 96.84719886470459471, 82.31250000136559208, -3.152801135295383084 ) ) ;
#7094 = CARTESIAN_POINT ( 'NONE',  ( 78.14518615778179367, 35.39414062608393152, -1.609821015232357215E-15 ) ) ;
#7095 =( BOUNDED_CURVE ( )  B_SPLINE_CURVE ( 2, ( #6502, #21623, #27902, #15178, #12479, #10492, #102, #25481, #8223 ),
 .UNSPECIFIED., .F., .F. ) 
 B_SPLINE_CURVE_WITH_KNOTS ( ( 3, 2, 2, 2, 3 ),
 ( 0.2142857142857142183, 0.2232142857142856707, 0.2321428571428570953, 0.2410714285714285199, 0.2499999999999999445 ),
 .UNSPECIFIED. ) 
 CURVE ( )  GEOMETRIC_REPRESENTATION_ITEM ( )  RATIONAL_B_SPLINE_CURVE ( ( 1.000000000000000444, 0.9238795325112862944, 1.000000000000000000, 0.9238795325112867385, 1.000000000000000000, 0.9238795325112867385, 1.000000000000000000, 0.9238795325112871826, 0.9999999999999995559 ) ) 
 REPRESENTATION_ITEM ( '' )  );
#7096 = CARTESIAN_POINT ( 'NONE',  ( 93.46109445667491400, 105.2492070361643215, -53.17500000273119554 ) ) ;
#7097 = CARTESIAN_POINT ( 'NONE',  ( 98.69444032418647339, 123.0000000000000426, -2.137373984154804063 ) ) ;
#7098 = CARTESIAN_POINT ( 'NONE',  ( 102.0669872999999939, 123.3000000010924850, 0.8561741729129311862 ) ) ;
#7099 = CARTESIAN_POINT ( 'NONE',  ( 9.598844408820456309, 33.55859375000000000, -9.598844408820458085 ) ) ;
#7100 = CARTESIAN_POINT ( 'NONE',  ( 139.2950502721270425, 37.08085937608393579, 9.295050272127046043 ) ) ;
#7101 = ORIENTED_EDGE ( 'NONE', *, *, #15580, .F. ) ;
#7102 = CARTESIAN_POINT ( 'NONE',  ( 103.5355339059327093, 80.37500000000000000, 3.535533905932726206 ) ) ;
#7103 = CARTESIAN_POINT ( 'NONE',  ( 98.14342173294696181, 123.0000000000000426, 0.9730510570952660698 ) ) ;
#7104 = CARTESIAN_POINT ( 'NONE',  ( 96.46446609406721961, 82.00000000273119838, -3.535533905932755072 ) ) ;
#7105 = AXIS2_PLACEMENT_3D ( 'NONE', #3757, #24997, #16295 ) ;
#7106 = CARTESIAN_POINT ( 'NONE',  ( 102.0710678118654613, 92.81249999999998579, 4.999999999999983125 ) ) ;
#7107 = CARTESIAN_POINT ( 'NONE',  ( 99.99999999999997158, 101.5015231886685854, -49.12499999726882294 ) ) ;
#7108 = CARTESIAN_POINT ( 'NONE',  ( 68.75563815586001226, 31.78804748261757140, -13.14518615778179367 ) ) ;
#7109 = ORIENTED_EDGE ( 'NONE', *, *, #17152, .F. ) ;
#7110 = B_SPLINE_CURVE_WITH_KNOTS ( 'NONE', 3,
 ( #8202, #16893, #20386, #16241, #21047, #3938, #1530, #10182, #12598, #5280, #873, #18892, #27602, #23324, #8062, #21324, #7255, #15945, #22671, #16757, #26953, #13944, #3143, #9684, #11810, #20533, #25457, #5938, #3797, #15157, #13156 ),
 .UNSPECIFIED., .F., .F.,
 ( 4, 2, 2, 2, 2, 2, 2, 2, 2, 2, 1, 2, 2, 2, 2, 4 ),
 ( 1.175569253024769036E-15, 0.001656255954914826172, 0.003312511909828477069, 0.004968767864742128400, 0.005796895842198994397, 0.006625023819655860395, 0.008281279774569594992, 0.009937535729483326988, 0.01325004763931079445, 0.01490630359422449695, 0.01656255954913820119, 0.01821881550405190370, 0.01987507145896560620, 0.02318758336879301468, 0.02484383932370672413, 0.02650009527862043010 ),
 .UNSPECIFIED. ) ;
#7111 = CARTESIAN_POINT ( 'NONE',  ( 94.99999999999995737, 1.387778780781445676E-14, 13.00000000000000000 ) ) ;
#7112 = ORIENTED_EDGE ( 'NONE', *, *, #25532, .T. ) ;
#7113 = CARTESIAN_POINT ( 'NONE',  ( 2.414731522848535132E-15, 37.77539062608393294, 13.14518615778179544 ) ) ;
#7114 = CARTESIAN_POINT ( 'NONE',  ( 195.0000000000000000, 32.96328125216787441, -13.57481594606304576 ) ) ;
#7115 = AXIS2_PLACEMENT_3D ( 'NONE', #12959, #25542, #19399 ) ;
#7116 = ORIENTED_EDGE ( 'NONE', *, *, #25691, .T. ) ;
#7117 = CARTESIAN_POINT ( 'NONE',  ( 3.755638265659908104, 31.58960998161716560, -13.14518615778179722 ) ) ;
#7118 = CARTESIAN_POINT ( 'NONE',  ( -5.622872871577767384, 40.85117187499999147, -13.57481594606315412 ) ) ;
#7119 = CARTESIAN_POINT ( 'NONE',  ( 103.5355339059327093, -3.535533905932726206, 3.374999999999999556 ) ) ;
#7120 = CARTESIAN_POINT ( 'NONE',  ( 5.444914386472297529, 35.74140625108393721, -13.14518615778179900 ) ) ;
#7121 = DIRECTION ( 'NONE',  ( 1.000000000000000000, 0.000000000000000000, 0.000000000000000000 ) ) ;
#7122 = CARTESIAN_POINT ( 'NONE',  ( 59.37712712842213136, 32.11992187499999574, -13.57481594606304753 ) ) ;
#7123 = AXIS2_PLACEMENT_3D ( 'NONE', #27227, #22516, #7680 ) ;
#7124 = CARTESIAN_POINT ( 'NONE',  ( -13.14518615778179544, 40.55351562608393579, 0.000000000000000000 ) ) ;
#7125 = DIRECTION ( 'NONE',  ( -0.8660254037844392627, -0.000000000000000000, 0.4999999999999987788 ) ) ;
#7126 = CARTESIAN_POINT ( 'NONE',  ( 95.54126587499995082, -1.846868145590724986, 10.75000000136559208 ) ) ;
#7127 = CARTESIAN_POINT ( 'NONE',  ( 94.99999999999995737, 1.387778780781445676E-14, 2.125000002731185056 ) ) ;
#7128 = CARTESIAN_POINT ( 'NONE',  ( 95.54126587499996504, 1.846868145590750077, 13.37500000136559386 ) ) ;
#7129 = CARTESIAN_POINT ( 'NONE',  ( 91.91746824999998466, 112.6261737610028320, -47.22500000273119269 ) ) ;
#7130 = CARTESIAN_POINT ( 'NONE',  ( 96.84719886470463734, 91.93749999863440792, -3.152801135295366208 ) ) ;
#7131 = DIRECTION ( 'NONE',  ( -0.000000000000000000, -0.000000000000000000, -1.000000000000000000 ) ) ;
#7132 = CARTESIAN_POINT ( 'NONE',  ( 104.9952793366501567, 116.8754121666685393, -52.32499999726881867 ) ) ;
#7133 = CARTESIAN_POINT ( 'NONE',  ( -13.14518615778179544, 35.98945312608393721, 0.000000000000000000 ) ) ;
#7134 = VERTEX_POINT ( 'NONE', #4167 ) ;
#7135 = CARTESIAN_POINT ( 'NONE',  ( 120.4011555911795455, 36.93203124999999432, -9.598844408820458085 ) ) ;
#7136 = VECTOR ( 'NONE', #23795, 1000.000000000000000 ) ;
#7137 = CARTESIAN_POINT ( 'NONE',  ( 99.99999999999998579, 91.75000000000000000, 4.999999999999984013 ) ) ;
#7138 = CARTESIAN_POINT ( 'NONE',  ( 96.46446609406721961, -3.535533905932727539, 1.124999999999999334 ) ) ;
#7139 = EDGE_CURVE ( 'NONE', #12585, #4508, #17403, .T. ) ;
#7140 = CARTESIAN_POINT ( 'NONE',  ( 181.8548138422182205, 34.99726562608393721, 0.000000000000000000 ) ) ;
#7141 = ADVANCED_FACE ( 'NONE', ( #24247 ), #25819, .T. ) ;
#7142 = ORIENTED_EDGE ( 'NONE', *, *, #2897, .F. ) ;
#7143 = DIRECTION ( 'NONE',  ( -0.000000000000000000, -1.000000000000000000, -0.000000000000000000 ) ) ;
#7144 = CARTESIAN_POINT ( 'NONE',  ( 95.54126587499996504, 1.387778780781445676E-14, 12.68750000136559208 ) ) ;
#7145 = ORIENTED_EDGE ( 'NONE', *, *, #24323, .F. ) ;
#7146 = CARTESIAN_POINT ( 'NONE',  ( 99.99999999999998579, 102.6397644303321215, -45.50000000000000000 ) ) ;
#7147 = CARTESIAN_POINT ( 'NONE',  ( 13.14518615778179900, 36.13828125108393863, 5.444914386472293977 ) ) ;
#7148 = CARTESIAN_POINT ( 'NONE',  ( 97.92893218813443923, 79.31250000273119838, 4.999999999999927169 ) ) ;
#7149 = CARTESIAN_POINT ( 'NONE',  ( 116.8548138422182063, 36.63437500108393152, 5.444914386472304635 ) ) ;
#7150 = CARTESIAN_POINT ( 'NONE',  ( 130.0000000000000000, 36.00000000000000000, -1.503427012513233026E-14 ) ) ;
#7151 = CARTESIAN_POINT ( 'NONE',  ( 13.14518615778179900, 36.23750000108393010, -5.444914386472297529 ) ) ;
#7152 = CARTESIAN_POINT ( 'NONE',  ( 99.99999999999998579, 95.62499999726881583, 4.999999999999984013 ) ) ;
#7153 = CARTESIAN_POINT ( 'NONE',  ( 74.29505027212704249, 36.48554687608393721, -9.295050272127046043 ) ) ;
#7154 = CARTESIAN_POINT ( 'NONE',  ( 55.81982418635197973, 55.00000000000000000, -15.00000000000000000 ) ) ;
#7155 = CARTESIAN_POINT ( 'NONE',  ( 99.99999999999998579, 101.5015231886685712, -48.87500000273119838 ) ) ;
#7156 = CARTESIAN_POINT ( 'NONE',  ( 204.5988444088204403, 40.70234374999999716, -9.598844408820458085 ) ) ;
#7157 = FACE_OUTER_BOUND ( 'NONE', #21496, .T. ) ;
#7158 = EDGE_LOOP ( 'NONE', ( #13000, #16890, #7733, #19744 ) ) ;
#7159 = CARTESIAN_POINT ( 'NONE',  ( 2.414731522848535132E-15, 36.18789062608393436, 13.14518615778179544 ) ) ;
#7160 = CARTESIAN_POINT ( 'NONE',  ( 98.15313185440923860, -4.458734124999987891, 6.875000001365592972 ) ) ;
#7161 = CARTESIAN_POINT ( 'NONE',  ( 70.44491438647229131, 38.42031250108393436, 13.14518615778179189 ) ) ;
#7162 = CARTESIAN_POINT ( 'NONE',  ( 51.42518405393695957, 38.56914062499999574, -5.622872871577872189 ) ) ;
#7163 = CARTESIAN_POINT ( 'NONE',  ( 104.9999999999999716, 1.449011120738813565E-14, 14.49999999999999822 ) ) ;
#7164 = CARTESIAN_POINT ( 'NONE',  ( -13.14518615778179544, 33.60820312608393579, 0.000000000000000000 ) ) ;
#7165 = CARTESIAN_POINT ( 'NONE',  ( 99.99999999999998579, 91.81249999863440792, -4.458734124999994997 ) ) ;
#7166 = CARTESIAN_POINT ( 'NONE',  ( 208.1451861577818079, 38.81718750108393579, -5.444914386472297529 ) ) ;
#7167 = CARTESIAN_POINT ( 'NONE',  ( 99.99999999999997158, 118.4984768113314004, -46.37499999726880873 ) ) ;
#7168 = ORIENTED_EDGE ( 'NONE', *, *, #15254, .F. ) ;
#7169 = CARTESIAN_POINT ( 'NONE',  ( 9.598844408820459861, 34.15390624999999858, 9.598844408820456309 ) ) ;
#7170 = CARTESIAN_POINT ( 'NONE',  ( 13.14518615778179900, 34.55078125108393294, 5.444914386472293977 ) ) ;
#7171 = VERTEX_POINT ( 'NONE', #19978 ) ;
#7172 = CARTESIAN_POINT ( 'NONE',  ( 139.2950502721270425, 33.31054687608394005, -9.295050272127046043 ) ) ;
#7173 = CARTESIAN_POINT ( 'NONE',  ( 51.85481384221820633, 31.82226562608393650, 0.000000000000000000 ) ) ;
#7174 = CARTESIAN_POINT ( 'NONE',  ( 181.8548138422181921, 35.14609375108393152, -5.444914386472297529 ) ) ;
#7175 = EDGE_LOOP ( 'NONE', ( #11411, #16309, #5568, #10498 ) ) ;
#7176 = CARTESIAN_POINT ( 'NONE',  ( 98.09035273295538104, 123.0000000000000142, 0.7910017786517971050 ) ) ;
#7177 = CARTESIAN_POINT ( 'NONE',  ( 95.00000000000000000, 91.43749999726880162, 2.071067811865463959 ) ) ;
#7178 = DIRECTION ( 'NONE',  ( -5.782411586589357392E-17, -0.000000000000000000, -1.000000000000000000 ) ) ;
#7179 = CARTESIAN_POINT ( 'NONE',  ( 94.99999999999995737, 1.387778780781445676E-14, 34.79898987322334136 ) ) ;
#7180 = CARTESIAN_POINT ( 'NONE',  ( 93.46109445667491400, 105.2492070361643215, -46.92500000273119554 ) ) ;
#7181 = CARTESIAN_POINT ( 'NONE',  ( 103.5355339059327093, 3.535533905932755072, 10.62499999999999822 ) ) ;
#7182 = CARTESIAN_POINT ( 'NONE',  ( 99.99999999999998579, 89.99899999999999523, -2.500000000000004885 ) ) ;
#7183 = CARTESIAN_POINT ( 'NONE',  ( 74.18017581364802027, 50.00000000000000000, 9.999999999999966249 ) ) ;
#7184 = CARTESIAN_POINT ( 'NONE',  ( 103.1528011352953342, -3.152801135295355106, 4.812500001365592084 ) ) ;
#7185 = ORIENTED_EDGE ( 'NONE', *, *, #19222, .T. ) ;
#7186 = CARTESIAN_POINT ( 'NONE',  ( -11.14554687309540348, 36.00000000000000711, -7.260818043107225783 ) ) ;
#7187 = CARTESIAN_POINT ( 'NONE',  ( 96.84719886470459471, -3.152801135295355994, 9.562500001365593860 ) ) ;
#7188 = CARTESIAN_POINT ( 'NONE',  ( 143.5748159460630688, 38.27148437716787299, 5.622872871577868636 ) ) ;
#7189 = AXIS2_PLACEMENT_3D ( 'NONE', #16041, #20055, #826 ) ;
#7190 = CARTESIAN_POINT ( 'NONE',  ( -9.295050272127046043, 37.27929687608393294, -9.295050272127046043 ) ) ;
#7191 = CARTESIAN_POINT ( 'NONE',  ( 0.2703369776638426258, 35.99999999999999289, 13.14949859323921721 ) ) ;
#7192 = CARTESIAN_POINT ( 'NONE',  ( 2.385244779468109360E-15, 75.00000000000000000, 9.999999999999996447 ) ) ;
#7193 = CARTESIAN_POINT ( 'NONE',  ( 95.54126587500000767, 93.81249999863440792, -7.484931351350258973E-15 ) ) ;
#7194 = EDGE_CURVE ( 'NONE', #19665, #8206, #320, .T. ) ;
#7195 = CARTESIAN_POINT ( 'NONE',  ( 102.4976396683250925, 102.3130555110000159, -46.52500000273119696 ) ) ;
#7196 = CARTESIAN_POINT ( 'NONE',  ( -5.444914386472297529, 38.81718750108393579, -13.14518615778179722 ) ) ;
#7197 = CARTESIAN_POINT ( 'NONE',  ( 97.50000000000000000, 124.6500000010924651, -9.540979117872439019E-15 ) ) ;
#7198 = CARTESIAN_POINT ( 'NONE',  ( -8.211314015175641856, 50.68678854790643840, 15.00000000000000178 ) ) ;
#7199 = CARTESIAN_POINT ( 'NONE',  ( 95.00000000000000000, 91.37499999726880162, -7.551217303480904118E-15 ) ) ;
#7200 = CARTESIAN_POINT ( 'NONE',  ( 120.4011555911795455, 35.54296874999999289, 9.598844408820459861 ) ) ;
#7201 = ORIENTED_EDGE ( 'NONE', *, *, #13476, .T. ) ;
#7202 = CARTESIAN_POINT ( 'NONE',  ( 2.493653234604083739E-15, 33.26093749999999716, 13.57481594606304576 ) ) ;
#7203 = CARTESIAN_POINT ( 'NONE',  ( 5.444914386472297529, 34.15390625108393863, -13.14518615778179900 ) ) ;
#7204 = CARTESIAN_POINT ( 'NONE',  ( 9.598844408820459861, 33.45937500216787441, 9.598844408820456309 ) ) ;
#7205 =( BOUNDED_CURVE ( )  B_SPLINE_CURVE ( 2, ( #20992, #27409, #5608, #3322, #9587, #12267, #7444, #14274, #23272, #1473, #7872 ),
 .UNSPECIFIED., .F., .F. ) 
 B_SPLINE_CURVE_WITH_KNOTS ( ( 3, 2, 2, 2, 2, 3 ),
 ( 0.4999999999999996669, 0.5199999999999996847, 0.5399999999999998135, 0.5599999999999998312, 0.5799999999999998490, 0.5999999999999998668 ),
 .UNSPECIFIED. ) 
 CURVE ( )  GEOMETRIC_REPRESENTATION_ITEM ( )  RATIONAL_B_SPLINE_CURVE ( ( 1.000000000000000888, 0.9510565162951527540, 1.000000000000000000, 0.9510565162951535312, 1.000000000000000000, 0.9510565162951535312, 1.000000000000000000, 0.9510565162951535312, 1.000000000000000000, 0.9510565162951537532, 0.9999999999999997780 ) ) 
 REPRESENTATION_ITEM ( '' )  );
#7206 = CARTESIAN_POINT ( 'NONE',  ( 99.99999999999995737, 5.000000000000018652, 10.87500000273118594 ) ) ;
#7207 = CARTESIAN_POINT ( 'NONE',  ( 143.1451861577818079, 33.75703125108393010, 5.444914386472293977 ) ) ;
#7208 = EDGE_CURVE ( 'NONE', #613, #2910, #27676, .T. ) ;
#7209 = CARTESIAN_POINT ( 'NONE',  ( 70.44491438647230552, 40.30546875108393579, -13.14518615778179900 ) ) ;
#7210 = ADVANCED_FACE ( 'NONE', ( #4876 ), #2869, .T. ) ;
#7211 = VERTEX_POINT ( 'NONE', #1034 ) ;
#7212 = CARTESIAN_POINT ( 'NONE',  ( 99.99999999999995737, 80.75000000000000000, -5.000000000000018652 ) ) ;
#7213 = CARTESIAN_POINT ( 'NONE',  ( -13.14518615778179189, 38.22187500108393010, 5.444914386472304635 ) ) ;
#7214 = CIRCLE ( 'NONE', #24976, 7.000000000000006217 ) ;
#7215 = CARTESIAN_POINT ( 'NONE',  ( 104.9999999999999574, 2.071067811865491937, 2.562499999999998668 ) ) ;
#7216 = CARTESIAN_POINT ( 'NONE',  ( 99.99999999999997158, 101.5015231886685712, -51.37499999726882294 ) ) ;
#7217 = CARTESIAN_POINT ( 'NONE',  ( -5.622872871577873077, 38.86679687716788578, 13.57481594606304753 ) ) ;
#7218 = AXIS2_PLACEMENT_3D ( 'NONE', #5982, #7971, #3710 ) ;
#7219 = CARTESIAN_POINT ( 'NONE',  ( 185.7049497278729575, 35.69179687608393436, -9.295050272127046043 ) ) ;
#7220 = CARTESIAN_POINT ( 'NONE',  ( 103.5355339059327093, 3.535533905932755072, 5.750000002731185056 ) ) ;
#7221 = CARTESIAN_POINT ( 'NONE',  ( 97.50000000000000000, 124.2569999999781487, 1.035533905932725096 ) ) ;
#7222 = ADVANCED_FACE ( 'NONE', ( #20257 ), #18406, .F. ) ;
#7223 = CYLINDRICAL_SURFACE ( 'NONE', #7298, 11.57481594606304576 ) ;
#7224 = CARTESIAN_POINT ( 'NONE',  ( 195.0000000000000000, -7.395377635281828788, -2.255140518769849538E-14 ) ) ;
#7225 = CARTESIAN_POINT ( 'NONE',  ( 102.0710678118654329, -4.999999999999989342, 10.43750000273118417 ) ) ;
#7226 = DIRECTION ( 'NONE',  ( -0.000000000000000000, -1.000000000000000000, -0.000000000000000000 ) ) ;
#7227 = CARTESIAN_POINT ( 'NONE',  ( -8.312177448680279460E-16, 33.65781249999999147, -13.57481594606304576 ) ) ;
#7228 = CARTESIAN_POINT ( 'NONE',  ( 97.83688103937535629, 116.6573956140660897, -45.40000000000001279 ) ) ;
#7229 = CARTESIAN_POINT ( 'NONE',  ( 9.295050272127046043, 35.69179687608394147, -9.295050272127046043 ) ) ;
#7230 = CARTESIAN_POINT ( 'NONE',  ( 9.295050272127046043, 37.08085937608393579, -9.295050272127046043 ) ) ;
#7231 = CARTESIAN_POINT ( 'NONE',  ( 1.137167824541903460, 36.00000000000000000, 13.09590655363594180 ) ) ;
#7232 = CARTESIAN_POINT ( 'NONE',  ( 9.598844408820459861, 36.63437500216787157, 9.598844408820456309 ) ) ;
#7233 = DIRECTION ( 'NONE',  ( 0.000000000000000000, 0.000000000000000000, -1.000000000000000000 ) ) ;
#7234 = CARTESIAN_POINT ( 'NONE',  ( 101.8468681455906903, 82.75000000136560629, 4.458734124999987891 ) ) ;
#7235 = CARTESIAN_POINT ( 'NONE',  ( 78.14518615778179367, 32.26875000108393721, -5.444914386472297529 ) ) ;
#7236 = CARTESIAN_POINT ( 'NONE',  ( 106.5389055433251002, 114.7507929638356785, -52.17500000273119554 ) ) ;
#7237 = CARTESIAN_POINT ( 'NONE',  ( 97.70296704779451602, 123.0000000000000000, 0.9970373613995330286 ) ) ;
#7238 = ORIENTED_EDGE ( 'NONE', *, *, #19057, .F. ) ;
#7239 = CARTESIAN_POINT ( 'NONE',  ( 102.0669872999999797, 123.3500000010924680, -9.794112055954760458E-15 ) ) ;
#7240 = CARTESIAN_POINT ( 'NONE',  ( -13.57481594606304576, 33.11210937499999574, 5.622872871577880183 ) ) ;
#7241 = CARTESIAN_POINT ( 'NONE',  ( 135.4449143864723055, 36.53515625108393294, -13.14518615778179900 ) ) ;
#7242 = ADVANCED_FACE ( 'NONE', ( #22689 ), #17831, .F. ) ;
#7243 = ORIENTED_EDGE ( 'NONE', *, *, #10229, .F. ) ;
#7244 = LINE ( 'NONE', #13934, #13625 ) ;
#7245 =( GEOMETRIC_REPRESENTATION_CONTEXT ( 3 ) GLOBAL_UNCERTAINTY_ASSIGNED_CONTEXT ( ( #12316 ) ) GLOBAL_UNIT_ASSIGNED_CONTEXT ( ( #10162, #18871, #22748 ) ) REPRESENTATION_CONTEXT ( 'NONE', 'WORKASPACE' ) );
#7246 = CARTESIAN_POINT ( 'NONE',  ( 195.0000000000000000, 36.53515625216787299, 13.57481594606304576 ) ) ;
#7247 = CARTESIAN_POINT ( 'NONE',  ( 96.84719886470459471, 83.31250000136560629, -3.152801135295383084 ) ) ;
#7248 = CARTESIAN_POINT ( 'NONE',  ( 96.46446609406726225, 92.62500000000000000, 3.535533905932723986 ) ) ;
#7249 = VECTOR ( 'NONE', #2316, 1000.000000000000000 ) ;
#7250 = CARTESIAN_POINT ( 'NONE',  ( 51.42518405393695957, 39.46210937716787726, -5.622872871577873077 ) ) ;
#7251 = ADVANCED_FACE ( 'NONE', ( #11970 ), #15686, .T. ) ;
#7252 = CARTESIAN_POINT ( 'NONE',  ( 108.0825317500000011, 110.0000000000000000, -46.62499999726882294 ) ) ;
#7253 = CARTESIAN_POINT ( 'NONE',  ( 59.37712712842213136, 40.05742187499999574, -13.57481594606304753 ) ) ;
#7254 = ORIENTED_EDGE ( 'NONE', *, *, #2702, .F. ) ;
#7255 = CARTESIAN_POINT ( 'NONE',  ( 187.6059679576637507, 36.00000000000000000, -11.20317769887076764 ) ) ;
#7256 = ADVANCED_FACE ( 'NONE', ( #24533 ), #20015, .T. ) ;
#7257 = CARTESIAN_POINT ( 'NONE',  ( 95.54126587499995082, -1.846868145590724986, 0.7500000013655925279 ) ) ;
#7258 = ORIENTED_EDGE ( 'NONE', *, *, #26612, .T. ) ;
#7259 = CARTESIAN_POINT ( 'NONE',  ( 9.295050272127047819, 35.49335937608393721, 9.295050272127046043 ) ) ;
#7260 = CARTESIAN_POINT ( 'NONE',  ( 189.3771271284221314, 33.80664062716786589, -13.57481594606304753 ) ) ;
#7261 = CARTESIAN_POINT ( 'NONE',  ( 6.944423797152706079, 31.55306878032414986, -11.16113333171310451 ) ) ;
#7262 = CARTESIAN_POINT ( 'NONE',  ( 9.598844408820459861, 36.63437500216787157, 9.598844408820456309 ) ) ;
#7263 = DIRECTION ( 'NONE',  ( 0.8660254037844418162, 0.4999999999999947264, 0.000000000000000000 ) ) ;
#7264 = CARTESIAN_POINT ( 'NONE',  ( -5.444914386472297529, 35.84062500108394289, -13.14518615778179900 ) ) ;
#7265 =( BOUNDED_CURVE ( )  B_SPLINE_CURVE ( 2, ( #22338, #2943, #13468, #2529, #4952, #24325, #17770, #2808, #7202 ),
 .UNSPECIFIED., .F., .F. ) 
 B_SPLINE_CURVE_WITH_KNOTS ( ( 3, 2, 2, 2, 3 ),
 ( 0.7708333333333333703, 0.7812500000000000000, 0.7916666666666665186, 0.8020833333333332593, 0.8124999999999998890 ),
 .UNSPECIFIED. ) 
 CURVE ( )  GEOMETRIC_REPRESENTATION_ITEM ( )  RATIONAL_B_SPLINE_CURVE ( ( 1.000000000000000000, 0.9238795325112867385, 1.000000000000000000, 0.9238795325112867385, 1.000000000000000000, 0.9238795325112867385, 1.000000000000000000, 0.9238795325112875156, 0.9999999999999992228 ) ) 
 REPRESENTATION_ITEM ( '' )  );
#7266 = FACE_OUTER_BOUND ( 'NONE', #1004, .T. ) ;
#7267 = CARTESIAN_POINT ( 'NONE',  ( 78.57481594606304043, 32.61601562499999574, 5.622872871577869525 ) ) ;
#7268 = CARTESIAN_POINT ( 'NONE',  ( 104.9999999999999716, 91.93749999999998579, 2.071067811865467956 ) ) ;
#7269 = DIRECTION ( 'NONE',  ( 0.000000000000000000, 0.000000000000000000, 1.000000000000000000 ) ) ;
#7270 = CARTESIAN_POINT ( 'NONE',  ( 94.99999999999995737, 1.387778780781445676E-14, 0.1250000027311851669 ) ) ;
#7271 = CARTESIAN_POINT ( 'NONE',  ( 103.1528011352953342, 3.152801135295383084, 7.312500001365592084 ) ) ;
#7272 = CYLINDRICAL_SURFACE ( 'NONE', #8952, 13.57481594606304398 ) ;
#7273 = CARTESIAN_POINT ( 'NONE',  ( 101.8468681455907046, 4.458734125000016313, 10.12500000136559208 ) ) ;
#7274 = CARTESIAN_POINT ( 'NONE',  ( 95.67376207875072680, 104.0454443415356991, -52.20000000546237828 ) ) ;
#7275 = DIRECTION ( 'NONE',  ( -0.000000000000000000, 1.000000000000000000, -0.000000000000000000 ) ) ;
#7276 = CARTESIAN_POINT ( 'NONE',  ( 65.00000000000000000, -7.395377635281828788, -7.517135062566165128E-15 ) ) ;
#7277 = CARTESIAN_POINT ( 'NONE',  ( 0.000000000000000000, 36.00000000000000000, 0.000000000000000000 ) ) ;
#7278 = CARTESIAN_POINT ( 'NONE',  ( -9.295050272127046043, 31.92148437608393508, -9.295050272127046043 ) ) ;
#7279 = VECTOR ( 'NONE', #27154, 1000.000000000000000 ) ;
#7280 = ORIENTED_EDGE ( 'NONE', *, *, #16085, .F. ) ;
#7281 = FACE_OUTER_BOUND ( 'NONE', #27266, .T. ) ;
#7282 = DIRECTION ( 'NONE',  ( 0.000000000000000000, 1.000000000000000000, 0.000000000000000000 ) ) ;
#7283 = CARTESIAN_POINT ( 'NONE',  ( 94.99999999999995737, 1.387778780781445676E-14, 0.9999999999999991118 ) ) ;
#7284 = EDGE_CURVE ( 'NONE', #15725, #4666, #4551, .T. ) ;
#7285 = CARTESIAN_POINT ( 'NONE',  ( 181.8548138422181921, 36.63437500108393152, 5.444914386472304635 ) ) ;
#7286 = ORIENTED_EDGE ( 'NONE', *, *, #973, .F. ) ;
#7287 = CARTESIAN_POINT ( 'NONE',  ( 93.00000000000000000, 112.2744378736303332, -48.59999999453764019 ) ) ;
#7288 = CARTESIAN_POINT ( 'NONE',  ( 103.1528011352953342, 3.152801135295383084, 12.31250000136559208 ) ) ;
#7289 = AXIS2_PLACEMENT_3D ( 'NONE', #23861, #12581, #21307 ) ;
#7290 = ORIENTED_EDGE ( 'NONE', *, *, #10285, .T. ) ;
#7291 = CARTESIAN_POINT ( 'NONE',  ( 104.9952793366501851, 103.1245878333314323, -50.67500000273119554 ) ) ;
#7292 = CARTESIAN_POINT ( 'NONE',  ( 5.444914386472297529, 37.92421875108392726, -13.14518615778179900 ) ) ;
#7293 = CARTESIAN_POINT ( 'NONE',  ( -20.00000000000000000, 55.00000000000000000, 10.00000000000000178 ) ) ;
#7294 = CYLINDRICAL_SURFACE ( 'NONE', #16697, 7.000000000000006217 ) ;
#7295 = CARTESIAN_POINT ( 'NONE',  ( 116.8548138422182205, 38.17226562608393436, 0.000000000000000000 ) ) ;
#7296 = CARTESIAN_POINT ( 'NONE',  ( 9.295050272127047819, 37.08085937608393579, 9.295050272127046043 ) ) ;
#7297 = CARTESIAN_POINT ( 'NONE',  ( -9.295050272127046043, 36.48554687608393721, -9.295050272127046043 ) ) ;
#7298 = AXIS2_PLACEMENT_3D ( 'NONE', #27207, #20207, #27062 ) ;
#7299 = CARTESIAN_POINT ( 'NONE',  ( 96.84719886470463734, 92.93749999863440792, -3.152801135295366208 ) ) ;
#7300 =( BOUNDED_CURVE ( )  B_SPLINE_CURVE ( 2, ( #15064, #2551, #12917, #13345, #26197, #6662, #24205, #11072, #19927 ),
 .UNSPECIFIED., .F., .F. ) 
 B_SPLINE_CURVE_WITH_KNOTS ( ( 3, 2, 2, 2, 3 ),
 ( 0.8124999999999998890, 0.8229166666666666297, 0.8333333333333334814, 0.8437500000000003331, 0.8541666666666670737 ),
 .UNSPECIFIED. ) 
 CURVE ( )  GEOMETRIC_REPRESENTATION_ITEM ( )  RATIONAL_B_SPLINE_CURVE ( ( 1.000000000000000888, 0.9238795325112859613, 1.000000000000000000, 0.9238795325112867385, 1.000000000000000000, 0.9238795325112867385, 1.000000000000000000, 0.9238795325112835188, 1.000000000000003331 ) ) 
 REPRESENTATION_ITEM ( '' )  );
#7301 = CARTESIAN_POINT ( 'NONE',  ( -9.598844408820454532, 36.43593750216787441, 9.598844408820459861 ) ) ;
#7302 = CARTESIAN_POINT ( 'NONE',  ( 91.91746824999998466, 112.6261737610028320, -51.47500000273119980 ) ) ;
#7303 = CARTESIAN_POINT ( 'NONE',  ( 76.20653150213495053, 36.00000000000000000, 7.323573988461856032 ) ) ;
#7304 = ORIENTED_EDGE ( 'NONE', *, *, #6007, .T. ) ;
#7305 = CARTESIAN_POINT ( 'NONE',  ( 13.14518615778179900, 34.84843750108393579, -5.444914386472297529 ) ) ;
#7306 = CARTESIAN_POINT ( 'NONE',  ( 104.4587341249999639, 1.442382525525748735E-14, 8.187500001365592084 ) ) ;
#7307 = CARTESIAN_POINT ( 'NONE',  ( 78.14518615778180788, 38.51953125108393294, 5.444914386472293977 ) ) ;
#7308 = LINE ( 'NONE', #9308, #25628 ) ;
#7309 = CARTESIAN_POINT ( 'NONE',  ( 204.2950502721270425, 36.28710937608393294, -9.295050272127046043 ) ) ;
#7310 = EDGE_LOOP ( 'NONE', ( #7887, #26941, #6804, #10999 ) ) ;
#7311 = CARTESIAN_POINT ( 'NONE',  ( 2.414731522848535132E-15, 35.39414062608393863, 13.14518615778179544 ) ) ;
#7312 = CARTESIAN_POINT ( 'NONE',  ( 97.93301269999999192, 124.5000000010924879, -0.8561741729129505041 ) ) ;
#7313 = CARTESIAN_POINT ( 'NONE',  ( 95.54126587499999346, 91.99999999863439371, -1.846868145590737864 ) ) ;
#7314 = CARTESIAN_POINT ( 'NONE',  ( 204.2950502721270425, 37.27929687608394005, -9.295050272127046043 ) ) ;
#7315 = CARTESIAN_POINT ( 'NONE',  ( 91.91746824999997045, 112.6261737610028320, -51.97499999726882436 ) ) ;
#7316 = EDGE_LOOP ( 'NONE', ( #27150, #532, #901, #4150 ) ) ;
#7317 = CARTESIAN_POINT ( 'NONE',  ( -8.312177448680279460E-16, 33.65781249999999147, -13.57481594606304576 ) ) ;
#7318 = CARTESIAN_POINT ( 'NONE',  ( -8.049105076161786076E-16, 34.00507812608393721, -13.14518615778179544 ) ) ;
#7319 = ORIENTED_EDGE ( 'NONE', *, *, #14895, .F. ) ;
#7320 = CARTESIAN_POINT ( 'NONE',  ( 139.2950502721270425, 33.90585937608393863, 9.295050272127046043 ) ) ;
#7321 = CARTESIAN_POINT ( 'NONE',  ( 59.55508561352770158, 31.97109375108393436, 13.14518615778179722 ) ) ;
#7322 = CARTESIAN_POINT ( 'NONE',  ( 204.2950502721270425, 34.69960937608393436, 9.295050272127046043 ) ) ;
#7323 = VERTEX_POINT ( 'NONE', #5224 ) ;
#7324 = CARTESIAN_POINT ( 'NONE',  ( 99.99999999999998579, 123.1500000010924794, 2.066987299999980099 ) ) ;
#7325 = CARTESIAN_POINT ( 'NONE',  ( 4.925026783667639130, 49.99999999893164215, -12.67776588291819095 ) ) ;
#7326 = CARTESIAN_POINT ( 'NONE',  ( 97.92893218813451028, -4.999999999999989342, 5.312500002731184168 ) ) ;
#7327 = AXIS2_PLACEMENT_3D ( 'NONE', #8384, #21648, #15062 ) ;
#7328 = CARTESIAN_POINT ( 'NONE',  ( 139.5988444088204403, 37.62656250216787157, -9.598844408820458085 ) ) ;
#7329 = CARTESIAN_POINT ( 'NONE',  ( 99.99999999999998579, 118.4984768113314146, -47.62500000273119127 ) ) ;
#7330 = DIRECTION ( 'NONE',  ( -0.000000000000000000, -0.000000000000000000, -1.000000000000000000 ) ) ;
#7331 = CARTESIAN_POINT ( 'NONE',  ( -5.622872871577737186, 34.89804687716787157, 13.57481594606318254 ) ) ;
#7332 = CARTESIAN_POINT ( 'NONE',  ( 65.72387193802225624, 53.51529642094862282, 14.99999999999997868 ) ) ;
#7333 = EDGE_CURVE ( 'NONE', #11913, #4741, #18474, .T. ) ;
#7334 = CARTESIAN_POINT ( 'NONE',  ( 101.8468681455906903, -4.458734124999987891, 3.750000001365591640 ) ) ;
#7335 = VERTEX_POINT ( 'NONE', #27448 ) ;
#7336 = CARTESIAN_POINT ( 'NONE',  ( -13.17415721692276165, 36.00000000000000000, 0.03826467346021143745 ) ) ;
#7337 = CARTESIAN_POINT ( 'NONE',  ( 99.99999999999995737, 4.458734125000016313, 6.187500001365592084 ) ) ;
#7338 = FACE_OUTER_BOUND ( 'NONE', #5023, .T. ) ;
#7339 = CARTESIAN_POINT ( 'NONE',  ( 13.14518615778179544, 36.18789062608393436, -1.609821015232357215E-15 ) ) ;
#7340 = CARTESIAN_POINT ( 'NONE',  ( 102.0710678118655039, 94.68749999726880162, 4.999999999999940492 ) ) ;
#7341 = CARTESIAN_POINT ( 'NONE',  ( 78.14518615778179367, 33.16171875108393863, 5.444914386472293977 ) ) ;
#7342 = CARTESIAN_POINT ( 'NONE',  ( -5.622872871577767384, 40.15664062716787441, -13.57481594606315412 ) ) ;
#7343 = PLANE ( 'NONE',  #9853 ) ;
#7344 = CARTESIAN_POINT ( 'NONE',  ( 105.6631189606246153, 114.1144967660473242, -53.29999999453764303 ) ) ;
#7345 = CARTESIAN_POINT ( 'NONE',  ( -4.571591632531241345, 51.44262710532056815, 15.00000000000065548 ) ) ;
#7346 = FACE_OUTER_BOUND ( 'NONE', #20562, .T. ) ;
#7347 = CARTESIAN_POINT ( 'NONE',  ( 143.5748159460630404, 34.99726562500000426, 5.622872871577869525 ) ) ;
#7348 = ORIENTED_EDGE ( 'NONE', *, *, #25688, .F. ) ;
#7349 = VERTEX_POINT ( 'NONE', #20614 ) ;
#7350 = FACE_BOUND ( 'NONE', #23140, .T. ) ;
#7351 = CARTESIAN_POINT ( 'NONE',  ( 13.14518615778179544, 34.00507812608393721, -1.609821015232357215E-15 ) ) ;
#7352 = CARTESIAN_POINT ( 'NONE',  ( -9.598844408820454532, 33.26093750216787726, 9.598844408820459861 ) ) ;
#7353 = CARTESIAN_POINT ( 'NONE',  ( 94.99999999999995737, -2.071067811865466624, 10.18750000273118417 ) ) ;
#7354 = CARTESIAN_POINT ( 'NONE',  ( 124.5550856135277087, 32.76484375108393010, 13.14518615778179722 ) ) ;
#7355 = CARTESIAN_POINT ( 'NONE',  ( 51.42518405393695957, 32.31835937716786589, -5.622872871577873077 ) ) ;
#7356 = CARTESIAN_POINT ( 'NONE',  ( 104.9999999999999716, 80.56250000000004263, -2.071067811865491937 ) ) ;
#7357 = CARTESIAN_POINT ( 'NONE',  ( 5.444914386472302859, 37.62656250108393863, 13.14518615778179189 ) ) ;
#7358 = CARTESIAN_POINT ( 'NONE',  ( -13.14518615778179544, 33.60820312608393579, 0.000000000000000000 ) ) ;
#7359 = CARTESIAN_POINT ( 'NONE',  ( 101.7677669529663547, 124.0000000021849615, -1.767766952966370209 ) ) ;
#7360 = CARTESIAN_POINT ( 'NONE',  ( 95.00472066334981491, 116.8754121666685393, -54.17499999726882720 ) ) ;
#7361 = CARTESIAN_POINT ( 'NONE',  ( -13.57481594606304753, 38.66835937716786731, -5.622872871577873077 ) ) ;
#7362 = CARTESIAN_POINT ( 'NONE',  ( 102.0710678118654187, 82.43750000273119838, 5.000000000000011546 ) ) ;
#7363 = CARTESIAN_POINT ( 'NONE',  ( -13.57481594606304753, 31.52460937716787370, -5.622872871577872189 ) ) ;
#7364 = CARTESIAN_POINT ( 'NONE',  ( 97.50000000000000000, 124.1569999999781544, -1.035533905932742416 ) ) ;
#7365 = CARTESIAN_POINT ( 'NONE',  ( 98.53841926354351699, 124.4500000010924765, -1.461580736456474794 ) ) ;
#7366 = CARTESIAN_POINT ( 'NONE',  ( 106.9999999999999716, 112.2744378736303759, -51.39999999453765156 ) ) ;
#7367 = DIRECTION ( 'NONE',  ( 0.000000000000000000, 0.000000000000000000, 1.000000000000000000 ) ) ;
#7368 = CARTESIAN_POINT ( 'NONE',  ( 102.0669872999999797, 122.5500000010924850, -9.794112055954760458E-15 ) ) ;
#7369 = CARTESIAN_POINT ( 'NONE',  ( -5.622872871577873077, 35.59257812499999574, 13.57481594606304753 ) ) ;
#7370 = CARTESIAN_POINT ( 'NONE',  ( -4.972887739508807137, 36.00000000000002842, -12.48139679469879582 ) ) ;
#7371 = CARTESIAN_POINT ( 'NONE',  ( -5.444914386472297529, 33.45937500108394147, -13.14518615778179900 ) ) ;
#7372 = CARTESIAN_POINT ( 'NONE',  ( 5.444914386472297529, 33.95546875108393436, -13.14518615778179900 ) ) ;
#7373 = EDGE_CURVE ( 'NONE', #26723, #896, #21624, .T. ) ;
#7374 = CARTESIAN_POINT ( 'NONE',  ( -5.444914386472299306, 35.93984375108392726, 13.14518615778179722 ) ) ;
#7375 = CARTESIAN_POINT ( 'NONE',  ( 2.493653234604083739E-15, 36.53515625216787299, 13.57481594606304576 ) ) ;
#7376 = CARTESIAN_POINT ( 'NONE',  ( 94.99999999999995737, 1.387778780781445676E-14, 4.125000002731185056 ) ) ;
#7377 = DIRECTION ( 'NONE',  ( 0.000000000000000000, 1.000000000000000000, 0.000000000000000000 ) ) ;
#7378 = CARTESIAN_POINT ( 'NONE',  ( 78.14518615778179367, 33.80664062608393294, -1.609821015232357215E-15 ) ) ;
#7379 = EDGE_CURVE ( 'NONE', #22018, #1696, #19073, .T. ) ;
#7380 = CARTESIAN_POINT ( 'NONE',  ( 97.92893218813452449, 90.68750000000000000, 4.999999999999991118 ) ) ;
#7381 = CARTESIAN_POINT ( 'NONE',  ( 98.24352329449848753, 123.0000000000000426, -1.784664002384159565 ) ) ;
#7382 =( BOUNDED_CURVE ( )  B_SPLINE_CURVE ( 2, ( #7894, #16445, #5768, #1495, #27301, #12428, #1773, #14437, #14297 ),
 .UNSPECIFIED., .F., .T. ) 
 B_SPLINE_CURVE_WITH_KNOTS ( ( 3, 2, 2, 2, 3 ),
 ( 0.3541666666666666852, 0.3645833333333332593, 0.3749999999999998890, 0.3854166666666665741, 0.3958333333333331483 ),
 .UNSPECIFIED. ) 
 CURVE ( )  GEOMETRIC_REPRESENTATION_ITEM ( )  RATIONAL_B_SPLINE_CURVE ( ( 1.000000000000000000, 0.9238795325112867385, 1.000000000000000000, 0.9238795325112867385, 1.000000000000000000, 0.9238795325112867385, 1.000000000000000000, 0.9238795325112879597, 0.9999999999999987788 ) ) 
 REPRESENTATION_ITEM ( '' )  );
#7383 = CARTESIAN_POINT ( 'NONE',  ( -5.622872871577873077, 32.91367187499999858, -13.57481594606304753 ) ) ;
#7384 = CARTESIAN_POINT ( 'NONE',  ( 124.5550856135277087, 34.55078125108393294, 13.14518615778179722 ) ) ;
#7385 = ORIENTED_EDGE ( 'NONE', *, *, #5869, .T. ) ;
#7386 = CARTESIAN_POINT ( 'NONE',  ( 97.92893218813451028, 82.18750000000000000, 4.999999999999989342 ) ) ;
#7387 = CARTESIAN_POINT ( 'NONE',  ( 74.59884440882045453, 38.42031250216787441, -9.598844408820458085 ) ) ;
#7388 = CARTESIAN_POINT ( 'NONE',  ( 96.84719886470459471, 82.31250000136559208, -3.152801135295383084 ) ) ;
#7389 = CARTESIAN_POINT ( 'NONE',  ( 102.0710678118654613, 92.18749999999998579, -4.999999999999997335 ) ) ;
#7390 = CARTESIAN_POINT ( 'NONE',  ( 70.62287287157788285, 39.75976562716787299, 13.57481594606304576 ) ) ;
#7391 = EDGE_CURVE ( 'NONE', #27982, #8588, #15071, .T. ) ;
#7392 = CARTESIAN_POINT ( 'NONE',  ( 94.33688103937535629, 105.8855032339526758, -54.80000000000001847 ) ) ;
#7393 = CARTESIAN_POINT ( 'NONE',  ( 70.62287287157788285, 39.66054687500000142, 13.57481594606304576 ) ) ;
#7394 = CARTESIAN_POINT ( 'NONE',  ( -8.312177448680279460E-16, 38.51953125216787299, -13.57481594606304576 ) ) ;
#7395 = ORIENTED_EDGE ( 'NONE', *, *, #6004, .T. ) ;
#7396 = CYLINDRICAL_SURFACE ( 'NONE', #4900, 13.57481594606304398 ) ;
#7397 = VECTOR ( 'NONE', #15069, 1000.000000000000000 ) ;
#7398 = CARTESIAN_POINT ( 'NONE',  ( 94.99999999999995737, 1.387778780781445676E-14, 13.99999999999999822 ) ) ;
#7399 = ORIENTED_EDGE ( 'NONE', *, *, #5935, .F. ) ;
#7400 = CARTESIAN_POINT ( 'NONE',  ( 9.295050272127046043, 36.48554687608393721, -9.295050272127046043 ) ) ;
#7401 = CARTESIAN_POINT ( 'NONE',  ( 185.7049497278729575, 39.85898437608393152, 9.295050272127047819 ) ) ;
#7402 = CARTESIAN_POINT ( 'NONE',  ( 13.14518615778179722, 34.65000000108393152, -5.444914386472297529 ) ) ;
#7403 = PRODUCT ( 'Vacuum Distribution Tubing Harness', 'Vacuum Distribution Tubing Harness', '', ( #21095 ) ) ;
#7404 = DIRECTION ( 'NONE',  ( 0.000000000000000000, 0.000000000000000000, 1.000000000000000000 ) ) ;
#7405 = CARTESIAN_POINT ( 'NONE',  ( 139.2950502721270425, 40.25585937608393294, -9.295050272127046043 ) ) ;
#7406 = CARTESIAN_POINT ( 'NONE',  ( 13.14518615778179900, 36.43593750108392726, -5.444914386472297529 ) ) ;
#7407 = CYLINDRICAL_SURFACE ( 'NONE', #2685, 7.000000000000006217 ) ;
#7408 = CARTESIAN_POINT ( 'NONE',  ( 103.1528011352953484, 91.18749999863440792, 3.152801135295352886 ) ) ;
#7409 = CARTESIAN_POINT ( 'NONE',  ( 102.4999999999999716, 124.5500000000000114, 1.035533905932722876 ) ) ;
#7410 = EDGE_CURVE ( 'NONE', #21904, #19382, #27318, .T. ) ;
#7411 = DIRECTION ( 'NONE',  ( 0.000000000000000000, 0.000000000000000000, 1.000000000000000000 ) ) ;
#7412 = LINE ( 'NONE', #18401, #13632 ) ;
#7413 = CARTESIAN_POINT ( 'NONE',  ( 103.1528011352953342, 3.152801135295383084, 8.312500001365592084 ) ) ;
#7414 = CARTESIAN_POINT ( 'NONE',  ( 95.54126587499996504, -1.846868145590724986, 10.50000000136559208 ) ) ;
#7415 = CARTESIAN_POINT ( 'NONE',  ( 108.0825317500000011, 107.3738262389971538, -48.22500000273118559 ) ) ;
#7416 = CARTESIAN_POINT ( 'NONE',  ( 101.8468681455907330, 91.74999999863439371, -4.458734124999994997 ) ) ;
#7417 = CARTESIAN_POINT ( 'NONE',  ( 104.9999999999999716, 2.071067811865491937, 3.562499999999999556 ) ) ;
#7418 = CARTESIAN_POINT ( 'NONE',  ( 130.0000000000000000, -7.395377635281828788, -1.503427012513233026E-14 ) ) ;
#7419 = CARTESIAN_POINT ( 'NONE',  ( 9.295050272127046043, 34.89804687608393863, -9.295050272127046043 ) ) ;
#7420 = EDGE_CURVE ( 'NONE', #3329, #21904, #909, .T. ) ;
#7421 = EDGE_LOOP ( 'NONE', ( #7757, #22225, #341 ) ) ;
#7422 = CARTESIAN_POINT ( 'NONE',  ( 130.0000000000000000, 37.22968749999999716, 13.57481594606304576 ) ) ;
#7423 = CARTESIAN_POINT ( 'NONE',  ( -13.36000105192242060, 40.87597656304196647, 0.000000000000000000 ) ) ;
#7424 = DIRECTION ( 'NONE',  ( 0.000000000000000000, 0.000000000000000000, -1.000000000000000000 ) ) ;
#7425 = EDGE_CURVE ( 'NONE', #26599, #19519, #27462, .T. ) ;
#7426 = CARTESIAN_POINT ( 'NONE',  ( 185.7049497278729575, 36.68398437608392726, 9.295050272127047819 ) ) ;
#7427 = ORIENTED_EDGE ( 'NONE', *, *, #476, .F. ) ;
#7428 = CARTESIAN_POINT ( 'NONE',  ( 194.5539587432196527, 49.99999999978076204, -13.57776691409238268 ) ) ;
#7429 = CARTESIAN_POINT ( 'NONE',  ( 101.8468681455906903, 4.458734125000016313, 10.37500000136559208 ) ) ;
#7430 = VERTEX_POINT ( 'NONE', #22893 ) ;
#7431 = CARTESIAN_POINT ( 'NONE',  ( 93.46109445667491400, 114.7507929638356785, -53.57500000273119412 ) ) ;
#7432 = CARTESIAN_POINT ( 'NONE',  ( -5.444914386472299306, 36.73359375108393010, 13.14518615778179722 ) ) ;
#7433 = DIRECTION ( 'NONE',  ( 0.000000000000000000, -1.000000000000000000, 0.000000000000000000 ) ) ;
#7434 = DIRECTION ( 'NONE',  ( 0.000000000000000000, 0.000000000000000000, 1.000000000000000000 ) ) ;
#7435 = CARTESIAN_POINT ( 'NONE',  ( 135.4449143864723055, 38.71796875108393721, -13.14518615778179900 ) ) ;
#7436 = CARTESIAN_POINT ( 'NONE',  ( -9.295050272127044266, 37.67617187608393436, 9.295050272127047819 ) ) ;
#7437 = AXIS2_PLACEMENT_3D ( 'NONE', #23744, #8768, #17457 ) ;
#7438 = CARTESIAN_POINT ( 'NONE',  ( 5.444914386472297529, 33.95546875108393436, -13.14518615778179900 ) ) ;
#7439 = CARTESIAN_POINT ( 'NONE',  ( 101.8468681455907330, 94.37499999863440792, 4.458734124999979898 ) ) ;
#7440 = CARTESIAN_POINT ( 'NONE',  ( 62.47041600482873491, 49.99999999938352602, -13.34625891065891778 ) ) ;
#7441 = CARTESIAN_POINT ( 'NONE',  ( 108.0825317500000011, 112.6261737610028320, -48.27500000273119696 ) ) ;
#7442 = ORIENTED_EDGE ( 'NONE', *, *, #16267, .F. ) ;
#7443 = EDGE_LOOP ( 'NONE', ( #21571, #6631, #20758, #23705 ) ) ;
#7444 = CARTESIAN_POINT ( 'NONE',  ( 97.83688103937537051, 103.3426043859339103, -50.60000000000001563 ) ) ;
#7445 = CARTESIAN_POINT ( 'NONE',  ( -13.14518615778179189, 34.45156250108394147, 5.444914386472304635 ) ) ;
#7446 = CARTESIAN_POINT ( 'NONE',  ( 95.54126587499996504, 1.387778780781445676E-14, 5.687500001365591196 ) ) ;
#7447 = CARTESIAN_POINT ( 'NONE',  ( 78.14518615778180788, 36.93203125108394147, 5.444914386472293977 ) ) ;
#7448 = MANIFOLD_SOLID_BREP ( 'Thread1', #21742 ) ;
#7449 = ADVANCED_FACE ( 'NONE', ( #955 ), #7633, .F. ) ;
#7450 = CARTESIAN_POINT ( 'NONE',  ( 55.40115559117954547, 36.23750000216787726, -9.598844408820458085 ) ) ;
#7451 = CARTESIAN_POINT ( 'NONE',  ( 104.9999999999999716, 1.449011120738813565E-14, 2.499999999999998668 ) ) ;
#7452 = CARTESIAN_POINT ( 'NONE',  ( -13.14518615778179544, 35.19570312608393436, 0.000000000000000000 ) ) ;
#7453 = CARTESIAN_POINT ( 'NONE',  ( 102.0669872999999797, 122.5500000010924850, -9.794112055954760458E-15 ) ) ;
#7454 = CARTESIAN_POINT ( 'NONE',  ( 98.15313185440923860, 92.24999999863439371, 4.458734124999980786 ) ) ;
#7455 = CARTESIAN_POINT ( 'NONE',  ( 208.1451861577818079, 38.02343750108395426, -5.444914386472297529 ) ) ;
#7456 = CARTESIAN_POINT ( 'NONE',  ( 99.99999999999997158, 101.5015231886685854, -51.37499999726882294 ) ) ;
#7457 = ORIENTED_EDGE ( 'NONE', *, *, #16085, .T. ) ;
#7458 = CARTESIAN_POINT ( 'NONE',  ( -13.57481594606304576, 32.31835937499999289, 5.622872871577880183 ) ) ;
#7459 = CARTESIAN_POINT ( 'NONE',  ( -8.049105076161786076E-16, 34.79882812608393294, -13.14518615778179544 ) ) ;
#7460 = VERTEX_POINT ( 'NONE', #23724 ) ;
#7461 = CARTESIAN_POINT ( 'NONE',  ( 124.5550856135277087, 31.87187500108393223, -13.14518615778179900 ) ) ;
#7462 = CARTESIAN_POINT ( 'NONE',  ( 59.55508561352770158, 40.10703125108393152, 13.14518615778179722 ) ) ;
#7463 = LINE ( 'NONE', #1220, #9148 ) ;
#7464 = CARTESIAN_POINT ( 'NONE',  ( 189.5550856135277229, 35.34453125108393579, 13.14518615778179722 ) ) ;
#7465 = ORIENTED_EDGE ( 'NONE', *, *, #3251, .T. ) ;
#7466 = CARTESIAN_POINT ( 'NONE',  ( 99.99999999999995737, -4.999999999999990230, 13.25000000000000000 ) ) ;
#7467 = DIRECTION ( 'NONE',  ( -1.000000000000000000, 0.000000000000000000, 0.000000000000000000 ) ) ;
#7468 =( BOUNDED_CURVE ( )  B_SPLINE_CURVE ( 2, ( #6669, #22221, #272, #2700, #17647, #15355, #2420, #6955, #13208 ),
 .UNSPECIFIED., .F., .F. ) 
 B_SPLINE_CURVE_WITH_KNOTS ( ( 3, 2, 2, 2, 3 ),
 ( 0.4375000000000003331, 0.4479166666666669627, 0.4583333333333335369, 0.4687500000000001665, 0.4791666666666667962 ),
 .UNSPECIFIED. ) 
 CURVE ( )  GEOMETRIC_REPRESENTATION_ITEM ( )  RATIONAL_B_SPLINE_CURVE ( ( 0.9999999999999975575, 0.9238795325112891810, 1.000000000000000000, 0.9238795325112867385, 1.000000000000000000, 0.9238795325112867385, 1.000000000000000000, 0.9238795325112859613, 1.000000000000000888 ) ) 
 REPRESENTATION_ITEM ( '' )  );
#7469 = CARTESIAN_POINT ( 'NONE',  ( 135.6228728715778971, 38.17226562716786731, 13.57481594606304576 ) ) ;
#7470 = CARTESIAN_POINT ( 'NONE',  ( 95.00472066334981491, 116.8754121666685393, -45.42500000273118843 ) ) ;
#7471 = CARTESIAN_POINT ( 'NONE',  ( 51.42518405393695957, 40.25585937716787299, -5.622872871577872189 ) ) ;
#7472 = FACE_OUTER_BOUND ( 'NONE', #2752, .T. ) ;
#7473 = CARTESIAN_POINT ( 'NONE',  ( 65.44604125677763307, 49.99999999978076914, 13.57776691409234715 ) ) ;
#7474 = VERTEX_POINT ( 'NONE', #4199 ) ;
#7475 = ORIENTED_EDGE ( 'NONE', *, *, #8912, .F. ) ;
#7476 = SURFACE_STYLE_USAGE ( .BOTH. , #23305 ) ;
#7477 = CARTESIAN_POINT ( 'NONE',  ( 104.4587341249999639, 1.442382525525748735E-14, 3.937500001365591640 ) ) ;
#7478 = ORIENTED_EDGE ( 'NONE', *, *, #2880, .T. ) ;
#7479 = CARTESIAN_POINT ( 'NONE',  ( -2.086998648631069653, 36.00000000000000000, -13.31420566034952202 ) ) ;
#7480 = CARTESIAN_POINT ( 'NONE',  ( 104.4587341249999781, 1.846868145590750299, 8.000000001365592084 ) ) ;
#7481 = CARTESIAN_POINT ( 'NONE',  ( 195.0000000000000000, 38.02343749999999289, 13.57481594606304576 ) ) ;
#7482 = FACE_OUTER_BOUND ( 'NONE', #25796, .T. ) ;
#7483 = CARTESIAN_POINT ( 'NONE',  ( 51.85481384221820633, 32.02070312608393010, 0.000000000000000000 ) ) ;
#7484 = CARTESIAN_POINT ( 'NONE',  ( 99.99999999999995737, -4.999999999999990230, 5.249999999999999112 ) ) ;
#7485 = CARTESIAN_POINT ( 'NONE',  ( 106.5389055433251002, 105.2492070361643215, -48.32500000273119412 ) ) ;
#7486 = DIRECTION ( 'NONE',  ( 1.000000000000000000, -0.000000000000000000, 1.224646799147353207E-16 ) ) ;
#7487 = VECTOR ( 'NONE', #15972, 1000.000000000000000 ) ;
#7488 = CARTESIAN_POINT ( 'NONE',  ( 95.67376207875072680, 115.9545556584642867, -52.79999999453764303 ) ) ;
#7489 = CARTESIAN_POINT ( 'NONE',  ( 0.8765262653613452581, 51.45968077934942642, 14.99999999999965716 ) ) ;
#7490 = CARTESIAN_POINT ( 'NONE',  ( 139.5988444088204687, 40.50390624999999289, 9.598844408820456309 ) ) ;
#7491 = CARTESIAN_POINT ( 'NONE',  ( 124.3771271284221314, 35.59257812499999574, 13.57481594606304753 ) ) ;
#7492 = EDGE_LOOP ( 'NONE', ( #6441, #13510, #21444, #25657 ) ) ;
#7493 = CARTESIAN_POINT ( 'NONE',  ( 94.33688103937534208, 114.1144967660473242, -51.20000000000000995 ) ) ;
#7494 = CARTESIAN_POINT ( 'NONE',  ( 9.295050272127047819, 33.11210937608393579, 9.295050272127046043 ) ) ;
#7495 = CARTESIAN_POINT ( 'NONE',  ( 13.57481594606304576, 32.76484375216787015, -1.662435489736055892E-15 ) ) ;
#7496 =( REPRESENTATION_RELATIONSHIP ('NONE','NONE', #2411, #26810 ) REPRESENTATION_RELATIONSHIP_WITH_TRANSFORMATION ( #10237 )SHAPE_REPRESENTATION_RELATIONSHIP( ) );
#7497 = CARTESIAN_POINT ( 'NONE',  ( 102.0710678118654329, 5.000000000000018652, 6.812500002731185056 ) ) ;
#7498 = CARTESIAN_POINT ( 'NONE',  ( 116.8548138422182063, 34.94765625108392726, -5.444914386472297529 ) ) ;
#7499 = CARTESIAN_POINT ( 'NONE',  ( 59.55508561352770158, 39.61093750108393152, -13.14518615778179900 ) ) ;
#7500 = EDGE_LOOP ( 'NONE', ( #6558, #12302, #4917, #15550 ) ) ;
#7501 = EDGE_CURVE ( 'NONE', #27592, #27159, #23444, .T. ) ;
#7502 = CARTESIAN_POINT ( 'NONE',  ( 102.0710678118654329, 5.000000000000018652, 14.68749999999999822 ) ) ;
#7503 = CARTESIAN_POINT ( 'NONE',  ( 5.444914386472297529, 37.92421875108392726, -13.14518615778179900 ) ) ;
#7504 = CARTESIAN_POINT ( 'NONE',  ( 6.944426393311537993, 31.75150625057403175, -11.16113171639042356 ) ) ;
#7505 = CARTESIAN_POINT ( 'NONE',  ( 93.00000000000000000, 110.0000000000000000, -48.00000000000000711 ) ) ;
#7506 = CARTESIAN_POINT ( 'NONE',  ( 97.50236033167490746, 117.6869444889999841, -50.27499999726882152 ) ) ;
#7507 = VECTOR ( 'NONE', #11874, 999.9999999999998863 ) ;
#7508 = CARTESIAN_POINT ( 'NONE',  ( 9.598844408820459861, 38.22187500216787015, 9.598844408820456309 ) ) ;
#7509 = CARTESIAN_POINT ( 'NONE',  ( 99.99999999999998579, 129.0000000000000000, -12.50000000000002132 ) ) ;
#7510 = CARTESIAN_POINT ( 'NONE',  ( 143.4064236467344813, 36.00000000000000000, 1.227293221035692161 ) ) ;
#7511 = CARTESIAN_POINT ( 'NONE',  ( 99.99999999999998579, 124.8069999999781459, -2.499999999999997780 ) ) ;
#7512 = CARTESIAN_POINT ( 'NONE',  ( 101.4615807364564546, 123.4500000010924765, -1.461580736456474794 ) ) ;
#7513 = CARTESIAN_POINT ( 'NONE',  ( 195.0000000000000000, 39.21406249999999716, -13.57481594606304576 ) ) ;
#7514 =( BOUNDED_CURVE ( )  B_SPLINE_CURVE ( 2, ( #10853, #6587, #1776, #25698, #2333, #2049, #10991, #12712, #10440 ),
 .UNSPECIFIED., .F., .T. ) 
 B_SPLINE_CURVE_WITH_KNOTS ( ( 3, 2, 2, 2, 3 ),
 ( 0.5500000000000004885, 0.5750000000000003997, 0.6000000000000005329, 0.6250000000000005551, 0.6500000000000005773 ),
 .UNSPECIFIED. ) 
 CURVE ( )  GEOMETRIC_REPRESENTATION_ITEM ( )  RATIONAL_B_SPLINE_CURVE ( ( 0.9999999999999986677, 0.9238795325112880708, 1.000000000000000000, 0.9238795325112867385, 1.000000000000000000, 0.9238795325112867385, 1.000000000000000000, 0.9238795325112850731, 1.000000000000001776 ) ) 
 REPRESENTATION_ITEM ( '' )  );
#7515 = CARTESIAN_POINT ( 'NONE',  ( 189.3771271284221029, 39.66054687716787441, 13.57481594606302444 ) ) ;
#7516 = CARTESIAN_POINT ( 'NONE',  ( 195.0000000000000000, 38.91640625216786731, 13.57481594606304576 ) ) ;
#7517 = CARTESIAN_POINT ( 'NONE',  ( 9.598844408820459861, 34.94765624999999432, 9.598844408820456309 ) ) ;
#7518 = CARTESIAN_POINT ( 'NONE',  ( 2.493653234604083739E-15, 40.40468749999999432, 13.57481594606304576 ) ) ;
#7519 = CARTESIAN_POINT ( 'NONE',  ( 13.14518615778179900, 35.64218750108393152, -5.444914386472297529 ) ) ;
#7520 = CARTESIAN_POINT ( 'NONE',  ( 13.14518615778179900, 32.26875000108393721, -5.444914386472297529 ) ) ;
#7521 = CARTESIAN_POINT ( 'NONE',  ( -13.14518615778179544, 34.20351562608393436, 0.000000000000000000 ) ) ;
#7522 = CARTESIAN_POINT ( 'NONE',  ( 13.57481594606304931, 35.89023437716787868, 5.622872871577869525 ) ) ;
#7523 = CARTESIAN_POINT ( 'NONE',  ( -13.57481594606304576, 37.92421875216787441, 0.000000000000000000 ) ) ;
#7524 = CARTESIAN_POINT ( 'NONE',  ( 101.8468681455906903, 84.12500000136560629, -4.458734125000016313 ) ) ;
#7525 = CARTESIAN_POINT ( 'NONE',  ( 51.85481384221820633, 33.40976562608393863, 0.000000000000000000 ) ) ;
#7526 = DIRECTION ( 'NONE',  ( -0.8660254037844404840, 0.000000000000000000, 0.4999999999999967804 ) ) ;
#7527 = DIRECTION ( 'NONE',  ( -0.000000000000000000, 1.000000000000000000, -0.000000000000000000 ) ) ;
#7528 = CARTESIAN_POINT ( 'NONE',  ( 97.93301270000000613, 124.5500000010924850, -9.540979117872439019E-15 ) ) ;
#7529 = CARTESIAN_POINT ( 'NONE',  ( 5.622872871577878406, 33.31054687499999289, 13.57481594606304576 ) ) ;
#7530 = CARTESIAN_POINT ( 'NONE',  ( 106.5389055433250860, 114.7507929638356785, -54.67499999726882720 ) ) ;
#7531 = CARTESIAN_POINT ( 'NONE',  ( 124.5550856135277087, 32.96328125108393436, 13.14518615778179722 ) ) ;
#7532 = EDGE_LOOP ( 'NONE', ( #16291, #16269, #18731, #1759 ) ) ;
#7533 = CARTESIAN_POINT ( 'NONE',  ( 94.99999999999995737, 80.06250000000001421, 2.071067811865466624 ) ) ;
#7534 = VECTOR ( 'NONE', #10569, 1000.000000000000000 ) ;
#7535 = CARTESIAN_POINT ( 'NONE',  ( 0.000000000000000000, 1.000000000000000000, 0.000000000000000000 ) ) ;
#7536 = CARTESIAN_POINT ( 'NONE',  ( 104.4587341249999781, 82.87500000136560629, 1.846868145590721655 ) ) ;
#7537 = CARTESIAN_POINT ( 'NONE',  ( 95.00000000000000000, 91.43750000000001421, -2.071067811865479058 ) ) ;
#7538 = CARTESIAN_POINT ( 'NONE',  ( 130.0000000000000000, 38.81718749999999574, 13.57481594606304576 ) ) ;
#7539 = CARTESIAN_POINT ( 'NONE',  ( 104.9952793366501709, 103.1245878333314323, -48.92499999726882010 ) ) ;
#7540 = CARTESIAN_POINT ( 'NONE',  ( 208.1451861577817795, 32.16953125108393152, 5.444914386472293977 ) ) ;
#7541 = DIRECTION ( 'NONE',  ( 0.000000000000000000, 0.000000000000000000, -1.000000000000000000 ) ) ;
#7542 = CIRCLE ( 'NONE', #16183, 13.57481594606304398 ) ;
#7543 = ORIENTED_EDGE ( 'NONE', *, *, #25688, .T. ) ;
#7544 = CARTESIAN_POINT ( 'NONE',  ( 51.42518405393695957, 36.18789062499999432, -5.622872871577872189 ) ) ;
#7545 = CARTESIAN_POINT ( 'NONE',  ( 99.99999999999995737, -4.999999999999990230, 9.250000000000000000 ) ) ;
#7546 = ADVANCED_FACE ( 'NONE', ( #12580 ), #14726, .F. ) ;
#7547 = VERTEX_POINT ( 'NONE', #19442 ) ;
#7548 = CARTESIAN_POINT ( 'NONE',  ( -9.295050272127044266, 36.08867187608393579, 9.295050272127047819 ) ) ;
#7549 = CARTESIAN_POINT ( 'NONE',  ( 181.4251840539369596, 31.52460937716787370, -5.622872871577873077 ) ) ;
#7550 = CARTESIAN_POINT ( 'NONE',  ( -9.295050272127044266, 31.92148437608393508, 9.295050272127047819 ) ) ;
#7551 = CARTESIAN_POINT ( 'NONE',  ( 97.92893218813451028, 5.000000000000018652, 11.93750000273118772 ) ) ;
#7552 = FACE_OUTER_BOUND ( 'NONE', #23998, .T. ) ;
#7553 = DIRECTION ( 'NONE',  ( -1.000000000000000000, 0.000000000000000000, 0.000000000000000000 ) ) ;
#7554 = CARTESIAN_POINT ( 'NONE',  ( 135.4449143864723055, 32.36796875108393579, -13.14518615778179900 ) ) ;
#7555 = CARTESIAN_POINT ( 'NONE',  ( 95.54126587499999346, 92.74999999863439371, -1.846868145590737864 ) ) ;
#7556 = CARTESIAN_POINT ( 'NONE',  ( 102.0669872999999797, 123.5500000010924708, -9.794112055954760458E-15 ) ) ;
#7557 = DIRECTION ( 'NONE',  ( 0.000000000000000000, 0.000000000000000000, 1.000000000000000000 ) ) ;
#7558 = CARTESIAN_POINT ( 'NONE',  ( 2.493653234604083739E-15, 35.74140625216787015, 13.57481594606304576 ) ) ;
#7559 = CARTESIAN_POINT ( 'NONE',  ( 95.54126587499995082, 1.846868145590750077, 8.625000001365593860 ) ) ;
#7560 = CARTESIAN_POINT ( 'NONE',  ( 98.23223304703363112, 123.5000000000000000, 1.767766952966351557 ) ) ;
#7561 = CARTESIAN_POINT ( 'NONE',  ( 104.4587341249999781, 1.846868145590750521, 11.00000000136559208 ) ) ;
#7562 = CARTESIAN_POINT ( 'NONE',  ( 99.99999999999998579, 117.3602355696678501, -51.00000000546238255 ) ) ;
#7563 = CARTESIAN_POINT ( 'NONE',  ( 95.54126587499999346, 90.99999999863439371, -1.846868145590737864 ) ) ;
#7564 = CARTESIAN_POINT ( 'NONE',  ( 200.6228728715778118, 39.95820312499999716, -13.57481594606312036 ) ) ;
#7565 = DIRECTION ( 'NONE',  ( -0.000000000000000000, 1.000000000000000000, -0.000000000000000000 ) ) ;
#7566 = CARTESIAN_POINT ( 'NONE',  ( 2.414731522848535132E-15, 33.01289062608393721, 13.14518615778179544 ) ) ;
#7567 = ORIENTED_EDGE ( 'NONE', *, *, #13115, .T. ) ;
#7568 = FILL_AREA_STYLE ('',( #5591 ) ) ;
#7569 = EDGE_CURVE ( 'NONE', #15184, #12415, #12240, .T. ) ;
#7570 = CARTESIAN_POINT ( 'NONE',  ( -15.00000000000000000, 80.00000000000000000, 10.00000000000000000 ) ) ;
#7571 = CARTESIAN_POINT ( 'NONE',  ( 181.8548138422181921, 33.36015625108393579, -5.444914386472297529 ) ) ;
#7572 = ORIENTED_EDGE ( 'NONE', *, *, #21359, .T. ) ;
#7573 = VECTOR ( 'NONE', #22992, 1000.000000000000000 ) ;
#7574 = ADVANCED_FACE ( 'NONE', ( #21030 ), #12440, .T. ) ;
#7575 = CARTESIAN_POINT ( 'NONE',  ( 191.3635037532015986, 51.46815297079189122, -15.00000000000068745 ) ) ;
#7576 = CARTESIAN_POINT ( 'NONE',  ( 95.54126587499996504, 1.387778780781445676E-14, 10.68750000136559208 ) ) ;
#7577 = EDGE_CURVE ( 'NONE', #2045, #3877, #6139, .T. ) ;
#7578 = ORIENTED_EDGE ( 'NONE', *, *, #4113, .T. ) ;
#7579 = CARTESIAN_POINT ( 'NONE',  ( 97.50236033167492167, 117.6869444889999841, -45.77500000273119696 ) ) ;
#7580 = CARTESIAN_POINT ( 'NONE',  ( -9.295050272127046043, 37.27929687608393294, -9.295050272127046043 ) ) ;
#7581 = AXIS2_PLACEMENT_3D ( 'NONE', #1805, #3798, #15021 ) ;
#7582 = CARTESIAN_POINT ( 'NONE',  ( 181.4251840539369596, 39.56132812716787583, 5.622872871577880183 ) ) ;
#7583 = CARTESIAN_POINT ( 'NONE',  ( 13.57481594606304931, 38.96601562499999005, 5.622872871577868636 ) ) ;
#7584 = EDGE_CURVE ( 'NONE', #10198, #12623, #23162, .T. ) ;
#7585 = CARTESIAN_POINT ( 'NONE',  ( 120.7049497278729575, 38.27148437608393294, 9.295050272127047819 ) ) ;
#7586 = CARTESIAN_POINT ( 'NONE',  ( -9.295050272127046043, 39.06523437608392868, -9.295050272127046043 ) ) ;
#7587 = CARTESIAN_POINT ( 'NONE',  ( 9.295050272127046043, 40.45429687608393721, -9.295050272127046043 ) ) ;
#7588 = CARTESIAN_POINT ( 'NONE',  ( 96.84719886470463734, 91.18749999863440792, 3.152801135295351997 ) ) ;
#7589 = CARTESIAN_POINT ( 'NONE',  ( 99.99999999999998579, 90.00000000000000000, -6.938893903907228378E-15 ) ) ;
#7590 = CARTESIAN_POINT ( 'NONE',  ( 91.91746824999999887, 110.0000000000000000, -51.37500000273119127 ) ) ;
#7591 = EDGE_CURVE ( 'NONE', #10432, #15088, #6348, .T. ) ;
#7592 = EDGE_LOOP ( 'NONE', ( #1014, #4278, #13635, #18831 ) ) ;
#7593 = ORIENTED_EDGE ( 'NONE', *, *, #11866, .T. ) ;
#7594 = CARTESIAN_POINT ( 'NONE',  ( 9.598844408820456309, 38.42031250216787441, -9.598844408820458085 ) ) ;
#7595 = CARTESIAN_POINT ( 'NONE',  ( -5.444914386472299306, 36.13828125108393863, 13.14518615778179722 ) ) ;
#7596 = CARTESIAN_POINT ( 'NONE',  ( 104.4587341249999781, -1.846868145590721655, 5.125000001365592972 ) ) ;
#7597 = VECTOR ( 'NONE', #12584, 1000.000000000000000 ) ;
#7598 = CARTESIAN_POINT ( 'NONE',  ( 70.44491438647229131, 37.13046875108393152, -13.14518615778179722 ) ) ;
#7599 = FACE_OUTER_BOUND ( 'NONE', #182, .T. ) ;
#7600 = LINE ( 'NONE', #10006, #602 ) ;
#7601 = CARTESIAN_POINT ( 'NONE',  ( 104.9999999999999858, -2.071067811865442643, 2.437500000000000000 ) ) ;
#7602 = ORIENTED_EDGE ( 'NONE', *, *, #17472, .T. ) ;
#7603 = CARTESIAN_POINT ( 'NONE',  ( 5.444914386472302859, 33.85625000108393579, 13.14518615778179189 ) ) ;
#7604 = CARTESIAN_POINT ( 'NONE',  ( 101.7677669529663547, 123.2000000021849502, -1.767766952966370209 ) ) ;
#7605 = CARTESIAN_POINT ( 'NONE',  ( 95.54126587499999346, 94.12499999863439371, 1.846868145590722543 ) ) ;
#7606 = DIRECTION ( 'NONE',  ( 0.000000000000000000, 1.000000000000000000, 0.000000000000000000 ) ) ;
#7607 = CARTESIAN_POINT ( 'NONE',  ( 97.50236033167490746, 102.3130555110000159, -47.47499999726881725 ) ) ;
#7608 = EDGE_CURVE ( 'NONE', #1369, #20160, #13141, .T. ) ;
#7609 = CARTESIAN_POINT ( 'NONE',  ( 9.598844408820456309, 33.55859375000000000, -9.598844408820458085 ) ) ;
#7610 = CARTESIAN_POINT ( 'NONE',  ( 5.444914386472297529, 33.95546875108393436, -13.14518615778179900 ) ) ;
#7611 = ORIENTED_EDGE ( 'NONE', *, *, #20993, .F. ) ;
#7612 = CARTESIAN_POINT ( 'NONE',  ( 99.99999999999998579, 90.00000000000000000, -2.999999999999996447 ) ) ;
#7613 = CARTESIAN_POINT ( 'NONE',  ( 51.85481384221820633, 40.70234375108392300, -5.444914386472297529 ) ) ;
#7614 = CARTESIAN_POINT ( 'NONE',  ( 5.622872871577870413, 32.91367187716787157, -13.57481594606304753 ) ) ;
#7615 = CARTESIAN_POINT ( 'NONE',  ( 189.5550856135277229, 33.45937500108394147, -13.14518615778179900 ) ) ;
#7616 = ORIENTED_EDGE ( 'NONE', *, *, #25654, .T. ) ;
#7617 = CARTESIAN_POINT ( 'NONE',  ( 74.18017581364799184, 50.00000000000000000, -9.999999999999998224 ) ) ;
#7618 = EDGE_CURVE ( 'NONE', #8183, #21036, #1760, .T. ) ;
#7619 = CARTESIAN_POINT ( 'NONE',  ( 6.450879342659026960, 50.00000000106836495, -11.97362904075607482 ) ) ;
#7620 = CARTESIAN_POINT ( 'NONE',  ( 67.12981065842747341, 36.02027164734404607, -13.57481594606306352 ) ) ;
#7621 = VECTOR ( 'NONE', #28021, 999.9999999999998863 ) ;
#7622 = EDGE_CURVE ( 'NONE', #25304, #12136, #16717, .T. ) ;
#7623 = CARTESIAN_POINT ( 'NONE',  ( 135.6228728715778971, 37.37851562716787157, 13.57481594606304576 ) ) ;
#7624 = CARTESIAN_POINT ( 'NONE',  ( 93.00000000000000000, 112.2744378736303190, -44.60000000546238397 ) ) ;
#7625 = CARTESIAN_POINT ( 'NONE',  ( 84.99999999999998579, 125.0000000000000000, 14.99999999999999112 ) ) ;
#7626 = CARTESIAN_POINT ( 'NONE',  ( 200.4449143864723055, 39.41250000108393436, 13.14518615778179189 ) ) ;
#7627 = ORIENTED_EDGE ( 'NONE', *, *, #8158, .F. ) ;
#7628 = CARTESIAN_POINT ( 'NONE',  ( 101.8468681455906903, 4.458734125000016313, 13.37500000136559386 ) ) ;
#7629 = CARTESIAN_POINT ( 'NONE',  ( 0.3745404134779373173, 36.00000000000003553, -13.51869779562201757 ) ) ;
#7630 = CARTESIAN_POINT ( 'NONE',  ( 0.000000000000000000, -1.000000000000001998, 0.000000000000000000 ) ) ;
#7631 = CARTESIAN_POINT ( 'NONE',  ( -4.374022130818334020, 36.00000000000000711, 12.40367315690567018 ) ) ;
#7632 = CARTESIAN_POINT ( 'NONE',  ( 59.55508561352770158, 31.87187500108393223, -13.14518615778179900 ) ) ;
#7633 = CYLINDRICAL_SURFACE ( 'NONE', #4995, 7.000000000000006217 ) ;
#7634 = CARTESIAN_POINT ( 'NONE',  ( 95.00472066334982912, 103.1245878333314323, -44.82500000273117990 ) ) ;
#7635 = CARTESIAN_POINT ( 'NONE',  ( 9.598844408820459861, 40.50390624999999289, 9.598844408820456309 ) ) ;
#7636 = LINE ( 'NONE', #9209, #26683 ) ;
#7637 = CARTESIAN_POINT ( 'NONE',  ( 2.024627725537271772, 50.00000000050963678, 13.43320860980897535 ) ) ;
#7638 = FACE_OUTER_BOUND ( 'NONE', #12884, .T. ) ;
#7639 = CARTESIAN_POINT ( 'NONE',  ( 116.4251840539369454, 33.80664062500000000, -5.622872871577873077 ) ) ;
#7640 = ORIENTED_EDGE ( 'NONE', *, *, #21540, .T. ) ;
#7641 = ORIENTED_EDGE ( 'NONE', *, *, #10, .T. ) ;
#7642 = CARTESIAN_POINT ( 'NONE',  ( 112.9999999999999858, 97.00000000000000000, 14.99999999999999467 ) ) ;
#7643 = CARTESIAN_POINT ( 'NONE',  ( 9.295050272127046043, 32.51679687608393721, -9.295050272127046043 ) ) ;
#7644 = CARTESIAN_POINT ( 'NONE',  ( 5.622872871577871301, 34.50117187716788436, -13.57481594606304753 ) ) ;
#7645 =( BOUNDED_CURVE ( )  B_SPLINE_CURVE ( 2, ( #9947, #18661, #7387, #1006, #2844, #9675, #7823, #5126, #16516 ),
 .UNSPECIFIED., .F., .F. ) 
 B_SPLINE_CURVE_WITH_KNOTS ( ( 3, 2, 2, 2, 3 ),
 ( 0.1875000000000001388, 0.1979166666666667407, 0.2083333333333333703, 0.2187499999999999722, 0.2291666666666665741 ),
 .UNSPECIFIED. ) 
 CURVE ( )  GEOMETRIC_REPRESENTATION_ITEM ( )  RATIONAL_B_SPLINE_CURVE ( ( 0.9999999999999990008, 0.9238795325112877377, 1.000000000000000000, 0.9238795325112867385, 1.000000000000000000, 0.9238795325112867385, 1.000000000000000000, 0.9238795325112872936, 0.9999999999999994449 ) ) 
 REPRESENTATION_ITEM ( '' )  );
#7646 = CARTESIAN_POINT ( 'NONE',  ( 102.0710678118654329, -4.999999999999989342, 6.437500002731185056 ) ) ;
#7647 = CARTESIAN_POINT ( 'NONE',  ( 116.8548138422182063, 31.77265625108393365, -5.444914386472297529 ) ) ;
#7648 = CARTESIAN_POINT ( 'NONE',  ( 70.44491438647230552, 40.00781250108393294, 13.14518615778179189 ) ) ;
#7649 = MANIFOLD_SOLID_BREP ( 'Thread1', #14440 ) ;
#7650 = CARTESIAN_POINT ( 'NONE',  ( 2.493653234604083739E-15, 37.32890625216786873, 13.57481594606304576 ) ) ;
#7651 = CARTESIAN_POINT ( 'NONE',  ( 2.414731522848535132E-15, 38.37070312608393152, 13.14518615778179544 ) ) ;
#7652 = CARTESIAN_POINT ( 'NONE',  ( 0.000000000000000000, 10.00000000000000000, 19.22649730810373470 ) ) ;
#7653 = CARTESIAN_POINT ( 'NONE',  ( 65.00000000000000000, 37.62656249999999858, -13.57481594606304576 ) ) ;
#7654 = CARTESIAN_POINT ( 'NONE',  ( 108.0825317500000011, 110.0000000000000000, -50.87499999726882294 ) ) ;
#7655 = CARTESIAN_POINT ( 'NONE',  ( 208.5748159460630688, 40.55351562499999574, 5.622872871577868636 ) ) ;
#7656 = CARTESIAN_POINT ( 'NONE',  ( -13.14518615778179544, 40.55351562608393579, 0.000000000000000000 ) ) ;
#7657 = CARTESIAN_POINT ( 'NONE',  ( 219.9999999999999716, 55.00000000000000000, -15.00000000000000000 ) ) ;
#7658 = CARTESIAN_POINT ( 'NONE',  ( -15.00000000000000000, 75.00000000000000000, 10.00000000000000000 ) ) ;
#7659 = CIRCLE ( 'NONE', #27256, 0.5000000000000086597 ) ;
#7660 = CARTESIAN_POINT ( 'NONE',  ( 107.0000000000000000, 110.0000000000000000, -51.49999999453763877 ) ) ;
#7661 = CARTESIAN_POINT ( 'NONE',  ( 102.1631189606246295, 103.3426043859339103, -47.40000000000000568 ) ) ;
#7662 = CARTESIAN_POINT ( 'NONE',  ( 0.000000000000000000, 50.00000000000000000, 0.000000000000000000 ) ) ;
#7663 = FACE_OUTER_BOUND ( 'NONE', #6981, .T. ) ;
#7664 = CARTESIAN_POINT ( 'NONE',  ( -8.312177448680279460E-16, 35.24531249999999716, -13.57481594606304576 ) ) ;
#7665 = CARTESIAN_POINT ( 'NONE',  ( 130.0000000000000000, 50.00000000000000000, -13.57481594606305997 ) ) ;
#7666 = CARTESIAN_POINT ( 'NONE',  ( 13.57481594606304576, 39.80937499999999574, -1.662435489736055892E-15 ) ) ;
#7667 = CARTESIAN_POINT ( 'NONE',  ( -9.295050272127046043, 31.72304687608393081, -9.295050272127046043 ) ) ;
#7668 = CARTESIAN_POINT ( 'NONE',  ( 198.8783852973912474, 32.03609435653363136, -13.57481594606304576 ) ) ;
#7669 = CARTESIAN_POINT ( 'NONE',  ( 5.622872871577878406, 37.37851562716787157, 13.57481594606304576 ) ) ;
#7670 = CARTESIAN_POINT ( 'NONE',  ( 103.1528011352953342, 84.06250000136560629, -3.152801135295383084 ) ) ;
#7671 = CARTESIAN_POINT ( 'NONE',  ( 55.70494972787295751, 40.65273437608393436, -9.295050272127046043 ) ) ;
#7672 = FACE_OUTER_BOUND ( 'NONE', #20318, .T. ) ;
#7673 = CYLINDRICAL_SURFACE ( 'NONE', #21409, 11.57481594606304398 ) ;
#7674 = CARTESIAN_POINT ( 'NONE',  ( 99.14382582708707048, 124.4000000010924794, -2.066987299999999195 ) ) ;
#7675 = CARTESIAN_POINT ( 'NONE',  ( 9.598844408820459861, 32.56640625000000000, 9.598844408820456309 ) ) ;
#7676 = CARTESIAN_POINT ( 'NONE',  ( 102.4976396683250783, 102.3130555110000159, -55.27499999726882152 ) ) ;
#7677 = CARTESIAN_POINT ( 'NONE',  ( 130.0000000000000000, 34.20351562608394147, -13.14518615778179544 ) ) ;
#7678 = ORIENTED_EDGE ( 'NONE', *, *, #14071, .T. ) ;
#7679 = CARTESIAN_POINT ( 'NONE',  ( 135.6228728715777834, 37.67617187716787441, -13.57481594606313990 ) ) ;
#7680 = DIRECTION ( 'NONE',  ( 0.000000000000000000, 0.000000000000000000, 1.000000000000000000 ) ) ;
#7681 = CARTESIAN_POINT ( 'NONE',  ( 98.15313185440925281, 84.25000000136559208, -4.458734125000016313 ) ) ;
#7682 = CARTESIAN_POINT ( 'NONE',  ( 95.00000000000000000, 92.56250000000000000, 2.071067811865463959 ) ) ;
#7683 = AXIS2_PLACEMENT_3D ( 'NONE', #21070, #3688, #12481 ) ;
#7684 = VECTOR ( 'NONE', #12120, 1000.000000000000000 ) ;
#7685 = CARTESIAN_POINT ( 'NONE',  ( 99.99999999999997158, 118.4984768113314004, -48.12499999726881583 ) ) ;
#7686 = CARTESIAN_POINT ( 'NONE',  ( 181.8548138422181921, 31.77265625108393365, -5.444914386472297529 ) ) ;
#7687 = VECTOR ( 'NONE', #10929, 1000.000000000000000 ) ;
#7688 = CARTESIAN_POINT ( 'NONE',  ( -13.57481594606304576, 38.71796875216787726, 0.000000000000000000 ) ) ;
#7689 = VERTEX_POINT ( 'NONE', #12698 ) ;
#7690 = CARTESIAN_POINT ( 'NONE',  ( 104.9999999999999716, 1.449011120738813565E-14, 10.49999999999999822 ) ) ;
#7691 = ORIENTED_EDGE ( 'NONE', *, *, #4785, .T. ) ;
#7692 =( BOUNDED_CURVE ( )  B_SPLINE_CURVE ( 2, ( #15810, #19666, #723, #2720, #11096, #6686, #17953, #9396, #4710 ),
 .UNSPECIFIED., .F., .T. ) 
 B_SPLINE_CURVE_WITH_KNOTS ( ( 3, 2, 2, 2, 3 ),
 ( 0.8500000000000007550, 0.8750000000000008882, 0.9000000000000009104, 0.9250000000000009326, 0.9500000000000009548 ),
 .UNSPECIFIED. ) 
 CURVE ( )  GEOMETRIC_REPRESENTATION_ITEM ( )  RATIONAL_B_SPLINE_CURVE ( ( 0.9999999999999976685, 0.9238795325112890700, 1.000000000000000000, 0.9238795325112867385, 1.000000000000000000, 0.9238795325112867385, 1.000000000000000000, 0.9238795325112837409, 1.000000000000003109 ) ) 
 REPRESENTATION_ITEM ( '' )  );
#7693 = CARTESIAN_POINT ( 'NONE',  ( 5.444914386472302859, 33.06250000108393294, 13.14518615778179189 ) ) ;
#7694 = CARTESIAN_POINT ( 'NONE',  ( 204.5988444088204403, 32.86406250216787583, -9.598844408820458085 ) ) ;
#7695 = CYLINDRICAL_SURFACE ( 'NONE', #21708, 13.57481594606304398 ) ;
#7696 = FACE_OUTER_BOUND ( 'NONE', #25034, .T. ) ;
#7697 = CARTESIAN_POINT ( 'NONE',  ( 143.1451861577818363, 40.10703125108393152, 5.444914386472293977 ) ) ;
#7698 = CARTESIAN_POINT ( 'NONE',  ( -13.14518615778179900, 32.76484375108393010, -5.444914386472297529 ) ) ;
#7699 = FACE_OUTER_BOUND ( 'NONE', #10574, .T. ) ;
#7700 = CARTESIAN_POINT ( 'NONE',  ( 65.00000000000000000, 32.46718749999999432, 13.57481594606304576 ) ) ;
#7701 = CARTESIAN_POINT ( 'NONE',  ( 99.99999999999998579, 124.7999999999999972, -2.499999999999997780 ) ) ;
#7702 = CARTESIAN_POINT ( 'NONE',  ( 181.4251840539369596, 39.41249999999999432, 0.000000000000000000 ) ) ;
#7703 = CARTESIAN_POINT ( 'NONE',  ( 118.7351811978182781, 36.00000000000000000, 6.828991891054703167 ) ) ;
#7704 = CARTESIAN_POINT ( 'NONE',  ( 101.8468681455906903, -4.458734124999987891, 9.000000001365593860 ) ) ;
#7705 = DIRECTION ( 'NONE',  ( 1.000000000000000000, 0.000000000000000000, 0.000000000000000000 ) ) ;
#7706 = EDGE_CURVE ( 'NONE', #2793, #11153, #7712, .T. ) ;
#7707 = CARTESIAN_POINT ( 'NONE',  ( 95.54126587499996504, -1.846868145590724986, 9.500000001365593860 ) ) ;
#7708 = CARTESIAN_POINT ( 'NONE',  ( 97.83688103937537051, 103.3426043859339103, -48.10000000546237686 ) ) ;
#7709 = MECHANICAL_DESIGN_GEOMETRIC_PRESENTATION_REPRESENTATION (  '', ( #14962 ), #6330 ) ;
#7710 = CARTESIAN_POINT ( 'NONE',  ( 101.8468681455907330, 95.37499999863440792, 4.458734124999979898 ) ) ;
#7711 = CARTESIAN_POINT ( 'NONE',  ( 99.99999999999995737, -4.999999999999990230, 4.249999999999998224 ) ) ;
#7712 = CIRCLE ( 'NONE', #11321, 13.57481594606304398 ) ;
#7713 = CARTESIAN_POINT ( 'NONE',  ( 106.5389055433250860, 105.2492070361643215, -52.82499999726881867 ) ) ;
#7714 = CARTESIAN_POINT ( 'NONE',  ( 13.14518615778179900, 33.26093750108393721, -5.444914386472297529 ) ) ;
#7715 = VERTEX_POINT ( 'NONE', #21136 ) ;
#7716 = CARTESIAN_POINT ( 'NONE',  ( 116.4251840539369738, 37.08085937499999574, 5.622872871577880183 ) ) ;
#7717 = CARTESIAN_POINT ( 'NONE',  ( 94.99999999999995737, 1.387778780781445676E-14, 34.79898987322334136 ) ) ;
#7718 = CARTESIAN_POINT ( 'NONE',  ( 204.2950502721270425, 33.70742187608393436, 9.295050272127046043 ) ) ;
#7719 = ORIENTED_EDGE ( 'NONE', *, *, #9595, .T. ) ;
#7720 = CARTESIAN_POINT ( 'NONE',  ( 198.7165341137897485, 51.46663580899081580, -15.00000000000000178 ) ) ;
#7721 = CARTESIAN_POINT ( 'NONE',  ( 103.1528011352953342, 3.152801135295383084, 8.312500001365592084 ) ) ;
#7722 = ORIENTED_EDGE ( 'NONE', *, *, #15580, .T. ) ;
#7723 = CARTESIAN_POINT ( 'NONE',  ( 97.50236033167492167, 102.3130555110000159, -46.97500000273119269 ) ) ;
#7724 = CARTESIAN_POINT ( 'NONE',  ( 13.14518615778179900, 33.85625000108393579, -5.444914386472297529 ) ) ;
#7725 = CARTESIAN_POINT ( 'NONE',  ( 195.0000000000000000, 39.31328125216787583, -13.57481594606304576 ) ) ;
#7726 = CARTESIAN_POINT ( 'NONE',  ( -8.049105076161786076E-16, 37.97382812608393721, -13.14518615778179544 ) ) ;
#7727 = VECTOR ( 'NONE', #11053, 1000.000000000000000 ) ;
#7728 = CARTESIAN_POINT ( 'NONE',  ( -8.049105076161786076E-16, 38.96601562608393721, -13.14518615778179544 ) ) ;
#7729 = CARTESIAN_POINT ( 'NONE',  ( 13.14518615778179900, 32.26875000108393721, -5.444914386472297529 ) ) ;
#7730 = CARTESIAN_POINT ( 'NONE',  ( 96.84719886470463734, 91.93749999863440792, -3.152801135295366208 ) ) ;
#7731 = CYLINDRICAL_SURFACE ( 'NONE', #19138, 11.57481594606304398 ) ;
#7732 = AXIS2_PLACEMENT_3D ( 'NONE', #5294, #20547, #20250 ) ;
#7733 = ORIENTED_EDGE ( 'NONE', *, *, #22456, .F. ) ;
#7734 = CARTESIAN_POINT ( 'NONE',  ( 0.000000000000000000, 50.00000000000000000, 0.000000000000000000 ) ) ;
#7735 = CARTESIAN_POINT ( 'NONE',  ( -8.049105076161786076E-16, 34.20351562608394147, -13.14518615778179544 ) ) ;
#7736 = CARTESIAN_POINT ( 'NONE',  ( 95.54126587499996504, 1.846868145590750077, 8.625000001365592084 ) ) ;
#7737 = ADVANCED_FACE ( 'NONE', ( #1902 ), #1483, .T. ) ;
#7738 = CARTESIAN_POINT ( 'NONE',  ( 103.1528011352953342, 82.31250000136559208, -3.152801135295383084 ) ) ;
#7739 = CARTESIAN_POINT ( 'NONE',  ( 94.99999999999995737, 2.071067811865491493, 8.062500002731185944 ) ) ;
#7740 = CARTESIAN_POINT ( 'NONE',  ( 13.57481594606304931, 39.06523437716786873, 5.622872871577868636 ) ) ;
#7741 = ORIENTED_EDGE ( 'NONE', *, *, #11083, .T. ) ;
#7742 = EDGE_CURVE ( 'NONE', #24651, #6493, #23623, .T. ) ;
#7743 = CARTESIAN_POINT ( 'NONE',  ( -5.444914386472297529, 35.84062500108394289, -13.14518615778179722 ) ) ;
#7744 = CARTESIAN_POINT ( 'NONE',  ( 99.99999999999998579, 123.3000000021849587, -2.499999999999997780 ) ) ;
#7745 = CARTESIAN_POINT ( 'NONE',  ( 95.54126587500000767, 95.06249999863440792, -7.484931351350258973E-15 ) ) ;
#7746 = LINE ( 'NONE', #18853, #7279 ) ;
#7747 = CARTESIAN_POINT ( 'NONE',  ( 99.99999999999997158, 101.5015231886685854, -49.37499999726882294 ) ) ;
#7748 = VECTOR ( 'NONE', #12727, 1000.000000000000000 ) ;
#7749 = CARTESIAN_POINT ( 'NONE',  ( 99.99999999999998579, 138.0000000000000000, -5.204170427930421283E-15 ) ) ;
#7750 = CARTESIAN_POINT ( 'NONE',  ( -5.444914386472299306, 31.97109375108393436, 13.14518615778179722 ) ) ;
#7751 = ORIENTED_EDGE ( 'NONE', *, *, #23185, .F. ) ;
#7752 = DIRECTION ( 'NONE',  ( -1.000000000000000000, 0.000000000000000000, 0.000000000000000000 ) ) ;
#7753 = CARTESIAN_POINT ( 'NONE',  ( 59.55508561352770158, 36.93203125108394147, 13.14518615778179722 ) ) ;
#7754 = DIRECTION ( 'NONE',  ( -0.000000000000000000, -1.000000000000000000, -0.000000000000000000 ) ) ;
#7755 = EDGE_CURVE ( 'NONE', #16160, #20673, #26255, .T. ) ;
#7756 = FACE_OUTER_BOUND ( 'NONE', #24433, .T. ) ;
#7757 = ORIENTED_EDGE ( 'NONE', *, *, #446, .T. ) ;
#7758 = CARTESIAN_POINT ( 'NONE',  ( 102.0710678118654329, 5.000000000000018652, 1.812500002731185056 ) ) ;
#7759 = AXIS2_PLACEMENT_3D ( 'NONE', #6802, #15487, #13342 ) ;
#7760 = CARTESIAN_POINT ( 'NONE',  ( 1.014130826074231884, 51.45790058219387930, -14.99999999999932321 ) ) ;
#7761 = CARTESIAN_POINT ( 'NONE',  ( 201.0790800205188589, 54.65154858643461466, 14.99999999999994671 ) ) ;
#7762 = CARTESIAN_POINT ( 'NONE',  ( 116.4251840539369454, 38.66835937716786731, -5.622872871577873077 ) ) ;
#7763 = CARTESIAN_POINT ( 'NONE',  ( 104.9999999999999716, -2.071067811865462627, 7.437500000000000000 ) ) ;
#7764 = DIRECTION ( 'NONE',  ( 0.000000000000000000, 1.000000000000000000, -1.156482317317871478E-16 ) ) ;
#7765 = CARTESIAN_POINT ( 'NONE',  ( 208.1451861577817795, 38.81718750108393579, -5.444914386472297529 ) ) ;
#7766 = ADVANCED_FACE ( 'NONE', ( #2177 ), #4453, .T. ) ;
#7767 = ORIENTED_EDGE ( 'NONE', *, *, #27520, .T. ) ;
#7768 = AXIS2_PLACEMENT_3D ( 'NONE', #20115, #13384, #15534 ) ;
#7769 = CARTESIAN_POINT ( 'NONE',  ( 99.99999999999995737, 4.458734125000016313, 1.187500001365592750 ) ) ;
#7770 = CARTESIAN_POINT ( 'NONE',  ( -5.622872871577920151, 35.69179687716787441, 13.57481594606300135 ) ) ;
#7771 = CARTESIAN_POINT ( 'NONE',  ( 104.9999999999999858, 91.00000000000000000, -6.938893903907228378E-15 ) ) ;
#7772 = PLANE ( 'NONE',  #9709 ) ;
#7773 = CARTESIAN_POINT ( 'NONE',  ( 55.70494972787295751, 32.11992187608393579, 9.295050272127047819 ) ) ;
#7774 = CARTESIAN_POINT ( 'NONE',  ( 0.000000000000000000, 36.00000000000000000, 0.000000000000000000 ) ) ;
#7775 = CARTESIAN_POINT ( 'NONE',  ( -5.444914386472297529, 39.80937500108392868, -13.14518615778179900 ) ) ;
#7777 = LINE ( 'NONE', #12310, #19119 ) ;
#7776 = COLOUR_RGB ( '', 0.72549020, 0.75294118, 0.79215686) ;
#7778 = CARTESIAN_POINT ( 'NONE',  ( 5.364947964714800399, 36.00000000000002842, 12.09311862596063492 ) ) ;
#7779 = CARTESIAN_POINT ( 'NONE',  ( -15.00000000000000000, 55.00000000000000000, 10.00000000000000000 ) ) ;
#7780 = CARTESIAN_POINT ( 'NONE',  ( 120.4011555911795455, 33.95546874999999432, 9.598844408820459861 ) ) ;
#7781 = EDGE_CURVE ( 'NONE', #20441, #14776, #26768, .T. ) ;
#7782 = ORIENTED_EDGE ( 'NONE', *, *, #10011, .T. ) ;
#7783 = DIRECTION ( 'NONE',  ( 1.000000000000000000, 0.000000000000000000, -2.385244779468110248E-16 ) ) ;
#7784 = UNCERTAINTY_MEASURE_WITH_UNIT (LENGTH_MEASURE( 1.000000000000000082E-05 ), #5640, 'distance_accuracy_value', 'NONE');
#7785 = CARTESIAN_POINT ( 'NONE',  ( -13.57481594606304576, 38.66835937499999432, 5.622872871577880183 ) ) ;
#7786 = CARTESIAN_POINT ( 'NONE',  ( 9.598844408820456309, 32.07031250216787299, -9.598844408820458085 ) ) ;
#7787 = CARTESIAN_POINT ( 'NONE',  ( 97.92893218813451028, 5.000000000000018652, 6.937500002731185944 ) ) ;
#7788 = CARTESIAN_POINT ( 'NONE',  ( 116.8548138422182205, 40.75195312608393294, 0.000000000000000000 ) ) ;
#7789 = CARTESIAN_POINT ( 'NONE',  ( 74.29505027212704249, 39.46210937608393010, -9.295050272127046043 ) ) ;
#7790 = VECTOR ( 'NONE', #8028, 1000.000000000000000 ) ;
#7791 = ORIENTED_EDGE ( 'NONE', *, *, #11098, .T. ) ;
#7792 = CARTESIAN_POINT ( 'NONE',  ( 60.21996080114833916, 35.99999999999998579, 12.25280873422828876 ) ) ;
#7793 = CARTESIAN_POINT ( 'NONE',  ( -13.14518615778179900, 38.91640625108393436, -5.444914386472297529 ) ) ;
#7794 = CARTESIAN_POINT ( 'NONE',  ( 101.7677669529663547, 123.8000000021849587, 1.767766952966350891 ) ) ;
#7795 = DIRECTION ( 'NONE',  ( 0.000000000000000000, 0.000000000000000000, -1.000000000000000000 ) ) ;
#7796 = CARTESIAN_POINT ( 'NONE',  ( 91.91746824999998466, 110.0000000000000000, -53.87499999726882294 ) ) ;
#7797 = CARTESIAN_POINT ( 'NONE',  ( 195.0000000000000000, 40.40468749999999432, 13.57481594606304576 ) ) ;
#7798 = DIRECTION ( 'NONE',  ( -0.000000000000000000, -1.000000000000000000, -0.000000000000000000 ) ) ;
#7799 = CYLINDRICAL_SURFACE ( 'NONE', #17918, 13.57481594606304398 ) ;
#7800 = CARTESIAN_POINT ( 'NONE',  ( 102.4999999999999858, 122.9813376334432604, 0.3865102666887284544 ) ) ;
#7801 = CARTESIAN_POINT ( 'NONE',  ( 100.8561741729129153, 123.7000000010924765, -2.066987299999999195 ) ) ;
#7802 = CARTESIAN_POINT ( 'NONE',  ( 116.9040934463640156, 36.00000000000000000, 1.137167824541468031 ) ) ;
#7803 = FACE_OUTER_BOUND ( 'NONE', #22872, .T. ) ;
#7804 = CARTESIAN_POINT ( 'NONE',  ( 95.54126587499995082, 1.846868145590750077, 14.37500000136559386 ) ) ;
#7805 = DIRECTION ( 'NONE',  ( 5.782411586589358625E-17, -0.000000000000000000, 1.000000000000000000 ) ) ;
#7806 = VERTEX_POINT ( 'NONE', #9007 ) ;
#7807 = CARTESIAN_POINT ( 'NONE',  ( -6.470563696665745823, 36.00000000000002132, -11.78199955157067080 ) ) ;
#7808 = CARTESIAN_POINT ( 'NONE',  ( -5.622872871577873077, 40.05742187499999574, -13.57481594606304753 ) ) ;
#7809 = CARTESIAN_POINT ( 'NONE',  ( 3.755639919285892248, 31.58960996655074993, -13.14518615778179544 ) ) ;
#7810 = CARTESIAN_POINT ( 'NONE',  ( 13.14518615778179544, 32.21914062608393436, -1.609821015232357215E-15 ) ) ;
#7811 = CARTESIAN_POINT ( 'NONE',  ( -13.57481594606304576, 33.95546875216787441, 0.000000000000000000 ) ) ;
#7812 = CARTESIAN_POINT ( 'NONE',  ( 99.99999999999998579, 128.0000000000000000, -2.500000000000013767 ) ) ;
#7813 = CARTESIAN_POINT ( 'NONE',  ( 99.99999999999995737, 80.68750000136559208, 4.458734124999988779 ) ) ;
#7814 = CARTESIAN_POINT ( 'NONE',  ( 55.70494972787295751, 33.50898437608393010, 9.295050272127047819 ) ) ;
#7815 = CARTESIAN_POINT ( 'NONE',  ( 91.91746824999999887, 110.0000000000000000, -51.37500000273119127 ) ) ;
#7816 = CARTESIAN_POINT ( 'NONE',  ( 107.0000000000000000, 107.7255621263696668, -46.10000000000000142 ) ) ;
#7817 =( BOUNDED_CURVE ( )  B_SPLINE_CURVE ( 2, ( #12422, #12006, #21140, #25133, #10286, #10016, #18994, #18724, #20731 ),
 .UNSPECIFIED., .F., .F. ) 
 B_SPLINE_CURVE_WITH_KNOTS ( ( 3, 2, 2, 2, 3 ),
 ( 0.06250000000000004163, 0.07291666666666665741, 0.08333333333333325932, 0.09374999999999987510, 0.1041666666666664909 ),
 .UNSPECIFIED. ) 
 CURVE ( )  GEOMETRIC_REPRESENTATION_ITEM ( )  RATIONAL_B_SPLINE_CURVE ( ( 0.9999999999999996669, 0.9238795325112870716, 1.000000000000000000, 0.9238795325112867385, 1.000000000000000000, 0.9238795325112867385, 1.000000000000000000, 0.9238795325112880708, 0.9999999999999986677 ) ) 
 REPRESENTATION_ITEM ( '' )  );
#7818 = DIRECTION ( 'NONE',  ( 0.000000000000000000, 0.000000000000000000, -1.000000000000000000 ) ) ;
#7819 = CARTESIAN_POINT ( 'NONE',  ( 9.598844408820456309, 33.55859375000000000, -9.598844408820458085 ) ) ;
#7820 = CARTESIAN_POINT ( 'NONE',  ( 97.50236033167490746, 102.3130555110000159, -53.47499999726882436 ) ) ;
#7821 = CARTESIAN_POINT ( 'NONE',  ( 124.5550856135277087, 35.34453125108393579, 13.14518615778179722 ) ) ;
#7822 = VERTEX_POINT ( 'NONE', #26401 ) ;
#7823 = CARTESIAN_POINT ( 'NONE',  ( 74.59884440882045453, 38.22187500216787015, 9.598844408820456309 ) ) ;
#7824 = CARTESIAN_POINT ( 'NONE',  ( 95.54126587499996504, 82.43750000136559208, -1.387778780781445676E-14 ) ) ;
#7825 = CARTESIAN_POINT ( 'NONE',  ( 116.8548138422182063, 40.50390625108394005, -5.444914386472297529 ) ) ;
#7826 = CARTESIAN_POINT ( 'NONE',  ( 200.6228728715778686, 37.57695312499999574, -13.57481594606304753 ) ) ;
#7827 = CARTESIAN_POINT ( 'NONE',  ( 91.91746824999997045, 107.3738262389971538, -51.52499999726882152 ) ) ;
#7828 = CARTESIAN_POINT ( 'NONE',  ( -9.598844408820458085, 39.41250000216787441, -9.598844408820458085 ) ) ;
#7829 = ORIENTED_EDGE ( 'NONE', *, *, #19411, .T. ) ;
#7830 = CARTESIAN_POINT ( 'NONE',  ( 103.5355339059327093, 3.535533905932755072, 8.624999999999998224 ) ) ;
#7831 = VERTEX_POINT ( 'NONE', #22124 ) ;
#7832 = CARTESIAN_POINT ( 'NONE',  ( 9.295050272127047819, 33.11210937608393579, 9.295050272127046043 ) ) ;
#7833 = CARTESIAN_POINT ( 'NONE',  ( 208.1451861577818079, 39.36289062608393152, -1.609821015232357215E-15 ) ) ;
#7834 = DIRECTION ( 'NONE',  ( 0.000000000000000000, 0.000000000000000000, 1.000000000000000000 ) ) ;
#7835 = MANIFOLD_SOLID_BREP ( 'Cavity1', #18093 ) ;
#7836 = CARTESIAN_POINT ( 'NONE',  ( 94.99999999999995737, 2.071067811865491048, 14.06250000273118772 ) ) ;
#7837 = CARTESIAN_POINT ( 'NONE',  ( 143.1451861577818363, 37.03125000108393294, -5.444914386472297529 ) ) ;
#7838 = CARTESIAN_POINT ( 'NONE',  ( 5.444914386472297529, 33.36015625108393579, -13.14518615778179900 ) ) ;
#7839 = DIRECTION ( 'NONE',  ( -0.000000000000000000, 1.000000000000000000, -0.000000000000000000 ) ) ;
#7840 = DIRECTION ( 'NONE',  ( 0.000000000000000000, 0.000000000000000000, -1.000000000000000000 ) ) ;
#7841 = CARTESIAN_POINT ( 'NONE',  ( 98.53841926354351699, 123.2500000010924737, 1.461580736456455920 ) ) ;
#7842 = CARTESIAN_POINT ( 'NONE',  ( 185.4011555911795313, 40.10703124999999147, -9.598844408820458085 ) ) ;
#7843 = ITEM_DEFINED_TRANSFORMATION ( 'NONE', 'NONE', #9925,  #26844 ) ;
#7844 = DIRECTION ( 'NONE',  ( -5.782411586589357392E-17, 0.000000000000000000, -1.000000000000000000 ) ) ;
#7845 = CARTESIAN_POINT ( 'NONE',  ( 96.84719886470459471, -3.152801135295355994, 5.812500001365591196 ) ) ;
#7846 = CARTESIAN_POINT ( 'NONE',  ( 93.00000000000000000, 110.0000000000000000, -52.50000000546237544 ) ) ;
#7847 = CARTESIAN_POINT ( 'NONE',  ( 95.54126587499996504, -1.846868145590724986, 5.500000001365591196 ) ) ;
#7848 = CARTESIAN_POINT ( 'NONE',  ( 97.83688103937538472, 116.6573956140660897, -50.90000000546238113 ) ) ;
#7849 = CARTESIAN_POINT ( 'NONE',  ( 104.4587341249999923, 93.62499999863440792, -1.846868145590737198 ) ) ;
#7850 = CARTESIAN_POINT ( 'NONE',  ( 97.92893218813451028, -4.999999999999989342, 4.187499999999998224 ) ) ;
#7851 = CARTESIAN_POINT ( 'NONE',  ( 102.3556624333333076, 122.3833333351541199, -9.829464563757769835E-15 ) ) ;
#7852 = CARTESIAN_POINT ( 'NONE',  ( -8.049105076161786076E-16, 34.20351562608394147, -13.14518615778179544 ) ) ;
#7853 = VERTEX_POINT ( 'NONE', #9421 ) ;
#7854 = CARTESIAN_POINT ( 'NONE',  ( 96.84719886470459471, 83.81250000136560629, 3.152801135295355994 ) ) ;
#7855 = CARTESIAN_POINT ( 'NONE',  ( 99.99999999999998579, 90.56249999863440792, -4.458734124999994997 ) ) ;
#7856 =( BOUNDED_CURVE ( )  B_SPLINE_CURVE ( 2, ( #1123, #20206, #5106, #11776, #4970, #16058, #26776, #16205, #24909 ),
 .UNSPECIFIED., .F., .F. ) 
 B_SPLINE_CURVE_WITH_KNOTS ( ( 3, 2, 2, 2, 3 ),
 ( 0.7291666666666668517, 0.7395833333333334814, 0.7500000000000001110, 0.7604166666666667407, 0.7708333333333333703 ),
 .UNSPECIFIED. ) 
 CURVE ( )  GEOMETRIC_REPRESENTATION_ITEM ( )  RATIONAL_B_SPLINE_CURVE ( ( 0.9999999999999983347, 0.9238795325112884038, 1.000000000000000000, 0.9238795325112867385, 1.000000000000000000, 0.9238795325112867385, 1.000000000000000000, 0.9238795325112867385, 1.000000000000000000 ) ) 
 REPRESENTATION_ITEM ( '' )  );
#7857 = CARTESIAN_POINT ( 'NONE',  ( 185.7049497278729575, 33.50898437608393010, 9.295050272127047819 ) ) ;
#7858 = EDGE_LOOP ( 'NONE', ( #5451, #25002, #23974, #2656 ) ) ;
#7859 = DIRECTION ( 'NONE',  ( -0.000000000000000000, -0.000000000000000000, -1.000000000000000000 ) ) ;
#7860 = CARTESIAN_POINT ( 'NONE',  ( 96.84719886470459471, -3.152801135295355994, 7.812500001365592084 ) ) ;
#7861 = EDGE_CURVE ( 'NONE', #13418, #11663, #20698, .T. ) ;
#7862 = ORIENTED_EDGE ( 'NONE', *, *, #18231, .T. ) ;
#7863 = CARTESIAN_POINT ( 'NONE',  ( 97.50236033167492167, 102.3130555110000159, -48.97500000273119269 ) ) ;
#7864 = CARTESIAN_POINT ( 'NONE',  ( -5.444914386472299306, 32.76484375108393010, 13.14518615778179722 ) ) ;
#7865 = CARTESIAN_POINT ( 'NONE',  ( 219.9999999999999716, 80.00000000000000000, 9.999999999999946709 ) ) ;
#7866 = CARTESIAN_POINT ( 'NONE',  ( -9.295050272127046043, 38.86679687608393863, -9.295050272127046043 ) ) ;
#7867 = CARTESIAN_POINT ( 'NONE',  ( 9.295050272127047819, 37.87460937608393863, 9.295050272127046043 ) ) ;
#7868 = CARTESIAN_POINT ( 'NONE',  ( -9.295050272127044266, 33.50898437608393010, 9.295050272127047819 ) ) ;
#7869 = CARTESIAN_POINT ( 'NONE',  ( 104.4587341249999923, 93.62499999863440792, -1.846868145590737198 ) ) ;
#7870 = CARTESIAN_POINT ( 'NONE',  ( 99.99999999999995737, 80.37500000273119838, 4.999999999999990230 ) ) ;
#7871 = CONICAL_SURFACE ( 'NONE', #8330, 23.85284712729792389, 0.9599310885968833640 ) ;
#7872 = CARTESIAN_POINT ( 'NONE',  ( 92.99999999999998579, 110.0000000000000000, -51.00000000000000711 ) ) ;
#7873 = FACE_OUTER_BOUND ( 'NONE', #7316, .T. ) ;
#7874 = CARTESIAN_POINT ( 'NONE',  ( 95.54126587499996504, 1.387778780781445676E-14, 2.687500001365592528 ) ) ;
#7875 = CARTESIAN_POINT ( 'NONE',  ( 98.15313185440923860, 82.87500000136560629, 4.458734124999987891 ) ) ;
#7876 = CARTESIAN_POINT ( 'NONE',  ( 5.444914386472297529, 35.54296875108393294, -13.14518615778179900 ) ) ;
#7877 = CARTESIAN_POINT ( 'NONE',  ( 78.57481594606305464, 39.06523437716786873, 5.622872871577868636 ) ) ;
#7878 = CARTESIAN_POINT ( 'NONE',  ( 2.493653234604083739E-15, 38.91640625216786731, 13.57481594606304576 ) ) ;
#7879 = ORIENTED_EDGE ( 'NONE', *, *, #17356, .T. ) ;
#7880 = CARTESIAN_POINT ( 'NONE',  ( -8.049105076161786076E-16, 31.82226562608393650, -13.14518615778179544 ) ) ;
#7881 = CARTESIAN_POINT ( 'NONE',  ( 97.93301270000000613, 123.7500000010924879, -9.540979117872439019E-15 ) ) ;
#7882 = CARTESIAN_POINT ( 'NONE',  ( 96.84719886470463734, 94.93749999863440792, -3.152801135295366208 ) ) ;
#7883 = DIRECTION ( 'NONE',  ( -0.000000000000000000, 1.000000000000000000, -0.000000000000000000 ) ) ;
#7884 = CARTESIAN_POINT ( 'NONE',  ( 95.00472066334982912, 103.1245878333314323, -55.57499999726881157 ) ) ;
#7885 = CARTESIAN_POINT ( 'NONE',  ( 94.99999999999995737, 1.387778780781445676E-14, 6.125000002731185056 ) ) ;
#7886 = CARTESIAN_POINT ( 'NONE',  ( 5.444914386472297529, 32.36796875108393579, -13.14518615778179900 ) ) ;
#7887 = ORIENTED_EDGE ( 'NONE', *, *, #13135, .F. ) ;
#7888 = CARTESIAN_POINT ( 'NONE',  ( 55.70494972787295751, 38.46992187608393721, 9.295050272127047819 ) ) ;
#7889 = VERTEX_POINT ( 'NONE', #2875 ) ;
#7890 = CARTESIAN_POINT ( 'NONE',  ( 13.57481594606304931, 32.71523437716787441, 5.622872871577868636 ) ) ;
#7891 =( GEOMETRIC_REPRESENTATION_CONTEXT ( 3 ) GLOBAL_UNCERTAINTY_ASSIGNED_CONTEXT ( ( #17530 ) ) GLOBAL_UNIT_ASSIGNED_CONTEXT ( ( #13440, #26151, #22598 ) ) REPRESENTATION_CONTEXT ( 'NONE', 'WORKASPACE' ) );
#7892 = CARTESIAN_POINT ( 'NONE',  ( -8.312177448680279460E-16, 35.24531249999999716, -13.57481594606304576 ) ) ;
#7893 = ORIENTED_EDGE ( 'NONE', *, *, #8047, .F. ) ;
#7894 = CARTESIAN_POINT ( 'NONE',  ( 65.00000000000000000, 37.62656249999999858, -13.57481594606304576 ) ) ;
#7895 = DIRECTION ( 'NONE',  ( 0.000000000000000000, 0.000000000000000000, 1.000000000000000000 ) ) ;
#7896 = CARTESIAN_POINT ( 'NONE',  ( 143.5748159460630688, 36.68398437716787441, 5.622872871577868636 ) ) ;
#7897 = CARTESIAN_POINT ( 'NONE',  ( 143.5748159460630404, 35.98945312716787015, -5.622872871577873077 ) ) ;
#7898 = ADVANCED_FACE ( 'NONE', ( #22268 ), #9282, .T. ) ;
#7899 = CARTESIAN_POINT ( 'NONE',  ( 93.00000000000000000, 110.0000000000000000, -44.50000000546237544 ) ) ;
#7900 = LINE ( 'NONE', #21154, #4159 ) ;
#7901 = CARTESIAN_POINT ( 'NONE',  ( 181.8548138422181921, 36.73359375108393010, -5.444914386472297529 ) ) ;
#7902 = ORIENTED_EDGE ( 'NONE', *, *, #20337, .F. ) ;
#7903 = ORIENTED_EDGE ( 'NONE', *, *, #15621, .F. ) ;
#7904 = CARTESIAN_POINT ( 'NONE',  ( 98.15313185440925281, -4.458734124999987891, 2.625000001365592084 ) ) ;
#7905 = CARTESIAN_POINT ( 'NONE',  ( 104.4587341249999781, 1.846868145590750521, 14.25000000136559208 ) ) ;
#7906 = CARTESIAN_POINT ( 'NONE',  ( -8.312177448680279460E-16, 38.42031249999999432, -13.57481594606304576 ) ) ;
#7907 = DIRECTION ( 'NONE',  ( 0.000000000000000000, 0.000000000000000000, 1.000000000000000000 ) ) ;
#7908 = LINE ( 'NONE', #1645, #14851 ) ;
#7909 = CIRCLE ( 'NONE', #18338, 5.000000000000004441 ) ;
#7910 = DIRECTION ( 'NONE',  ( 0.000000000000000000, 0.000000000000000000, 1.000000000000000000 ) ) ;
#7911 = CARTESIAN_POINT ( 'NONE',  ( -5.444914386472297529, 40.60312500108393863, -13.14518615778179900 ) ) ;
#7912 = CARTESIAN_POINT ( 'NONE',  ( 13.39333672780522733, 35.99999999999999289, -2.034633736483404398 ) ) ;
#7913 = CARTESIAN_POINT ( 'NONE',  ( 103.5355339059327235, 93.74999999726881583, 3.535533905932724874 ) ) ;
#7914 = CARTESIAN_POINT ( 'NONE',  ( 104.9952793366501709, 116.8754121666685393, -46.32499999726881867 ) ) ;
#7915 = ORIENTED_EDGE ( 'NONE', *, *, #8104, .T. ) ;
#7916 = ORIENTED_EDGE ( 'NONE', *, *, #22040, .F. ) ;
#7917 = CARTESIAN_POINT ( 'NONE',  ( 2.493653234604083739E-15, 37.32890625216786873, 13.57481594606304576 ) ) ;
#7918 = CARTESIAN_POINT ( 'NONE',  ( -9.295050272127046043, 31.92148437608393508, -9.295050272127046043 ) ) ;
#7919 = CARTESIAN_POINT ( 'NONE',  ( 7.171391395016640580, 31.30502190640808990, -11.52591746582321974 ) ) ;
#7920 = CARTESIAN_POINT ( 'NONE',  ( 104.9999999999999574, 2.071067811865491937, 5.687500002731185056 ) ) ;
#7921 = CARTESIAN_POINT ( 'NONE',  ( 120.7049497278729575, 40.65273437608393436, -9.295050272127046043 ) ) ;
#7922 = CARTESIAN_POINT ( 'NONE',  ( 59.55508561352770158, 35.93984375108392726, 13.14518615778179722 ) ) ;
#7923 = DIRECTION ( 'NONE',  ( -0.000000000000000000, -0.000000000000000000, -1.000000000000000000 ) ) ;
#7924 = CARTESIAN_POINT ( 'NONE',  ( -5.444914386472297529, 35.64218750108392442, -13.14518615778179900 ) ) ;
#7925 = ADVANCED_FACE ( 'NONE', ( #27119 ), #1811, .F. ) ;
#7926 = CARTESIAN_POINT ( 'NONE',  ( 98.23223304703363112, 124.2000000021849502, -1.767766952966370209 ) ) ;
#7927 = DIRECTION ( 'NONE',  ( 0.000000000000000000, 0.000000000000000000, -1.000000000000000000 ) ) ;
#7928 = DIRECTION ( 'NONE',  ( 0.000000000000000000, -1.000000000000000000, 0.000000000000000000 ) ) ;
#7929 = CARTESIAN_POINT ( 'NONE',  ( 204.5988444088204687, 40.50390624999999289, 9.598844408820456309 ) ) ;
#7930 = CARTESIAN_POINT ( 'NONE',  ( 5.444914386472302859, 37.62656250108393863, 13.14518615778179189 ) ) ;
#7931 = CARTESIAN_POINT ( 'NONE',  ( 143.2454503467689619, 36.00000000000000000, 2.307131236160140375 ) ) ;
#7932 = CARTESIAN_POINT ( 'NONE',  ( 102.4999999999999716, 124.5500000000000114, 1.035533905932722876 ) ) ;
#7933 = ADVANCED_FACE ( 'NONE', ( #5448 ), #22298, .T. ) ;
#7934 = CARTESIAN_POINT ( 'NONE',  ( 97.93301269999999192, 123.1000000010924822, -0.8561741729129505041 ) ) ;
#7935 = CARTESIAN_POINT ( 'NONE',  ( 102.1631189606246153, 116.6573956140660897, -51.09999999453764019 ) ) ;
#7936 = VECTOR ( 'NONE', #24823, 1000.000000000000000 ) ;
#7937 = DIRECTION ( 'NONE',  ( -1.000000000000000000, 0.000000000000000000, 0.000000000000000000 ) ) ;
#7938 = CARTESIAN_POINT ( 'NONE',  ( 95.54126587499995082, -1.846868145590724986, 13.50000000136559208 ) ) ;
#7939 = DIRECTION ( 'NONE',  ( 0.000000000000000000, 1.000000000000000000, 0.000000000000000000 ) ) ;
#7940 = ORIENTED_EDGE ( 'NONE', *, *, #14668, .T. ) ;
#7941 = CARTESIAN_POINT ( 'NONE',  ( 0.000000000000000000, 30.99999999999999645, -13.57481594606304576 ) ) ;
#7942 = CARTESIAN_POINT ( 'NONE',  ( -13.57481594606304576, 40.99999999999999289, 0.000000000000000000 ) ) ;
#7943 = LINE ( 'NONE', #21341, #5038 ) ;
#7944 = EDGE_CURVE ( 'NONE', #16904, #10007, #11250, .T. ) ;
#7945 = CARTESIAN_POINT ( 'NONE',  ( -9.598844408820458085, 31.47500000216787441, -9.598844408820458085 ) ) ;
#7946 = CARTESIAN_POINT ( 'NONE',  ( 101.8468681455906903, 81.75000000136560629, 4.458734124999987891 ) ) ;
#7947 = CARTESIAN_POINT ( 'NONE',  ( 51.85481384221820633, 39.21406250108392300, 5.444914386472304635 ) ) ;
#7948 = CARTESIAN_POINT ( 'NONE',  ( 108.0825317500000153, 110.0000000000000000, -48.37500000273119838 ) ) ;
#7949 = DIRECTION ( 'NONE',  ( -0.000000000000000000, 1.000000000000000000, -0.000000000000000000 ) ) ;
#7950 = CARTESIAN_POINT ( 'NONE',  ( 97.93301269999999192, 123.1000000010924822, -0.8561741729129505041 ) ) ;
#7951 = CARTESIAN_POINT ( 'NONE',  ( 97.83688103937537051, 103.3426043859339103, -50.09999999453764019 ) ) ;
#7952 = CARTESIAN_POINT ( 'NONE',  ( 143.1451861577818079, 34.05468750108394005, -5.444914386472297529 ) ) ;
#7953 = VERTEX_POINT ( 'NONE', #22406 ) ;
#7954 = CARTESIAN_POINT ( 'NONE',  ( -7.616525325480801634, 54.91574374957786375, -14.99999999999999822 ) ) ;
#7955 = DIRECTION ( 'NONE',  ( 0.000000000000000000, -0.000000000000000000, -1.000000000000000000 ) ) ;
#7956 = CARTESIAN_POINT ( 'NONE',  ( 13.57481594606304753, 39.16445312716788152, -5.622872871577873077 ) ) ;
#7957 = CARTESIAN_POINT ( 'NONE',  ( 120.7049497278729575, 38.27148437608393294, 9.295050272127047819 ) ) ;
#7958 = CARTESIAN_POINT ( 'NONE',  ( 65.00000000000000000, 36.53515625216787299, 13.57481594606304576 ) ) ;
#7959 = VECTOR ( 'NONE', #3521, 1000.000000000000000 ) ;
#7960 = CARTESIAN_POINT ( 'NONE',  ( 95.00472066334982912, 103.1245878333314323, -51.32499999726880446 ) ) ;
#7961 = CARTESIAN_POINT ( 'NONE',  ( -5.622872871577873077, 38.07304687716787583, 13.57481594606304753 ) ) ;
#7962 = ORIENTED_EDGE ( 'NONE', *, *, #4299, .T. ) ;
#7963 = CARTESIAN_POINT ( 'NONE',  ( 102.0710678118654329, -4.999999999999989342, 7.312500000000000000 ) ) ;
#7964 = ORIENTED_EDGE ( 'NONE', *, *, #13839, .T. ) ;
#7965 = CARTESIAN_POINT ( 'NONE',  ( -13.14518615778179189, 32.86406250108393579, 5.444914386472304635 ) ) ;
#7966 = CARTESIAN_POINT ( 'NONE',  ( 189.3771271284221314, 31.72304687716787441, 13.57481594606304753 ) ) ;
#7967 = CARTESIAN_POINT ( 'NONE',  ( 99.99999999999995737, 81.75000000000000000, -5.000000000000018652 ) ) ;
#7968 = EDGE_CURVE ( 'NONE', #1889, #13215, #22695, .T. ) ;
#7969 = CARTESIAN_POINT ( 'NONE',  ( 116.8548138422182205, 37.37851562608393863, 0.000000000000000000 ) ) ;
#7970 = CARTESIAN_POINT ( 'NONE',  ( 13.14518615778179900, 33.26093750108393721, -5.444914386472297529 ) ) ;
#7971 = DIRECTION ( 'NONE',  ( 0.000000000000000000, -0.000000000000000000, 1.000000000000000000 ) ) ;
#7972 = CARTESIAN_POINT ( 'NONE',  ( 101.8468681455907330, 94.12499999863439371, 4.458734124999980786 ) ) ;
#7973 =( BOUNDED_CURVE ( )  B_SPLINE_CURVE ( 2, ( #4731, #457, #9417, #13391, #26684, #3160, #11541, #9001, #22119 ),
 .UNSPECIFIED., .F., .F. ) 
 B_SPLINE_CURVE_WITH_KNOTS ( ( 3, 2, 2, 2, 3 ),
 ( 0.05000000000000004441, 0.07500000000000006661, 0.1000000000000000888, 0.1250000000000001110, 0.1500000000000001332 ),
 .UNSPECIFIED. ) 
 CURVE ( )  GEOMETRIC_REPRESENTATION_ITEM ( )  RATIONAL_B_SPLINE_CURVE ( ( 0.9999999999999998890, 0.9238795325112868495, 1.000000000000000000, 0.9238795325112867385, 1.000000000000000000, 0.9238795325112867385, 1.000000000000000000, 0.9238795325112862944, 1.000000000000000444 ) ) 
 REPRESENTATION_ITEM ( '' )  );
#7974 = CARTESIAN_POINT ( 'NONE',  ( 97.50000000000000000, 123.3499999999999943, -1.035533905932742416 ) ) ;
#7975 = CARTESIAN_POINT ( 'NONE',  ( 200.6228728715778686, 37.27929687499999289, 13.57481594606304576 ) ) ;
#7976 = CARTESIAN_POINT ( 'NONE',  ( 55.40115559117954547, 39.51171874999999289, 9.598844408820459861 ) ) ;
#7977 = CARTESIAN_POINT ( 'NONE',  ( 101.8468681455906903, -4.458734124999987891, 5.000000001365592972 ) ) ;
#7978 = CARTESIAN_POINT ( 'NONE',  ( 70.44491438647230552, 39.21406250108392300, 13.14518615778179189 ) ) ;
#7979 = VECTOR ( 'NONE', #21231, 1000.000000000000000 ) ;
#7980 = CARTESIAN_POINT ( 'NONE',  ( 104.4587341249999639, 1.442382525525748735E-14, 4.937500001365592972 ) ) ;
#7981 = CARTESIAN_POINT ( 'NONE',  ( 105.6631189606246295, 114.1144967660473242, -47.30000000546237260 ) ) ;
#7982 = CARTESIAN_POINT ( 'NONE',  ( 98.15313185440925281, 93.24999999863439371, 4.458734124999979898 ) ) ;
#7983 = CARTESIAN_POINT ( 'NONE',  ( 104.9999999999999716, -2.071067811865462627, 9.437500000000000000 ) ) ;
#7984 = CARTESIAN_POINT ( 'NONE',  ( 130.0000000000000000, 52.00000000000000711, 11.57481594606302799 ) ) ;
#7985 = CARTESIAN_POINT ( 'NONE',  ( -9.598844408820454532, 40.30546874999999574, 9.598844408820459861 ) ) ;
#7986 = ORIENTED_EDGE ( 'NONE', *, *, #11387, .T. ) ;
#7987 = CARTESIAN_POINT ( 'NONE',  ( 103.1528011352953342, 81.31250000136559208, -3.152801135295383084 ) ) ;
#7988 = VECTOR ( 'NONE', #2194, 1000.000000000000000 ) ;
#7989 = CIRCLE ( 'NONE', #23916, 13.57481594606304398 ) ;
#7990 = CARTESIAN_POINT ( 'NONE',  ( 104.4587341249999781, 91.31249999863440792, -6.938893903907228378E-15 ) ) ;
#7991 = VERTEX_POINT ( 'NONE', #26688 ) ;
#7992 = ORIENTED_EDGE ( 'NONE', *, *, #3475, .F. ) ;
#7993 = CARTESIAN_POINT ( 'NONE',  ( 186.2306103279209140, 50.37710889402406877, -14.99999999999737454 ) ) ;
#7994 = CARTESIAN_POINT ( 'NONE',  ( 99.99999999999995737, -4.458734124999988779, 5.937500001365592084 ) ) ;
#7995 = ORIENTED_EDGE ( 'NONE', *, *, #7861, .F. ) ;
#7996 = CARTESIAN_POINT ( 'NONE',  ( 99.99999999999998579, 118.4984768113314004, -47.87500000273119127 ) ) ;
#7997 = CARTESIAN_POINT ( 'NONE',  ( 9.295050272127047819, 32.91367187608393152, 9.295050272127046043 ) ) ;
#7998 = CARTESIAN_POINT ( 'NONE',  ( 195.0000000000000000, 40.10703125216787157, -13.57481594606304576 ) ) ;
#7999 = CARTESIAN_POINT ( 'NONE',  ( -9.295050272127044266, 38.27148437608393294, 9.295050272127047819 ) ) ;
#8000 = CARTESIAN_POINT ( 'NONE',  ( 91.91746824999999887, 110.0000000000000000, -47.12500000273119838 ) ) ;
#8001 = CARTESIAN_POINT ( 'NONE',  ( 130.0000000000000000, 40.15664062608393436, 13.14518615778179544 ) ) ;
#8002 = CARTESIAN_POINT ( 'NONE',  ( -5.444914386472299306, 32.76484375108393010, 13.14518615778179722 ) ) ;
#8003 = ORIENTED_EDGE ( 'NONE', *, *, #4147, .T. ) ;
#8004 = CARTESIAN_POINT ( 'NONE',  ( 55.40115559117954547, 38.71796874999999716, 9.598844408820459861 ) ) ;
#8005 = CIRCLE ( 'NONE', #11630, 5.000000000000004441 ) ;
#8006 = CARTESIAN_POINT ( 'NONE',  ( 102.4999999999999858, 123.0500000000000114, -1.035533905932742638 ) ) ;
#8007 = CARTESIAN_POINT ( 'NONE',  ( 1.662435489736055498E-15, 50.00000000000000000, -13.57481594606304398 ) ) ;
#8008 = CARTESIAN_POINT ( 'NONE',  ( 95.54126587499996504, 1.387778780781445676E-14, 5.437500001365591196 ) ) ;
#8009 = CARTESIAN_POINT ( 'NONE',  ( 94.99999999999995737, 1.387778780781445676E-14, 4.125000002731185056 ) ) ;
#8010 = CARTESIAN_POINT ( 'NONE',  ( 104.4587341249999781, 1.846868145590750521, 1.250000001365592750 ) ) ;
#8011 = CARTESIAN_POINT ( 'NONE',  ( 95.54126587499996504, 83.68750000136560629, -1.387778780781445676E-14 ) ) ;
#8012 = CARTESIAN_POINT ( 'NONE',  ( 5.444914386472302859, 32.86406250108392868, 13.14518615778179189 ) ) ;
#8013 = CARTESIAN_POINT ( 'NONE',  ( 104.9999999999999716, 1.449011120738813565E-14, 8.625000002731185944 ) ) ;
#8014 = CARTESIAN_POINT ( 'NONE',  ( 84.99999999999998579, 100.0000000000000000, -15.00000000000000533 ) ) ;
#8015 = VERTEX_POINT ( 'NONE', #18120 ) ;
#8016 = CARTESIAN_POINT ( 'NONE',  ( 9.295050272127047819, 32.31835937608393294, 9.295050272127046043 ) ) ;
#8017 = ADVANCED_FACE ( 'NONE', ( #7281 ), #604, .F. ) ;
#8018 =( BOUNDED_CURVE ( )  B_SPLINE_CURVE ( 2, ( #5073, #7331, #9195, #20034, #3211, #2924, #11879, #15741, #20603 ),
 .UNSPECIFIED., .F., .F. ) 
 B_SPLINE_CURVE_WITH_KNOTS ( ( 3, 2, 2, 2, 3 ),
 ( 0.5624999999999996669, 0.5729166666666664076, 0.5833333333333332593, 0.5937500000000001110, 0.6041666666666668517 ),
 .UNSPECIFIED. ) 
 CURVE ( )  GEOMETRIC_REPRESENTATION_ITEM ( )  RATIONAL_B_SPLINE_CURVE ( ( 1.000000000000002442, 0.9238795325112842960, 1.000000000000000000, 0.9238795325112867385, 1.000000000000000000, 0.9238795325112867385, 1.000000000000000000, 0.9238795325112850731, 1.000000000000001554 ) ) 
 REPRESENTATION_ITEM ( '' )  );
#8019 = VECTOR ( 'NONE', #27074, 1000.000000000000000 ) ;
#8020 = CARTESIAN_POINT ( 'NONE',  ( -20.00000000000000000, 55.00000000000000000, 10.00000000000000178 ) ) ;
#8021 = FACE_OUTER_BOUND ( 'NONE', #18999, .T. ) ;
#8022 = DIRECTION ( 'NONE',  ( 0.000000000000000000, 0.000000000000000000, 1.000000000000000000 ) ) ;
#8023 = CARTESIAN_POINT ( 'NONE',  ( 102.4468180503172476, 122.9999999999999574, -0.3717709916353664212 ) ) ;
#8024 = CARTESIAN_POINT ( 'NONE',  ( 1.662435489736055498E-15, -7.395377635281828788, -13.57481594606304398 ) ) ;
#8025 = CIRCLE ( 'NONE', #18029, 13.57481594606304398 ) ;
#8026 = EDGE_LOOP ( 'NONE', ( #8473, #9672, #28118, #18030, #22102, #4773, #20596, #7829, #5498, #14119, #26582, #5703, #15944, #10862, #26519, #2142, #15256 ) ) ;
#8027 = CARTESIAN_POINT ( 'NONE',  ( 59.55508561352770158, 37.42812500108394147, -13.14518615778179722 ) ) ;
#8028 = DIRECTION ( 'NONE',  ( -0.000000000000000000, 1.000000000000000000, -0.000000000000000000 ) ) ;
#8029 = CYLINDRICAL_SURFACE ( 'NONE', #11657, 5.000000000000004441 ) ;
#8030 = ORIENTED_EDGE ( 'NONE', *, *, #16988, .F. ) ;
#8031 = CARTESIAN_POINT ( 'NONE',  ( 94.33688103937537051, 114.1144967660473242, -54.20000000000000284 ) ) ;
#8032 = CARTESIAN_POINT ( 'NONE',  ( -3.803054373244904696, 54.09082899096177499, -15.00000000000000000 ) ) ;
#8033 = CARTESIAN_POINT ( 'NONE',  ( 196.5010191243050315, 53.60014735326985402, 14.99999999999994493 ) ) ;
#8034 = CARTESIAN_POINT ( 'NONE',  ( 143.5748159460630688, 33.55859375216787299, -1.662435489736055892E-15 ) ) ;
#8035 = AXIS2_PLACEMENT_3D ( 'NONE', #26816, #13951, #7404 ) ;
#8036 = CARTESIAN_POINT ( 'NONE',  ( 84.99999999999998579, 120.0000000000000000, -15.00000000000000533 ) ) ;
#8037 = DIRECTION ( 'NONE',  ( -1.000000000000000000, -6.938893903907235280E-16, 2.385244779468109755E-16 ) ) ;
#8038 = CARTESIAN_POINT ( 'NONE',  ( 195.0000000000000000, 37.77539062608393294, 13.14518615778179544 ) ) ;
#8039 = ORIENTED_EDGE ( 'NONE', *, *, #15218, .F. ) ;
#8040 = ORIENTED_EDGE ( 'NONE', *, *, #17718, .F. ) ;
#8041 = CIRCLE ( 'NONE', #20348, 25.00000000000000711 ) ;
#8042 = CARTESIAN_POINT ( 'NONE',  ( 103.1528011352953342, 3.152801135295383084, 13.31250000136559386 ) ) ;
#8043 = CARTESIAN_POINT ( 'NONE',  ( 5.622872871577786924, 33.40976562716787157, 13.57481594606313813 ) ) ;
#8044 = FACE_BOUND ( 'NONE', #13380, .T. ) ;
#8045 = CARTESIAN_POINT ( 'NONE',  ( 214.9999999999999716, 80.00000000000000000, 14.99999999999994493 ) ) ;
#8046 = CARTESIAN_POINT ( 'NONE',  ( 9.295050272127046043, 39.66054687608393436, -9.295050272127046043 ) ) ;
#8047 = EDGE_CURVE ( 'NONE', #12248, #8859, #9084, .T. ) ;
#8048 = CARTESIAN_POINT ( 'NONE',  ( 139.1801758136479918, 50.00000000000000000, -10.00000000000000000 ) ) ;
#8049 = CARTESIAN_POINT ( 'NONE',  ( 93.00000000000002842, 112.2744378736303759, -48.60000000546236976 ) ) ;
#8050 = DIRECTION ( 'NONE',  ( 0.000000000000000000, -1.000000000000000000, 0.000000000000000000 ) ) ;
#8051 = CARTESIAN_POINT ( 'NONE',  ( 97.50236033167490746, 102.3130555110000159, -49.22499999726882436 ) ) ;
#8052 = ORIENTED_EDGE ( 'NONE', *, *, #17839, .T. ) ;
#8053 = UNCERTAINTY_MEASURE_WITH_UNIT (LENGTH_MEASURE( 1.000000000000000082E-05 ), #16875, 'distance_accuracy_value', 'NONE');
#8054 = CARTESIAN_POINT ( 'NONE',  ( -9.598844408820458085, 40.90078124999999432, -9.598844408820458085 ) ) ;
#8055 = CARTESIAN_POINT ( 'NONE',  ( 9.295050272127047819, 39.26367187608393294, 9.295050272127046043 ) ) ;
#8056 = VECTOR ( 'NONE', #4061, 1000.000000000000000 ) ;
#8057 = CARTESIAN_POINT ( 'NONE',  ( 103.5355339059327093, 3.535533905932755072, 5.750000002731185056 ) ) ;
#8058 = CARTESIAN_POINT ( 'NONE',  ( 143.1451861577818079, 38.02343750108395426, -5.444914386472297529 ) ) ;
#8059 = CARTESIAN_POINT ( 'NONE',  ( 74.29505027212704249, 35.49335937608393010, -9.295050272127046043 ) ) ;
#8060 = DIRECTION ( 'NONE',  ( 0.000000000000000000, 1.000000000000000000, 0.000000000000000000 ) ) ;
#8061 = CARTESIAN_POINT ( 'NONE',  ( -9.295050272127044266, 35.89023437608393152, 9.295050272127047819 ) ) ;
#8062 = CARTESIAN_POINT ( 'NONE',  ( 190.0271122604904406, 36.00000000000000711, -12.48139679469847607 ) ) ;
#8063 = DIRECTION ( 'NONE',  ( -0.000000000000000000, -1.000000000000000000, -0.000000000000000000 ) ) ;
#8064 = CARTESIAN_POINT ( 'NONE',  ( 102.1631189606246295, 116.6573956140660897, -48.60000000000000142 ) ) ;
#8065 = DIRECTION ( 'NONE',  ( -1.000000000000000000, 0.000000000000000000, 0.000000000000000000 ) ) ;
#8066 = DIRECTION ( 'NONE',  ( 0.000000000000000000, 0.000000000000000000, -1.000000000000000000 ) ) ;
#8067 = CARTESIAN_POINT ( 'NONE',  ( -13.14518615778179544, 37.37851562608393863, 0.000000000000000000 ) ) ;
#8068 = CARTESIAN_POINT ( 'NONE',  ( 133.3041185978226224, 35.99999999999998579, 12.77244747738241770 ) ) ;
#8069 = CARTESIAN_POINT ( 'NONE',  ( 97.50000000000000000, 124.1499999999999915, -1.035533905932742416 ) ) ;
#8070 = CARTESIAN_POINT ( 'NONE',  ( 97.93301270000000613, 124.7500000010924737, -9.540979117872439019E-15 ) ) ;
#8071 = CARTESIAN_POINT ( 'NONE',  ( 97.93301270000000613, 123.9000000010924794, -0.8561741729129506151 ) ) ;
#8072 = EDGE_CURVE ( 'NONE', #3824, #18580, #14115, .T. ) ;
#8073 = CYLINDRICAL_SURFACE ( 'NONE', #10873, 5.000000000000004441 ) ;
#8074 = CARTESIAN_POINT ( 'NONE',  ( 104.4587341249999781, 1.846868145590750299, 14.00000000136559208 ) ) ;
#8075 = CARTESIAN_POINT ( 'NONE',  ( -9.598844408820458085, 32.16953124999999147, -9.598844408820458085 ) ) ;
#8076 = ORIENTED_EDGE ( 'NONE', *, *, #26053, .T. ) ;
#8077 = CARTESIAN_POINT ( 'NONE',  ( 101.7677669529663547, 123.8000000021849587, 1.767766952966350891 ) ) ;
#8078 = AXIS2_PLACEMENT_3D ( 'NONE', #8488, #21184, #5940 ) ;
#8079 = CARTESIAN_POINT ( 'NONE',  ( 5.622872871577871301, 39.16445312499999432, -13.57481594606304753 ) ) ;
#8080 = CARTESIAN_POINT ( 'NONE',  ( 99.99999999999995737, 5.000000000000018652, 8.749999999999998224 ) ) ;
#8081 = CARTESIAN_POINT ( 'NONE',  ( 5.622872871577871301, 33.70742187716787441, -13.57481594606304753 ) ) ;
#8082 = CARTESIAN_POINT ( 'NONE',  ( 94.99999999999995737, 80.06250000000001421, 2.071067811865466624 ) ) ;
#8083 = CARTESIAN_POINT ( 'NONE',  ( 96.84719886470459471, 80.56250000136559208, 3.152801135295355994 ) ) ;
#8084 = CARTESIAN_POINT ( 'NONE',  ( 65.00000000000000000, 36.98164062608393721, 13.14518615778179544 ) ) ;
#8085 = CARTESIAN_POINT ( 'NONE',  ( 99.99999999999998579, 101.5015231886685854, -46.87500000273119838 ) ) ;
#8086 = LINE ( 'NONE', #5263, #22319 ) ;
#8087 = EDGE_CURVE ( 'NONE', #6724, #5473, #9993, .T. ) ;
#8088 = CARTESIAN_POINT ( 'NONE',  ( 99.14382582708707048, 124.6000000010924822, -2.066987299999999195 ) ) ;
#8089 = CARTESIAN_POINT ( 'NONE',  ( 102.4349316916707551, 122.9999999999999289, 0.6543697108981973987 ) ) ;
#8090 = CARTESIAN_POINT ( 'NONE',  ( 102.1631189606246153, 116.6573956140660897, -53.09999999453764019 ) ) ;
#8091 = CARTESIAN_POINT ( 'NONE',  ( 135.4449143864723055, 32.26875000108393721, 13.14518615778179189 ) ) ;
#8092 = VERTEX_POINT ( 'NONE', #25239 ) ;
#8093 = CARTESIAN_POINT ( 'NONE',  ( 94.33688103937535629, 105.8855032339526758, -52.29999999453764303 ) ) ;
#8094 = ADVANCED_FACE ( 'NONE', ( #5729 ), #25831, .T. ) ;
#8095 = CARTESIAN_POINT ( 'NONE',  ( -5.444914386472297529, 39.01562500108394005, -13.14518615778179900 ) ) ;
#8096 = CARTESIAN_POINT ( 'NONE',  ( 5.622872871577871301, 40.05742187716786873, -13.57481594606304753 ) ) ;
#8097 = CARTESIAN_POINT ( 'NONE',  ( 130.0000000000000000, 38.37070312608393152, 13.14518615778179544 ) ) ;
#8098 = CARTESIAN_POINT ( 'NONE',  ( 65.00000000000000000, 36.93203125216787441, -13.57481594606304576 ) ) ;
#8099 = EDGE_CURVE ( 'NONE', #28027, #947, #7244, .T. ) ;
#8100 = CARTESIAN_POINT ( 'NONE',  ( 106.5389055433250860, 114.7507929638356785, -54.42499999726882720 ) ) ;
#8101 = CARTESIAN_POINT ( 'NONE',  ( -13.57481594606304576, 35.54296875216788010, 0.000000000000000000 ) ) ;
#8102 = ORIENTED_EDGE ( 'NONE', *, *, #16815, .F. ) ;
#8103 = CARTESIAN_POINT ( 'NONE',  ( 102.0710678118654329, -4.999999999999989342, 10.31249999999999822 ) ) ;
#8104 = EDGE_CURVE ( 'NONE', #23060, #19811, #15659, .T. ) ;
#8105 = CARTESIAN_POINT ( 'NONE',  ( 107.0000000000000142, 112.2744378736303048, -47.40000000546237402 ) ) ;
#8106 = CARTESIAN_POINT ( 'NONE',  ( -8.049105076161786076E-16, 31.82226562608393650, -13.14518615778179544 ) ) ;
#8107 = CARTESIAN_POINT ( 'NONE',  ( 185.7049497278729575, 38.86679687608393863, -9.295050272127046043 ) ) ;
#8108 = CARTESIAN_POINT ( 'NONE',  ( 2.493653234604083739E-15, 34.94765625216787441, 13.57481594606304576 ) ) ;
#8109 = CARTESIAN_POINT ( 'NONE',  ( 135.4449143864723339, 38.42031250108393436, 13.14518615778179189 ) ) ;
#8110 = CARTESIAN_POINT ( 'NONE',  ( 13.14518615778179900, 33.16171875108393863, 5.444914386472293977 ) ) ;
#8111 = CARTESIAN_POINT ( 'NONE',  ( 130.0000000000000000, 37.22968749999999716, 13.57481594606304576 ) ) ;
#8112 = CARTESIAN_POINT ( 'NONE',  ( 104.4587341249999923, 93.24999999863439371, 1.846868145590726318 ) ) ;
#8113 = CARTESIAN_POINT ( 'NONE',  ( 97.92893218813451028, -4.999999999999989342, 12.31250000273118950 ) ) ;
#8114 = CARTESIAN_POINT ( 'NONE',  ( 13.14518615778179900, 39.41250000108393436, -5.444914386472297529 ) ) ;
#8115 = CARTESIAN_POINT ( 'NONE',  ( 185.4011555911795313, 38.51953124999999289, -9.598844408820458085 ) ) ;
#8116 = EDGE_CURVE ( 'NONE', #2928, #12585, #20230, .T. ) ;
#8117 = ITEM_DEFINED_TRANSFORMATION ( 'NONE', 'NONE', #870,  #26844 ) ;
#8118 = CARTESIAN_POINT ( 'NONE',  ( 0.000000000000000000, 40.99999999999999289, -13.57481594606304576 ) ) ;
#8119 = CARTESIAN_POINT ( 'NONE',  ( 103.1528011352953342, -3.152801135295355106, 3.062500001365592528 ) ) ;
#8120 = CARTESIAN_POINT ( 'NONE',  ( 74.29505027212704249, 40.25585937608393294, -9.295050272127046043 ) ) ;
#8121 = CARTESIAN_POINT ( 'NONE',  ( 104.4587341249999781, -1.846868145590721655, 7.875000001365592084 ) ) ;
#8122 = CARTESIAN_POINT ( 'NONE',  ( 95.67376207875072680, 115.9545556584642867, -50.80000000546237260 ) ) ;
#8123 = CARTESIAN_POINT ( 'NONE',  ( 103.1528011352953484, 90.43749999863440792, -3.152801135295366208 ) ) ;
#8124 = CARTESIAN_POINT ( 'NONE',  ( -1.021803718759008106, 36.00000000000000000, 13.11239906893445806 ) ) ;
#8125 = CARTESIAN_POINT ( 'NONE',  ( 9.598844408820459861, 38.12265624999999858, 9.598844408820456309 ) ) ;
#8126 = CARTESIAN_POINT ( 'NONE',  ( 143.1451861577818079, 40.40468750108393436, -5.444914386472297529 ) ) ;
#8127 = VERTEX_POINT ( 'NONE', #24787 ) ;
#8128 = CARTESIAN_POINT ( 'NONE',  ( 101.8468681455906903, 83.00000000136559208, 4.458734124999987891 ) ) ;
#8129 = ADVANCED_FACE ( 'NONE', ( #26797 ), #11511, .T. ) ;
#8130 = CARTESIAN_POINT ( 'NONE',  ( 95.54126587499996504, -1.846868145590724986, 0.5000000013655920839 ) ) ;
#8131 = CYLINDRICAL_SURFACE ( 'NONE', #15664, 13.57481594606304398 ) ;
#8132 = ORIENTED_EDGE ( 'NONE', *, *, #17385, .F. ) ;
#8133 = EDGE_CURVE ( 'NONE', #1383, #25390, #1463, .T. ) ;
#8134 =( BOUNDED_CURVE ( )  B_SPLINE_CURVE ( 2, ( #5164, #22550, #22697, #3019, #26978, #5306, #20559, #13969, #11835 ),
 .UNSPECIFIED., .F., .T. ) 
 B_SPLINE_CURVE_WITH_KNOTS ( ( 3, 2, 2, 2, 3 ),
 ( 0.02083333333333358892, 0.03125000000000020123, 0.04166666666666681007, 0.05208333333333342585, 0.06250000000000004163 ),
 .UNSPECIFIED. ) 
 CURVE ( )  GEOMETRIC_REPRESENTATION_ITEM ( )  RATIONAL_B_SPLINE_CURVE ( ( 0.9999999999999981126, 0.9238795325112886259, 1.000000000000000000, 0.9238795325112867385, 1.000000000000000000, 0.9238795325112867385, 1.000000000000000000, 0.9238795325112864054, 1.000000000000000222 ) ) 
 REPRESENTATION_ITEM ( '' )  );
#8135 = VERTEX_POINT ( 'NONE', #12075 ) ;
#8136 = CARTESIAN_POINT ( 'NONE',  ( 129.6752756888039926, 53.49346745874646558, -15.00000000000000355 ) ) ;
#8137 = CARTESIAN_POINT ( 'NONE',  ( 98.15313185440925281, -4.458734124999987891, 6.875000001365592972 ) ) ;
#8138 = ORIENTED_EDGE ( 'NONE', *, *, #19222, .F. ) ;
#8139 = CARTESIAN_POINT ( 'NONE',  ( 106.5389055433251002, 114.7507929638356785, -50.17500000273119554 ) ) ;
#8140 = CARTESIAN_POINT ( 'NONE',  ( -5.444914386472299306, 33.55859375108393294, 13.14518615778179722 ) ) ;
#8141 = CARTESIAN_POINT ( 'NONE',  ( 189.3771271284221314, 37.77539062716788010, -13.57481594606304753 ) ) ;
#8142 = CARTESIAN_POINT ( 'NONE',  ( -9.295050272127046043, 39.66054687608393436, -9.295050272127046043 ) ) ;
#8143 = CARTESIAN_POINT ( 'NONE',  ( 97.50236033167492167, 102.3130555110000159, -50.72500000273119980 ) ) ;
#8144 = CARTESIAN_POINT ( 'NONE',  ( 195.4460412567803189, 49.99999999978059151, 13.57776691409217484 ) ) ;
#8145 = CARTESIAN_POINT ( 'NONE',  ( 135.4449143864723339, 38.61875000108392442, 13.14518615778179189 ) ) ;
#8146 = CARTESIAN_POINT ( 'NONE',  ( 13.14518615778179900, 32.96328125108393436, 5.444914386472293977 ) ) ;
#8147 = ORIENTED_EDGE ( 'NONE', *, *, #14871, .T. ) ;
#8148 = CIRCLE ( 'NONE', #3140, 7.000000000000006217 ) ;
#8149 = CARTESIAN_POINT ( 'NONE',  ( 51.42518405393695957, 37.77539062499999289, -5.622872871577873077 ) ) ;
#8150 = CARTESIAN_POINT ( 'NONE',  ( 99.99999999999998579, 90.00000000000000000, -6.938893903907228378E-15 ) ) ;
#8151 = CARTESIAN_POINT ( 'NONE',  ( 201.8311344573052111, 36.00000000000002842, 11.35217666745979770 ) ) ;
#8152 = CARTESIAN_POINT ( 'NONE',  ( 98.15313185440925281, -4.458734124999987891, 4.625000001365592084 ) ) ;
#8153 = CARTESIAN_POINT ( 'NONE',  ( -9.295050272127046043, 33.50898437608393010, -9.295050272127046043 ) ) ;
#8154 = CARTESIAN_POINT ( 'NONE',  ( 104.4587341249999781, 1.846868145590750521, 4.250000001365592084 ) ) ;
#8155 = DIRECTION ( 'NONE',  ( 0.000000000000000000, -1.000000000000000000, 0.000000000000000000 ) ) ;
#8156 = CARTESIAN_POINT ( 'NONE',  ( 2.414731522848535132E-15, 32.02070312608393010, 13.14518615778179544 ) ) ;
#8157 = CARTESIAN_POINT ( 'NONE',  ( 5.444914386472297529, 40.50390625108394005, -13.14518615778179900 ) ) ;
#8158 = EDGE_CURVE ( 'NONE', #3022, #861, #22822, .T. ) ;
#8159 = DIRECTION ( 'NONE',  ( 5.782411586589357392E-17, -0.000000000000000000, 1.000000000000000000 ) ) ;
#8160 = ORIENTED_EDGE ( 'NONE', *, *, #11572, .T. ) ;
#8161 = CARTESIAN_POINT ( 'NONE',  ( 13.14518615778179722, 33.16171875108393863, 5.444914386472293977 ) ) ;
#8162 = CARTESIAN_POINT ( 'NONE',  ( 99.99999999999998579, 123.5500000010924850, -2.066987299999998751 ) ) ;
#8163 = CARTESIAN_POINT ( 'NONE',  ( 95.54126587499999346, 95.12499999863439371, 1.846868145590722543 ) ) ;
#8164 = CARTESIAN_POINT ( 'NONE',  ( 13.57481594606304931, 31.92148437716787157, 5.622872871577868636 ) ) ;
#8165 = CARTESIAN_POINT ( 'NONE',  ( 101.2031690377821462, 123.0000000000000000, -1.942071768828401490 ) ) ;
#8166 = CARTESIAN_POINT ( 'NONE',  ( -13.57481594606304576, 32.26874999999999716, 0.000000000000000000 ) ) ;
#8167 = MECHANICAL_DESIGN_GEOMETRIC_PRESENTATION_REPRESENTATION (  '', ( #20468 ), #15881 ) ;
#8168 = VERTEX_POINT ( 'NONE', #25072 ) ;
#8169 = CARTESIAN_POINT ( 'NONE',  ( 51.85481384221820633, 37.57695312608393579, 0.000000000000000000 ) ) ;
#8170 = CARTESIAN_POINT ( 'NONE',  ( 94.99999999999995737, 83.06250000273119838, -2.071067811865491493 ) ) ;
#8171 = CARTESIAN_POINT ( 'NONE',  ( 189.5550856135277229, 31.87187500108393223, -13.14518615778179900 ) ) ;
#8172 = VERTEX_POINT ( 'NONE', #23489 ) ;
#8173 = CARTESIAN_POINT ( 'NONE',  ( 104.9999999999999716, 1.449011120738813565E-14, 34.79898987322334136 ) ) ;
#8174 = CARTESIAN_POINT ( 'NONE',  ( -9.180175813648009608, 49.99999999999997868, -14.99999999999999822 ) ) ;
#8175 = CARTESIAN_POINT ( 'NONE',  ( -13.57481594606304576, 33.85624999999999574, 0.000000000000000000 ) ) ;
#8176 = AXIS2_PLACEMENT_3D ( 'NONE', #27930, #10102, #25229 ) ;
#8177 = CARTESIAN_POINT ( 'NONE',  ( 120.4011555911795455, 34.65000000216787868, -9.598844408820458085 ) ) ;
#8178 = CARTESIAN_POINT ( 'NONE',  ( 51.85481384221820633, 39.16445312608393436, 0.000000000000000000 ) ) ;
#8179 = CARTESIAN_POINT ( 'NONE',  ( 5.622872871577786924, 31.82226562716788365, 13.57481594606313813 ) ) ;
#8180 = CARTESIAN_POINT ( 'NONE',  ( 195.0000000000000000, 38.56914062608393579, 13.14518615778179544 ) ) ;
#8181 = ORIENTED_EDGE ( 'NONE', *, *, #430, .F. ) ;
#8182 =( BOUNDED_CURVE ( )  B_SPLINE_CURVE ( 1, ( #13776, #2963 ),
 .UNSPECIFIED., .F., .F. ) 
 B_SPLINE_CURVE_WITH_KNOTS ( ( 2, 2 ),
 ( 0.000000000000000000, 1.000000000000000000 ),
 .UNSPECIFIED. ) 
 CURVE ( )  GEOMETRIC_REPRESENTATION_ITEM ( )  RATIONAL_B_SPLINE_CURVE ( ( 0.9684275710300105366, 0.9684275710300105366 ) ) 
 REPRESENTATION_ITEM ( '' )  );
#8183 = VERTEX_POINT ( 'NONE', #16919 ) ;
#8184 = CARTESIAN_POINT ( 'NONE',  ( 94.99999999999995737, 84.06250000000002842, 2.071067811865466624 ) ) ;
#8185 = CARTESIAN_POINT ( 'NONE',  ( 13.57481594606304753, 39.85898437499999858, -5.622872871577873966 ) ) ;
#8186 = CARTESIAN_POINT ( 'NONE',  ( 104.9999999999999716, 1.449011120738813565E-14, 13.50000000000000000 ) ) ;
#8187 = CARTESIAN_POINT ( 'NONE',  ( 13.57481594606304753, 34.40195312716787157, -5.622872871577873966 ) ) ;
#8188 = CARTESIAN_POINT ( 'NONE',  ( 13.14518615778179722, 40.30546875108393579, 5.444914386472293977 ) ) ;
#8189 = LINE ( 'NONE', #8608, #7748 ) ;
#8190 = CARTESIAN_POINT ( 'NONE',  ( 3.304118597821753767, 35.99999999999998579, 12.77244747738262554 ) ) ;
#8191 = FACE_BOUND ( 'NONE', #20868, .T. ) ;
#8192 = CARTESIAN_POINT ( 'NONE',  ( 124.3771271284221314, 32.41757812499999858, 13.57481594606304753 ) ) ;
#8193 = ORIENTED_EDGE ( 'NONE', *, *, #5894, .F. ) ;
#8194 = CARTESIAN_POINT ( 'NONE',  ( -9.598844408820454532, 39.51171874999999289, 9.598844408820459861 ) ) ;
#8195 = CARTESIAN_POINT ( 'NONE',  ( -5.444914386472297529, 39.61093750108393152, -13.14518615778179900 ) ) ;
#8196 = CARTESIAN_POINT ( 'NONE',  ( 98.15313185440925281, 4.458734125000016313, 14.25000000136559208 ) ) ;
#8197 = CARTESIAN_POINT ( 'NONE',  ( 116.8548138422182205, 39.95820312608393010, 0.000000000000000000 ) ) ;
#8198 = CARTESIAN_POINT ( 'NONE',  ( 70.44491438647230552, 37.62656250108393863, 13.14518615778179189 ) ) ;
#8199 = CARTESIAN_POINT ( 'NONE',  ( 189.5550856135277229, 31.97109375108393436, 13.14518615778179722 ) ) ;
#8200 = FACE_OUTER_BOUND ( 'NONE', #11171, .T. ) ;
#8201 = CARTESIAN_POINT ( 'NONE',  ( 2.414731522848535132E-15, 35.19570312608392726, 13.14518615778179544 ) ) ;
#8202 = CARTESIAN_POINT ( 'NONE',  ( 199.1572863549628210, 35.99999999999999289, -12.92256159328821141 ) ) ;
#8203 = DIRECTION ( 'NONE',  ( -0.000000000000000000, 1.000000000000000000, -0.000000000000000000 ) ) ;
#8204 = CARTESIAN_POINT ( 'NONE',  ( 195.0000000000000000, -7.395377635281828788, 11.57481594606302266 ) ) ;
#8205 = ADVANCED_FACE ( 'NONE', ( #16653 ), #5560, .T. ) ;
#8206 = VERTEX_POINT ( 'NONE', #18660 ) ;
#8207 = CARTESIAN_POINT ( 'NONE',  ( -13.14518615778179544, 38.17226562608393436, 0.000000000000000000 ) ) ;
#8208 = CARTESIAN_POINT ( 'NONE',  ( 0.7197605961091595450, 53.51499872091925170, 14.99999999999999645 ) ) ;
#8209 = CARTESIAN_POINT ( 'NONE',  ( 97.50000000000000000, 123.4069999999781402, -9.540979117872439019E-15 ) ) ;
#8210 = CARTESIAN_POINT ( 'NONE',  ( 100.8561741729129153, 124.5000000010924737, -2.066987299999999195 ) ) ;
#8211 = CARTESIAN_POINT ( 'NONE',  ( 98.53841926354351699, 124.6500000010924651, -1.461580736456474794 ) ) ;
#8212 = SURFACE_STYLE_FILL_AREA ( #14750 ) ;
#8213 = CARTESIAN_POINT ( 'NONE',  ( 103.1528011352953342, 3.152801135295383084, 11.06250000136559208 ) ) ;
#8214 = EDGE_LOOP ( 'NONE', ( #13599, #2978, #2528, #13989 ) ) ;
#8215 = CARTESIAN_POINT ( 'NONE',  ( 99.99999999999997158, 102.6397644303321215, -49.99999999453764588 ) ) ;
#8216 = CARTESIAN_POINT ( 'NONE',  ( 13.14518615778179544, 32.41757812608393863, -1.609821015232357215E-15 ) ) ;
#8217 = CARTESIAN_POINT ( 'NONE',  ( 13.14518615778179722, 32.16953125108393152, 5.444914386472293977 ) ) ;
#8218 = CARTESIAN_POINT ( 'NONE',  ( 5.622872871577871301, 34.50117187716788436, -13.57481594606304753 ) ) ;
#8219 = LINE ( 'NONE', #23207, #14916 ) ;
#8220 = CARTESIAN_POINT ( 'NONE',  ( 104.4587341249999781, 81.00000000136560629, -1.846868145590750299 ) ) ;
#8221 = CARTESIAN_POINT ( 'NONE',  ( 51.85481384221819923, 39.11484375108394573, -5.444914386472297529 ) ) ;
#8222 = CARTESIAN_POINT ( 'NONE',  ( 93.46109445667491400, 114.7507929638356785, -45.57500000273119412 ) ) ;
#8223 = CARTESIAN_POINT ( 'NONE',  ( 104.9999999999999716, 1.449011120738813565E-14, 11.50000000000000000 ) ) ;
#8224 = CARTESIAN_POINT ( 'NONE',  ( 101.4615807364564546, 122.8500000010924680, -1.461580736456474794 ) ) ;
#8225 = CARTESIAN_POINT ( 'NONE',  ( 143.5748159460630688, 39.06523437499999574, -5.622872871577873966 ) ) ;
#8226 = CARTESIAN_POINT ( 'NONE',  ( 107.0000000000000000, 112.2744378736303332, -51.39999999453764445 ) ) ;
#8227 = CARTESIAN_POINT ( 'NONE',  ( 116.4251840539369596, 39.46210937499999005, 5.622872871577880183 ) ) ;
#8228 = EDGE_LOOP ( 'NONE', ( #16188, #23958, #18976, #4951 ) ) ;
#8229 = CARTESIAN_POINT ( 'NONE',  ( 7.623941961925452482, 55.00000000000001421, -15.00000000000000000 ) ) ;
#8230 = CARTESIAN_POINT ( 'NONE',  ( 13.14518615778179544, 38.76757812608393294, -1.609821015232357215E-15 ) ) ;
#8231 = CARTESIAN_POINT ( 'NONE',  ( 98.15313185440925281, 79.62500000136560629, 4.458734124999987891 ) ) ;
#8232 = CARTESIAN_POINT ( 'NONE',  ( 96.46446609406726225, 94.62500000000000000, 3.535533905932723986 ) ) ;
#8233 = CARTESIAN_POINT ( 'NONE',  ( 70.62287287157786864, 38.46992187716787015, -13.57481594606304753 ) ) ;
#8234 = AXIS2_PLACEMENT_3D ( 'NONE', #5606, #24983, #18430 ) ;
#8235 = CARTESIAN_POINT ( 'NONE',  ( 93.00000000000000000, 110.0000000000000000, -55.00000000000000711 ) ) ;
#8236 = CARTESIAN_POINT ( 'NONE',  ( 13.57481594606304753, 35.19570312716788152, -5.622872871577873077 ) ) ;
#8237 = EDGE_LOOP ( 'NONE', ( #13369, #40, #1747, #26526 ) ) ;
#8238 = CARTESIAN_POINT ( 'NONE',  ( 99.99999999999995737, 5.000000000000018652, 6.749999999999999112 ) ) ;
#8239 = CARTESIAN_POINT ( 'NONE',  ( 97.83688103937538472, 116.6573956140660897, -46.90000000546238113 ) ) ;
#8240 = CARTESIAN_POINT ( 'NONE',  ( 208.1451861577817795, 36.13828125108393863, 5.444914386472293977 ) ) ;
#8241 = EDGE_CURVE ( 'NONE', #12833, #25848, #2538, .T. ) ;
#8242 = CARTESIAN_POINT ( 'NONE',  ( 12.07727640983550188, 36.00000000000000711, -6.197985357349471869 ) ) ;
#8243 = CARTESIAN_POINT ( 'NONE',  ( 143.1451861577818363, 39.41250000108393436, -5.444914386472297529 ) ) ;
#8244 = CARTESIAN_POINT ( 'NONE',  ( 7.279598927625384519, 35.96878166309014802, -11.91808989001553520 ) ) ;
#8245 = EDGE_CURVE ( 'NONE', #24786, #789, #4358, .T. ) ;
#8246 = CARTESIAN_POINT ( 'NONE',  ( 102.0710678118654329, -4.999999999999989342, 11.31249999999999822 ) ) ;
#8247 = CARTESIAN_POINT ( 'NONE',  ( 99.99999999999998579, 93.06249999863440792, 4.458734124999981674 ) ) ;
#8248 = CARTESIAN_POINT ( 'NONE',  ( 99.99999999999997158, 102.6397644303321215, -48.50000000000000711 ) ) ;
#8249 = CARTESIAN_POINT ( 'NONE',  ( -9.295050272127044266, 39.06523437608392868, 9.295050272127047819 ) ) ;
#8250 = CARTESIAN_POINT ( 'NONE',  ( 181.4251840539369596, 37.87460937499999147, 5.622872871577880183 ) ) ;
#8251 = APPLICATION_PROTOCOL_DEFINITION ( 'draft international standard', 'automotive_design', 1998, #1690 ) ;
#8252 = CARTESIAN_POINT ( 'NONE',  ( 6.944423797152706079, 31.55306878032414986, -11.16113333171310451 ) ) ;
#8253 = CARTESIAN_POINT ( 'NONE',  ( 104.4587341249999781, 1.846868145590750299, 4.250000001365592084 ) ) ;
#8254 = CARTESIAN_POINT ( 'NONE',  ( 78.14518615778179367, 39.36289062608393152, -1.609821015232357215E-15 ) ) ;
#8255 = CARTESIAN_POINT ( 'NONE',  ( 101.8468681455907046, 4.458734125000016313, 6.125000001365592084 ) ) ;
#8256 = CARTESIAN_POINT ( 'NONE',  ( 0.000000000000000000, 78.00000000000000000, 0.000000000000000000 ) ) ;
#8257 = CARTESIAN_POINT ( 'NONE',  ( 104.4587341249999781, 93.56249999863440792, -6.938893903907228378E-15 ) ) ;
#8258 = DIRECTION ( 'NONE',  ( 0.000000000000000000, -1.000000000000000000, 0.000000000000000000 ) ) ;
#8259 = CARTESIAN_POINT ( 'NONE',  ( -13.57481594606304576, 39.46210937499999005, 5.622872871577880183 ) ) ;
#8260 = CARTESIAN_POINT ( 'NONE',  ( 116.8548138422182063, 39.90859375108394147, -5.444914386472297529 ) ) ;
#8261 = EDGE_CURVE ( 'NONE', #11873, #8652, #18008, .T. ) ;
#8262 = VERTEX_POINT ( 'NONE', #25487 ) ;
#8263 = CARTESIAN_POINT ( 'NONE',  ( 98.15313185440925281, 82.87500000136560629, 4.458734124999987891 ) ) ;
#8264 = CARTESIAN_POINT ( 'NONE',  ( 96.84719886470463734, 91.68749999863440792, -3.152801135295366208 ) ) ;
#8265 = ORIENTED_EDGE ( 'NONE', *, *, #17331, .T. ) ;
#8266 = CARTESIAN_POINT ( 'NONE',  ( -20.00000000000000355, 55.00000000000000000, -9.999999999999998224 ) ) ;
#8267 = CARTESIAN_POINT ( 'NONE',  ( 51.85481384221820633, 33.65781250108393152, 5.444914386472304635 ) ) ;
#8268 = ORIENTED_EDGE ( 'NONE', *, *, #25843, .T. ) ;
#8269 = FACE_OUTER_BOUND ( 'NONE', #2850, .T. ) ;
#8270 = CARTESIAN_POINT ( 'NONE',  ( 104.4587341249999781, -1.846868145590721655, 5.125000001365592972 ) ) ;
#8271 = VERTEX_POINT ( 'NONE', #14633 ) ;
#8272 = CARTESIAN_POINT ( 'NONE',  ( 5.444914386472302859, 32.86406250108392868, 13.14518615778179189 ) ) ;
#8273 = CARTESIAN_POINT ( 'NONE',  ( 208.5748159460630120, 36.68398437716788152, 5.622872871577869525 ) ) ;
#8274 = EDGE_CURVE ( 'NONE', #19327, #20134, #21386, .T. ) ;
#8275 = CARTESIAN_POINT ( 'NONE',  ( 5.444914386472297529, 39.51171875108393294, -13.14518615778179722 ) ) ;
#8276 = CARTESIAN_POINT ( 'NONE',  ( 84.99999999999998579, 120.0000000000000000, -45.00000000000000711 ) ) ;
#8277 = CARTESIAN_POINT ( 'NONE',  ( 203.3959387412915873, 54.99999999495823744, 14.99999999999994671 ) ) ;
#8278 = CARTESIAN_POINT ( 'NONE',  ( 143.1451861577818363, 39.61093750108393863, -5.444914386472297529 ) ) ;
#8279 = CARTESIAN_POINT ( 'NONE',  ( -5.444914386472297529, 39.80937500108392868, -13.14518615778179900 ) ) ;
#8280 = ORIENTED_EDGE ( 'NONE', *, *, #22594, .T. ) ;
#8281 = CARTESIAN_POINT ( 'NONE',  ( 55.40115559117954547, 36.93203124999999432, -9.598844408820458085 ) ) ;
#8282 = DIRECTION ( 'NONE',  ( 0.000000000000000000, -1.000000000000000000, 0.000000000000000000 ) ) ;
#8283 = EDGE_CURVE ( 'NONE', #15184, #3280, #17621, .T. ) ;
#8284 = CARTESIAN_POINT ( 'NONE',  ( 97.92893218813449607, 83.93750000273119838, -5.000000000000020428 ) ) ;
#8285 = CARTESIAN_POINT ( 'NONE',  ( 104.4587341249999781, -1.846868145590721655, 5.875000001365591196 ) ) ;
#8286 = FACE_OUTER_BOUND ( 'NONE', #13254, .T. ) ;
#8287 = CARTESIAN_POINT ( 'NONE',  ( 96.84719886470459471, 3.152801135295383084, 3.562500001365592972 ) ) ;
#8288 = CARTESIAN_POINT ( 'NONE',  ( 104.4587341249999781, 80.25000000136559208, -1.846868145590750521 ) ) ;
#8289 = CARTESIAN_POINT ( 'NONE',  ( 13.14518615778179900, 33.75703125108393010, 5.444914386472293977 ) ) ;
#8290 = CARTESIAN_POINT ( 'NONE',  ( -13.14518615778179900, 38.32109375108394289, -5.444914386472297529 ) ) ;
#8291 = EDGE_CURVE ( 'NONE', #8513, #11798, #6788, .T. ) ;
#8292 = CARTESIAN_POINT ( 'NONE',  ( 102.4976396683250783, 102.3130555110000159, -47.27499999726882152 ) ) ;
#8293 = VERTEX_POINT ( 'NONE', #26328 ) ;
#8294 =( LENGTH_UNIT ( ) NAMED_UNIT ( * ) SI_UNIT ( .MILLI., .METRE. ) );
#8295 =( BOUNDED_CURVE ( )  B_SPLINE_CURVE ( 2, ( #26708, #22142, #2622, #16707, #25257, #5748, #22716, #20717, #14415 ),
 .UNSPECIFIED., .F., .T. ) 
 B_SPLINE_CURVE_WITH_KNOTS ( ( 3, 2, 2, 2, 3 ),
 ( 0.2708333333333330928, 0.2812499999999998890, 0.2916666666666666852, 0.3020833333333334259, 0.3125000000000002220 ),
 .UNSPECIFIED. ) 
 CURVE ( )  GEOMETRIC_REPRESENTATION_ITEM ( )  RATIONAL_B_SPLINE_CURVE ( ( 1.000000000000001554, 0.9238795325112850731, 1.000000000000000000, 0.9238795325112867385, 1.000000000000000000, 0.9238795325112867385, 1.000000000000000000, 0.9238795325112850731, 1.000000000000001554 ) ) 
 REPRESENTATION_ITEM ( '' )  );
#8296 = CARTESIAN_POINT ( 'NONE',  ( 104.7293670624999748, 90.15624999931721106, -6.938893903907228378E-15 ) ) ;
#8297 = CARTESIAN_POINT ( 'NONE',  ( 98.97035852359087471, 122.9999999999999858, 1.976093766406173735 ) ) ;
#8298 = CARTESIAN_POINT ( 'NONE',  ( 99.99999999999995737, 80.37500000273119838, 4.999999999999990230 ) ) ;
#8299 = CARTESIAN_POINT ( 'NONE',  ( 104.9952793366501709, 116.8754121666685393, -54.57499999726882578 ) ) ;
#8300 = DIRECTION ( 'NONE',  ( -1.000000000000000000, 0.000000000000000000, 0.000000000000000000 ) ) ;
#8301 = EDGE_LOOP ( 'NONE', ( #23669, #19242, #5304, #12669 ) ) ;
#8302 = CARTESIAN_POINT ( 'NONE',  ( 59.55508561352770158, 38.51953125108393294, 13.14518615778179722 ) ) ;
#8303 = CARTESIAN_POINT ( 'NONE',  ( 99.99999999999995737, 82.87500000273119838, -5.000000000000018652 ) ) ;
#8304 = CARTESIAN_POINT ( 'NONE',  ( 185.7049497278729575, 32.11992187608393579, 9.295050272127047819 ) ) ;
#8305 = ORIENTED_EDGE ( 'NONE', *, *, #4038, .T. ) ;
#8306 = CARTESIAN_POINT ( 'NONE',  ( 93.00000000000000000, 110.0000000000000000, -48.00000000000000711 ) ) ;
#8307 = CARTESIAN_POINT ( 'NONE',  ( -4.504887086316538891, 51.44650206076907040, -14.99999999999999645 ) ) ;
#8308 = CARTESIAN_POINT ( 'NONE',  ( 104.9999999999999716, 92.93749999726880162, -2.071067811865478170 ) ) ;
#8309 = CIRCLE ( 'NONE', #581, 0.5000000000000086597 ) ;
#8310 = CARTESIAN_POINT ( 'NONE',  ( 130.0000000000000000, 34.94765625216787441, 13.57481594606304576 ) ) ;
#8311 = CARTESIAN_POINT ( 'NONE',  ( 104.9999999999999716, 81.62500000273119838, -1.449011120738813565E-14 ) ) ;
#8312 = CARTESIAN_POINT ( 'NONE',  ( -8.312177448680279460E-16, 34.55078125216787299, -13.57481594606304576 ) ) ;
#8313 = EDGE_CURVE ( 'NONE', #10673, #9430, #23903, .T. ) ;
#8314 = CARTESIAN_POINT ( 'NONE',  ( 208.1451861577817795, 34.74921875108395142, 5.444914386472293977 ) ) ;
#8315 = ORIENTED_EDGE ( 'NONE', *, *, #5147, .T. ) ;
#8316 = ORIENTED_EDGE ( 'NONE', *, *, #769, .F. ) ;
#8317 = ORIENTED_EDGE ( 'NONE', *, *, #8370, .F. ) ;
#8318 = ORIENTED_EDGE ( 'NONE', *, *, #20993, .T. ) ;
#8319 = CARTESIAN_POINT ( 'NONE',  ( -9.295050272127046043, 32.51679687608393721, -9.295050272127046043 ) ) ;
#8320 = FILL_AREA_STYLE ('',( #8741 ) ) ;
#8321 = CARTESIAN_POINT ( 'NONE',  ( 96.84719886470459471, 3.152801135295383084, 14.56250000136559208 ) ) ;
#8322 = CARTESIAN_POINT ( 'NONE',  ( 97.92893218813451028, 92.18749999726878741, -4.999999999999984013 ) ) ;
#8323 = CARTESIAN_POINT ( 'NONE',  ( 96.84719886470459471, 83.56250000136560629, 3.152801135295355994 ) ) ;
#8324 = CARTESIAN_POINT ( 'NONE',  ( 100.0000000000000000, 110.0000000000000000, -45.00000000000000711 ) ) ;
#8325 = DIRECTION ( 'NONE',  ( 0.000000000000000000, 0.000000000000000000, -1.000000000000000000 ) ) ;
#8326 = CARTESIAN_POINT ( 'NONE',  ( 112.9999999999999858, 123.0000000000000000, 14.99999999999999112 ) ) ;
#8327 = DIRECTION ( 'NONE',  ( 0.000000000000000000, 0.000000000000000000, -1.000000000000000000 ) ) ;
#8328 = FACE_OUTER_BOUND ( 'NONE', #13622, .T. ) ;
#8329 = CARTESIAN_POINT ( 'NONE',  ( 93.46109445667489979, 114.7507929638356785, -45.82499999726881867 ) ) ;
#8330 = AXIS2_PLACEMENT_3D ( 'NONE', #14308, #21163, #14450 ) ;
#8331 = ORIENTED_EDGE ( 'NONE', *, *, #24837, .F. ) ;
#8332 = UNCERTAINTY_MEASURE_WITH_UNIT (LENGTH_MEASURE( 1.000000000000000082E-05 ), #17603, 'distance_accuracy_value', 'NONE');
#8333 = CARTESIAN_POINT ( 'NONE',  ( -9.598844408820458085, 39.31328124999999574, -9.598844408820458085 ) ) ;
#8334 = CARTESIAN_POINT ( 'NONE',  ( -13.14518615778179189, 39.80937500108392868, 5.444914386472304635 ) ) ;
#8335 = CARTESIAN_POINT ( 'NONE',  ( 99.99999999999995737, -4.999999999999990230, 2.375000002731185500 ) ) ;
#8336 = CARTESIAN_POINT ( 'NONE',  ( 139.2950502721270425, 35.69179687608394147, -9.295050272127046043 ) ) ;
#8337 = CARTESIAN_POINT ( 'NONE',  ( 51.85481384221820633, 37.42812500108393436, 5.444914386472304635 ) ) ;
#8338 = CARTESIAN_POINT ( 'NONE',  ( 200.4449143864723055, 38.91640625108393436, -13.14518615778179900 ) ) ;
#8339 = CARTESIAN_POINT ( 'NONE',  ( 54.21315323181566015, 35.99999999999999289, 7.561388982944276194 ) ) ;
#8340 = CARTESIAN_POINT ( 'NONE',  ( 13.14518615778179544, 35.39414062608393152, -1.609821015232357215E-15 ) ) ;
#8341 = CARTESIAN_POINT ( 'NONE',  ( 137.1154903918550758, 49.99999999945652718, -11.58166858714055003 ) ) ;
#8342 = CARTESIAN_POINT ( 'NONE',  ( 196.1371678245420753, 35.99999999999999289, 13.09590655363592582 ) ) ;
#8343 = CARTESIAN_POINT ( 'NONE',  ( 97.50000000000000000, 124.9500000000000028, -1.035533905932742416 ) ) ;
#8344 =( BOUNDED_CURVE ( )  B_SPLINE_CURVE ( 2, ( #7917, #16612, #5793, #21037, #1906, #10572, #19281, #27979, #20760 ),
 .UNSPECIFIED., .F., .F. ) 
 B_SPLINE_CURVE_WITH_KNOTS ( ( 3, 2, 2, 2, 3 ),
 ( 0.3125000000000002220, 0.3229166666666668517, 0.3333333333333334259, 0.3437500000000000555, 0.3541666666666666852 ),
 .UNSPECIFIED. ) 
 CURVE ( )  GEOMETRIC_REPRESENTATION_ITEM ( )  RATIONAL_B_SPLINE_CURVE ( ( 0.9999999999999983347, 0.9238795325112884038, 1.000000000000000000, 0.9238795325112867385, 1.000000000000000000, 0.9238795325112867385, 1.000000000000000000, 0.9238795325112867385, 1.000000000000000000 ) ) 
 REPRESENTATION_ITEM ( '' )  );
#8345 = CARTESIAN_POINT ( 'NONE',  ( -8.049105076161786076E-16, 37.97382812608393721, -13.14518615778179544 ) ) ;
#8346 = CARTESIAN_POINT ( 'NONE',  ( -3.116592080465746761, 53.90895096933311237, 14.99999999999999645 ) ) ;
#8347 = CARTESIAN_POINT ( 'NONE',  ( 101.7677669529663547, 123.8999999999999915, -1.767766952966370209 ) ) ;
#8348 = CARTESIAN_POINT ( 'NONE',  ( 99.99999999999998579, 129.0000000000000000, 12.50000000000001066 ) ) ;
#8349 = CARTESIAN_POINT ( 'NONE',  ( 195.0000000000000000, 37.32890625216786873, 13.57481594606304576 ) ) ;
#8350 = VECTOR ( 'NONE', #5212, 1000.000000000000000 ) ;
#8351 = CARTESIAN_POINT ( 'NONE',  ( 95.54126587499996504, 1.387778780781445676E-14, 12.43750000136559208 ) ) ;
#8352 = CARTESIAN_POINT ( 'NONE',  ( 92.99999999999997158, 107.7255621263696952, -48.40000000546237402 ) ) ;
#8353 = ORIENTED_EDGE ( 'NONE', *, *, #15195, .T. ) ;
#8354 = FACE_OUTER_BOUND ( 'NONE', #27508, .T. ) ;
#8355 = CARTESIAN_POINT ( 'NONE',  ( 95.54126587499995082, -1.846868145590724986, 10.50000000136559208 ) ) ;
#8356 = CARTESIAN_POINT ( 'NONE',  ( 9.295050272127047819, 32.11992187608393579, 9.295050272127046043 ) ) ;
#8357 = CARTESIAN_POINT ( 'NONE',  ( 9.598844408820456309, 32.07031250216787299, -9.598844408820458085 ) ) ;
#8358 = CARTESIAN_POINT ( 'NONE',  ( 99.99999999999995737, 5.000000000000018652, 2.749999999999999112 ) ) ;
#8359 = CARTESIAN_POINT ( 'NONE',  ( 104.4587341249999639, 79.93750000136559208, -1.442382525525748735E-14 ) ) ;
#8360 = CARTESIAN_POINT ( 'NONE',  ( 78.14518615778179367, 38.02343750108395426, -5.444914386472297529 ) ) ;
#8361 = CARTESIAN_POINT ( 'NONE',  ( 95.00472066334982912, 116.8754121666685393, -45.67500000273119554 ) ) ;
#8362 = CARTESIAN_POINT ( 'NONE',  ( 107.0000000000000000, 110.0000000000000000, -145.0000000000000284 ) ) ;
#8363 = ORIENTED_EDGE ( 'NONE', *, *, #17839, .F. ) ;
#8364 = CARTESIAN_POINT ( 'NONE',  ( 99.14382582708707048, 122.8000000010924708, -2.066987299999999195 ) ) ;
#8365 = PLANE ( 'NONE',  #27271 ) ;
#8366 = CARTESIAN_POINT ( 'NONE',  ( 94.33688103937535629, 105.8855032339526758, -52.29999999453764303 ) ) ;
#8367 = CARTESIAN_POINT ( 'NONE',  ( 136.9444236247691151, 31.75150628229955529, -11.16113343896966370 ) ) ;
#8368 = ORIENTED_EDGE ( 'NONE', *, *, #11906, .T. ) ;
#8369 = DIRECTION ( 'NONE',  ( 0.000000000000000000, -1.000000000000000000, 0.000000000000000000 ) ) ;
#8370 = EDGE_CURVE ( 'NONE', #12194, #15376, #16920, .T. ) ;
#8371 = CARTESIAN_POINT ( 'NONE',  ( 2.414731522848535132E-15, 39.36289062608393152, 13.14518615778179544 ) ) ;
#8372 = CARTESIAN_POINT ( 'NONE',  ( 104.4587341249999781, 80.87500000136560629, 1.846868145590721655 ) ) ;
#8373 = LINE ( 'NONE', #10218, #22520 ) ;
#8374 = CARTESIAN_POINT ( 'NONE',  ( 51.42518405393695957, 35.59257812716788294, 5.622872871577880183 ) ) ;
#8375 = CARTESIAN_POINT ( 'NONE',  ( 104.9952793366501709, 116.8754121666685393, -52.32499999726881867 ) ) ;
#8376 = CARTESIAN_POINT ( 'NONE',  ( 13.57481594606304753, 34.40195312716787157, -5.622872871577873077 ) ) ;
#8377 = EDGE_LOOP ( 'NONE', ( #3418, #26870, #2883, #14718 ) ) ;
#8378 = CARTESIAN_POINT ( 'NONE',  ( 103.5355339059327093, 3.535533905932755072, 5.625000000000000000 ) ) ;
#8379 = VERTEX_POINT ( 'NONE', #2395 ) ;
#8380 = CARTESIAN_POINT ( 'NONE',  ( 195.0000000000000000, 37.57695312608392868, 13.14518615778179544 ) ) ;
#8381 =( BOUNDED_SURFACE ( )  B_SPLINE_SURFACE ( 1, 2, ( 
 ( #16983, #21700, #17120, #4171, #2033, #10701, #6440, #10566, #27838, #21559, #21421, #15110, #4588, #4031, #8292, #12968, #23830, #33, #2175, #1900, #2320, #13105, #17408, #25824, #2456, #19552, #11118, #4451, #8858, #6164, #14830, #12832, #10837, #19275, #4311, #13248, #27973, #23554, #26107, #6572, #15255, #23973, #8431, #10977, #21844, #19689, #6298, #14975, #176, #23694, #17549, #26253, #8576, #17266, #25967, #6713, #15399, #24112, #21980, #22939, #14221, #24392, #11796, #19832, #18373, #24926, #4734, #20797, #9811, #6854, #18517, #13394, #9142, #15543, #3402, #27078, #7820, #26399, #5412, #25069, #3269, #9670, #12072, #11937, #20659, #1277, #1144, #24252, #7530, #23074, #3130, #317, #5556, #27361, #7676, #20519, #27222, #4880, #13544, #26540, #16368 ),
 ( #22266, #1001, #9942, #6996, #9005, #16226, #22122, #18657, #15690, #16512, #14080, #3550, #22800, #25205, #5691, #14358, #17697, #2601, #11262, #19983, #461, #17835, #18789, #23761, #27768, #12767, #19340, #21071, #10351, #3822, #6099, #1559, #15044, #20934, #23485, #23626, #7951, #14905, #12626, #4102, #21209, #3966, #25344, #5829, #10077, #25901, #27905, #25484, #28044, #8226, #8511, #14766, #23214, #19060, #25755, #14497, #5962, #12482, #8366, #18922, #1418, #14630, #3689, #10496, #27630, #19203, #8090, #12207, #16785, #23349, #1694, #21485, #17194, #10634, #6371, #25616, #1966, #16916, #27496, #16649, #21352, #12353, #10212, #1832, #17051, #6237, #26325, #13036, #7062, #12897, #15470, #15618, #28180, #6924, #4662, #24320, #13177, #24184, #17339, #26036, #2103 ) ),
 .UNSPECIFIED., .F., .F., .F. ) 
 B_SPLINE_SURFACE_WITH_KNOTS ( ( 2, 2 ),
 ( 3, 2, 2, 2, 2, 2, 2, 2, 2, 2, 2, 2, 2, 2, 2, 2, 2, 2, 2, 2, 2, 2, 2, 2, 2, 2, 2, 2, 2, 2, 2, 2, 2, 2, 2, 2, 2, 2, 2, 2, 2, 2, 2, 2, 2, 2, 2, 2, 2, 2, 3 ),
 ( 0.000000000000000000, 1.000000000000000000 ),
 ( 0.000000000000000000, 0.02000000000000000042, 0.04000000000000000083, 0.05999999999999999778, 0.08000000000000000167, 0.1000000000000000056, 0.1199999999999999956, 0.1400000000000000133, 0.1600000000000000033, 0.1799999999999999933, 0.2000000000000000111, 0.2200000000000000011, 0.2399999999999999911, 0.2600000000000000089, 0.2800000000000000266, 0.2999999999999999889, 0.3200000000000000067, 0.3400000000000000244, 0.3599999999999999867, 0.3800000000000000044, 0.4000000000000000222, 0.4199999999999999845, 0.4400000000000000022, 0.4600000000000000200, 0.4799999999999999822, 0.5000000000000000000, 0.5200000000000000178, 0.5400000000000000355, 0.5600000000000000533, 0.5799999999999999600, 0.5999999999999999778, 0.6199999999999999956, 0.6400000000000000133, 0.6600000000000000311, 0.6800000000000000488, 0.6999999999999999556, 0.7199999999999999734, 0.7399999999999999911, 0.7600000000000000089, 0.7800000000000000266, 0.8000000000000000444, 0.8199999999999999512, 0.8399999999999999689, 0.8599999999999999867, 0.8800000000000000044, 0.9000000000000000222, 0.9200000000000000400, 0.9399999999999999467, 0.9599999999999999645, 0.9799999999999999822, 1.000000000000000000 ),
 .UNSPECIFIED. ) 
 GEOMETRIC_REPRESENTATION_ITEM ( )  RATIONAL_B_SPLINE_SURFACE ( (
 ( 1.000000000000000000, 0.9510565162951535312, 1.000000000000000000, 0.9510565162951535312, 1.000000000000000000, 0.9510565162951535312, 1.000000000000000000, 0.9510565162951535312, 1.000000000000000000, 0.9510565162951535312, 1.000000000000000000, 0.9510565162951535312, 1.000000000000000000, 0.9510565162951535312, 1.000000000000000000, 0.9510565162951535312, 1.000000000000000000, 0.9510565162951535312, 1.000000000000000000, 0.9510565162951535312, 1.000000000000000000, 0.9510565162951535312, 1.000000000000000000, 0.9510565162951535312, 1.000000000000000000, 0.9510565162951535312, 1.000000000000000000, 0.9510565162951535312, 1.000000000000000000, 0.9510565162951535312, 1.000000000000000000, 0.9510565162951535312, 1.000000000000000000, 0.9510565162951535312, 1.000000000000000000, 0.9510565162951535312, 1.000000000000000000, 0.9510565162951535312, 1.000000000000000000, 0.9510565162951535312, 1.000000000000000000, 0.9510565162951535312, 1.000000000000000000, 0.9510565162951535312, 1.000000000000000000, 0.9510565162951535312, 1.000000000000000000, 0.9510565162951535312, 1.000000000000000000, 0.9510565162951535312, 1.000000000000000000, 0.9510565162951535312, 1.000000000000000000, 0.9510565162951535312, 1.000000000000000000, 0.9510565162951535312, 1.000000000000000000, 0.9510565162951535312, 1.000000000000000000, 0.9510565162951535312, 1.000000000000000000, 0.9510565162951535312, 1.000000000000000000, 0.9510565162951535312, 1.000000000000000000, 0.9510565162951535312, 1.000000000000000000, 0.9510565162951535312, 1.000000000000000000, 0.9510565162951535312, 1.000000000000000000, 0.9510565162951535312, 1.000000000000000000, 0.9510565162951535312, 1.000000000000000000, 0.9510565162951535312, 1.000000000000000000, 0.9510565162951535312, 1.000000000000000000, 0.9510565162951535312, 1.000000000000000000, 0.9510565162951535312, 1.000000000000000000, 0.9510565162951535312, 1.000000000000000000, 0.9510565162951535312, 1.000000000000000000, 0.9510565162951535312, 1.000000000000000000, 0.9510565162951535312, 1.000000000000000000, 0.9510565162951535312, 1.000000000000000000, 0.9510565162951535312, 1.000000000000000000, 0.9510565162951535312, 1.000000000000000000, 0.9510565162951535312, 1.000000000000000000, 0.9510565162951535312, 1.000000000000000000),
 ( 1.000000000000000000, 0.9510565162951535312, 1.000000000000000000, 0.9510565162951535312, 1.000000000000000000, 0.9510565162951535312, 1.000000000000000000, 0.9510565162951535312, 1.000000000000000000, 0.9510565162951535312, 1.000000000000000000, 0.9510565162951535312, 1.000000000000000000, 0.9510565162951535312, 1.000000000000000000, 0.9510565162951535312, 1.000000000000000000, 0.9510565162951535312, 1.000000000000000000, 0.9510565162951535312, 1.000000000000000000, 0.9510565162951535312, 1.000000000000000000, 0.9510565162951535312, 1.000000000000000000, 0.9510565162951535312, 1.000000000000000000, 0.9510565162951535312, 1.000000000000000000, 0.9510565162951535312, 1.000000000000000000, 0.9510565162951535312, 1.000000000000000000, 0.9510565162951535312, 1.000000000000000000, 0.9510565162951535312, 1.000000000000000000, 0.9510565162951535312, 1.000000000000000000, 0.9510565162951535312, 1.000000000000000000, 0.9510565162951535312, 1.000000000000000000, 0.9510565162951535312, 1.000000000000000000, 0.9510565162951535312, 1.000000000000000000, 0.9510565162951535312, 1.000000000000000000, 0.9510565162951535312, 1.000000000000000000, 0.9510565162951535312, 1.000000000000000000, 0.9510565162951535312, 1.000000000000000000, 0.9510565162951535312, 1.000000000000000000, 0.9510565162951535312, 1.000000000000000000, 0.9510565162951535312, 1.000000000000000000, 0.9510565162951535312, 1.000000000000000000, 0.9510565162951535312, 1.000000000000000000, 0.9510565162951535312, 1.000000000000000000, 0.9510565162951535312, 1.000000000000000000, 0.9510565162951535312, 1.000000000000000000, 0.9510565162951535312, 1.000000000000000000, 0.9510565162951535312, 1.000000000000000000, 0.9510565162951535312, 1.000000000000000000, 0.9510565162951535312, 1.000000000000000000, 0.9510565162951535312, 1.000000000000000000, 0.9510565162951535312, 1.000000000000000000, 0.9510565162951535312, 1.000000000000000000, 0.9510565162951535312, 1.000000000000000000, 0.9510565162951535312, 1.000000000000000000, 0.9510565162951535312, 1.000000000000000000, 0.9510565162951535312, 1.000000000000000000, 0.9510565162951535312, 1.000000000000000000, 0.9510565162951535312, 1.000000000000000000, 0.9510565162951535312, 1.000000000000000000, 0.9510565162951535312, 1.000000000000000000) ) ) 
 REPRESENTATION_ITEM ( '' )  SURFACE ( )  );
#8382 = CARTESIAN_POINT ( 'NONE',  ( -13.57481594606304576, 38.61874999999999147, 0.000000000000000000 ) ) ;
#8383 = CARTESIAN_POINT ( 'NONE',  ( 143.1451861577818363, 37.82500000108392868, -5.444914386472297529 ) ) ;
#8384 = CARTESIAN_POINT ( 'NONE',  ( 99.99999999999998579, 89.99899999999999523, -9.540979117872439019E-15 ) ) ;
#8385 = DIRECTION ( 'NONE',  ( -1.000000000000000000, 0.000000000000000000, 2.385244779468110248E-16 ) ) ;
#8386 = LINE ( 'NONE', #2125, #15702 ) ;
#8387 = CARTESIAN_POINT ( 'NONE',  ( -9.295050272127046043, 39.66054687608393436, -9.295050272127046043 ) ) ;
#8388 = CARTESIAN_POINT ( 'NONE',  ( 208.5748159460630120, 38.96601562499999005, 5.622872871577869525 ) ) ;
#8389 = CARTESIAN_POINT ( 'NONE',  ( 55.40115559117954547, 39.31328124999999574, -9.598844408820458085 ) ) ;
#8390 = CARTESIAN_POINT ( 'NONE',  ( 101.8468681455906903, 4.458734125000016313, 3.375000001365592972 ) ) ;
#8391 = CARTESIAN_POINT ( 'NONE',  ( 70.44491438647230552, 38.71796875108393721, -13.14518615778179900 ) ) ;
#8392 = CARTESIAN_POINT ( 'NONE',  ( 95.54126587499996504, -1.846868145590724986, 6.500000001365592084 ) ) ;
#8393 = FACE_OUTER_BOUND ( 'NONE', #10714, .T. ) ;
#8394 = CARTESIAN_POINT ( 'NONE',  ( 101.8468681455907330, 94.49999999863442213, -4.458734124999994997 ) ) ;
#8395 = CARTESIAN_POINT ( 'NONE',  ( -12.05655202970020312, 36.00000000000000000, 5.307619621752285965 ) ) ;
#8396 = CARTESIAN_POINT ( 'NONE',  ( 2.493653234604083739E-15, 38.81718749999999574, 13.57481594606304576 ) ) ;
#8397 = CARTESIAN_POINT ( 'NONE',  ( 120.7049497278729575, 39.85898437608393152, -9.295050272127046043 ) ) ;
#8398 = ORIENTED_EDGE ( 'NONE', *, *, #5495, .T. ) ;
#8399 = CARTESIAN_POINT ( 'NONE',  ( 95.54126587499995082, 81.75000000136560629, 1.846868145590724986 ) ) ;
#8400 = AXIS2_PLACEMENT_3D ( 'NONE', #10023, #21016, #6043 ) ;
#8401 = CARTESIAN_POINT ( 'NONE',  ( 104.4587341249999781, 90.31249999863440792, -6.938893903907228378E-15 ) ) ;
#8402 = VERTEX_POINT ( 'NONE', #19762 ) ;
#8403 = FACE_OUTER_BOUND ( 'NONE', #22838, .T. ) ;
#8404 = CARTESIAN_POINT ( 'NONE',  ( 65.00000000000000000, 35.79101562608394005, -13.14518615778179544 ) ) ;
#8405 = ORIENTED_EDGE ( 'NONE', *, *, #14283, .F. ) ;
#8406 = LINE ( 'NONE', #25942, #8525 ) ;
#8407 = CARTESIAN_POINT ( 'NONE',  ( 96.84719886470459471, -3.152801135295355994, 2.812500001365592528 ) ) ;
#8408 = EDGE_LOOP ( 'NONE', ( #9154, #6882, #10112, #14093 ) ) ;
#8409 = CARTESIAN_POINT ( 'NONE',  ( -13.14518615778179722, 35.14609375108393152, -5.444914386472297529 ) ) ;
#8410 = CARTESIAN_POINT ( 'NONE',  ( 6.944426393311538881, 31.55306875057403104, -11.16113171639042356 ) ) ;
#8411 = CARTESIAN_POINT ( 'NONE',  ( 204.5988444088204403, 38.42031250216787441, -9.598844408820458085 ) ) ;
#8412 = CARTESIAN_POINT ( 'NONE',  ( -13.14518615778179722, 36.53515625108393294, -5.444914386472297529 ) ) ;
#8413 = CARTESIAN_POINT ( 'NONE',  ( 199.5048870863314505, 51.44650206076381238, 14.99999999999995381 ) ) ;
#8414 = CARTESIAN_POINT ( 'NONE',  ( 143.1451861577818363, 39.51171875108393294, 5.444914386472293977 ) ) ;
#8415 = CARTESIAN_POINT ( 'NONE',  ( 9.295050272127046043, 38.86679687608393863, -9.295050272127046043 ) ) ;
#8416 = VECTOR ( 'NONE', #15402, 1000.000000000000000 ) ;
#8417 = VERTEX_POINT ( 'NONE', #15473 ) ;
#8418 = CARTESIAN_POINT ( 'NONE',  ( 120.7049497278729575, 34.10429687608393579, -9.295050272127046043 ) ) ;
#8419 = CARTESIAN_POINT ( 'NONE',  ( 51.42518405393695957, 38.66835937499999432, 5.622872871577880183 ) ) ;
#8420 = LINE ( 'NONE', #23820, #6841 ) ;
#8421 = CARTESIAN_POINT ( 'NONE',  ( 98.15313185440925281, -4.458734124999987891, 0.6250000013655921949 ) ) ;
#8422 = ADVANCED_FACE ( 'NONE', ( #21775 ), #15047, .F. ) ;
#8423 =( BOUNDED_CURVE ( )  B_SPLINE_CURVE ( 2, ( #21531, #19383, #10255, #8, #19107, #4146, #14670, #21254, #18965 ),
 .UNSPECIFIED., .F., .T. ) 
 B_SPLINE_CURVE_WITH_KNOTS ( ( 3, 2, 2, 2, 3 ),
 ( 0.8541666666666662966, 0.8645833333333331483, 0.8750000000000000000, 0.8854166666666667407, 0.8958333333333335924 ),
 .UNSPECIFIED. ) 
 CURVE ( )  GEOMETRIC_REPRESENTATION_ITEM ( )  RATIONAL_B_SPLINE_CURVE ( ( 1.000000000000002442, 0.9238795325112842960, 1.000000000000000000, 0.9238795325112867385, 1.000000000000000000, 0.9238795325112867385, 1.000000000000000000, 0.9238795325112850731, 1.000000000000001554 ) ) 
 REPRESENTATION_ITEM ( '' )  );
#8424 = CARTESIAN_POINT ( 'NONE',  ( 99.99999999999995737, 4.458734125000016313, 4.187500001365592084 ) ) ;
#8425 = CARTESIAN_POINT ( 'NONE',  ( 95.00472066334982912, 116.8754121666685393, -49.42500000273118133 ) ) ;
#8426 = CARTESIAN_POINT ( 'NONE',  ( 104.4587341249999639, 1.442382525525748735E-14, 4.187500001365592084 ) ) ;
#8427 = VECTOR ( 'NONE', #14609, 1000.000000000000000 ) ;
#8428 = DIRECTION ( 'NONE',  ( 0.000000000000000000, 0.000000000000000000, 1.000000000000000000 ) ) ;
#8429 = CARTESIAN_POINT ( 'NONE',  ( 95.00472066334981491, 116.8754121666685393, -45.92499999726882720 ) ) ;
#8430 = CARTESIAN_POINT ( 'NONE',  ( -13.14518615778179544, 38.37070312608393152, 0.000000000000000000 ) ) ;
#8431 = CARTESIAN_POINT ( 'NONE',  ( 93.46109445667489979, 114.7507929638356785, -50.07499999726882578 ) ) ;
#8432 = EDGE_LOOP ( 'NONE', ( #22714, #14124, #25207, #4537, #6695 ) ) ;
#8433 = FILL_AREA_STYLE ('',( #25415 ) ) ;
#8435 = EDGE_CURVE ( 'NONE', #1369, #15719, #24188, .T. ) ;
#8434 = DIRECTION ( 'NONE',  ( -1.000000000000000000, 0.000000000000000000, 2.385244779468110248E-16 ) ) ;
#8436 = CARTESIAN_POINT ( 'NONE',  ( 13.57481594606304753, 35.09648437499999574, -5.622872871577873966 ) ) ;
#8437 = CARTESIAN_POINT ( 'NONE',  ( 91.91746824999997045, 112.6261737610028320, -53.97499999726881725 ) ) ;
#8438 = DIRECTION ( 'NONE',  ( 0.000000000000000000, -0.000000000000000000, 1.000000000000000000 ) ) ;
#8439 = ADVANCED_FACE ( 'NONE', ( #19206 ), #27908, .T. ) ;
#8440 = VECTOR ( 'NONE', #6057, 1000.000000000000000 ) ;
#8441 = CARTESIAN_POINT ( 'NONE',  ( 189.5550856135277229, 39.11484375108394573, 13.14518615778179722 ) ) ;
#8442 = ORIENTED_EDGE ( 'NONE', *, *, #25568, .T. ) ;
#8443 = DIRECTION ( 'NONE',  ( -0.000000000000000000, 1.000000000000000000, -0.000000000000000000 ) ) ;
#8444 = EDGE_CURVE ( 'NONE', #13216, #8588, #10915, .T. ) ;
#8445 = CARTESIAN_POINT ( 'NONE',  ( 96.46446609406721961, 83.00000000273119838, -3.535533905932755072 ) ) ;
#8446 = CARTESIAN_POINT ( 'NONE',  ( 55.81982418635200816, 55.00000000000000000, -14.99999999999999822 ) ) ;
#8447 = ORIENTED_EDGE ( 'NONE', *, *, #10719, .T. ) ;
#8448 = CARTESIAN_POINT ( 'NONE',  ( 99.99999999999998579, 102.6397644303321215, -53.50000000000000711 ) ) ;
#8449 = CARTESIAN_POINT ( 'NONE',  ( 0.000000000000000000, 40.99999999999999289, 0.000000000000000000 ) ) ;
#8450 = CIRCLE ( 'NONE', #12083, 13.57481594606304398 ) ;
#8451 = CARTESIAN_POINT ( 'NONE',  ( 102.0669872999999939, 123.6000000010924680, -0.8561741729129507261 ) ) ;
#8452 = EDGE_CURVE ( 'NONE', #637, #21530, #23585, .T. ) ;
#8453 = CARTESIAN_POINT ( 'NONE',  ( 135.6228728715778971, 35.79101562716787299, 13.57481594606304576 ) ) ;
#8454 = LINE ( 'NONE', #14715, #1057 ) ;
#8455 = CARTESIAN_POINT ( 'NONE',  ( -5.622872871577737186, 34.89804687716787157, 13.57481594606318254 ) ) ;
#8456 = CARTESIAN_POINT ( 'NONE',  ( 195.0000000000000000, 35.79101562608394005, -13.14518615778179544 ) ) ;
#8457 = ORIENTED_EDGE ( 'NONE', *, *, #84, .T. ) ;
#8458 = ORIENTED_EDGE ( 'NONE', *, *, #27445, .F. ) ;
#8459 = CARTESIAN_POINT ( 'NONE',  ( -9.295050272127044266, 40.05742187608393579, 9.295050272127047819 ) ) ;
#8460 =( NAMED_UNIT ( * ) PLANE_ANGLE_UNIT ( ) SI_UNIT ( $, .RADIAN. ) );
#8461 = DIRECTION ( 'NONE',  ( -0.000000000000000000, 1.000000000000000000, -0.000000000000000000 ) ) ;
#8462 =( BOUNDED_CURVE ( )  B_SPLINE_CURVE ( 2, ( #24541, #9423, #5025, #11690, #13691, #18122, #9713, #26836, #1040 ),
 .UNSPECIFIED., .F., .T. ) 
 B_SPLINE_CURVE_WITH_KNOTS ( ( 3, 2, 2, 2, 3 ),
 ( 0.4791666666666667962, 0.4895833333333333703, 0.5000000000000000000, 0.5104166666666665186, 0.5208333333333332593 ),
 .UNSPECIFIED. ) 
 CURVE ( )  GEOMETRIC_REPRESENTATION_ITEM ( )  RATIONAL_B_SPLINE_CURVE ( ( 0.9999999999999992228, 0.9238795325112875156, 1.000000000000000000, 0.9238795325112867385, 1.000000000000000000, 0.9238795325112867385, 1.000000000000000000, 0.9238795325112875156, 0.9999999999999992228 ) ) 
 REPRESENTATION_ITEM ( '' )  );
#8463 = CARTESIAN_POINT ( 'NONE',  ( 103.5355339059327235, 94.87500000000000000, 3.535533905932724874 ) ) ;
#8464 = EDGE_CURVE ( 'NONE', #3050, #2793, #10637, .T. ) ;
#8465 = CARTESIAN_POINT ( 'NONE',  ( 98.15313185440923860, 80.62500000136559208, 4.458734124999987891 ) ) ;
#8466 = CARTESIAN_POINT ( 'NONE',  ( 181.8548138422182205, 38.96601562608393721, 0.000000000000000000 ) ) ;
#8467 = CARTESIAN_POINT ( 'NONE',  ( 5.444914386472302859, 40.20625000108394431, 13.14518615778179189 ) ) ;
#8468 = CARTESIAN_POINT ( 'NONE',  ( 102.4999999999999858, 123.0000000000000000, -8.724596124144689908E-15 ) ) ;
#8469 = AXIS2_PLACEMENT_3D ( 'NONE', #22618, #11609, #22761 ) ;
#8470 = DIRECTION ( 'NONE',  ( 0.000000000000000000, 0.000000000000000000, -1.000000000000000000 ) ) ;
#8471 = CARTESIAN_POINT ( 'NONE',  ( 200.4449143864723055, 39.71015625108393010, -13.14518615778179722 ) ) ;
#8472 = CARTESIAN_POINT ( 'NONE',  ( 95.00472066334982912, 116.8754121666685393, -47.92499999726882010 ) ) ;
#8473 = ORIENTED_EDGE ( 'NONE', *, *, #16314, .T. ) ;
#8474 = ADVANCED_FACE ( 'NONE', ( #19343 ), #8514, .F. ) ;
#8475 = CARTESIAN_POINT ( 'NONE',  ( 5.622872871577878406, 35.69179687499999432, 13.57481594606304576 ) ) ;
#8476 = CARTESIAN_POINT ( 'NONE',  ( -5.444914386472297529, 36.43593750108392726, -13.14518615778179900 ) ) ;
#8477 = CARTESIAN_POINT ( 'NONE',  ( 94.99999999999995737, 1.387778780781445676E-14, 2.125000002731185056 ) ) ;
#8478 = CARTESIAN_POINT ( 'NONE',  ( 139.2950502721270425, 37.87460937608393863, 9.295050272127046043 ) ) ;
#8479 = CARTESIAN_POINT ( 'NONE',  ( 51.85481384221820633, 38.17226562608393436, 0.000000000000000000 ) ) ;
#8480 = B_SPLINE_CURVE_WITH_KNOTS ( 'NONE', 3,
 ( #6005, #23805, #6417, #25798, #1598, #27671, #12940, #8136, #4283, #12808, #16830, #10675, #25526, #10400, #27814, #10812, #8693, #14951 ),
 .UNSPECIFIED., .F., .F.,
 ( 4, 2, 2, 2, 2, 2, 2, 2, 4 ),
 ( 0.000000000000000000, 0.004618502246277096830, 0.006927753369415644812, 0.009237004492554193660, 0.01039163005412350842, 0.01154625561569282317, 0.01385550673883145616, 0.01616475786197005271, 0.01847400898510864406 ),
 .UNSPECIFIED. ) ;
#8481 = EDGE_CURVE ( 'NONE', #23831, #15488, #21631, .T. ) ;
#8482 = CARTESIAN_POINT ( 'NONE',  ( 208.1451861577817795, 39.61093750108393863, -5.444914386472297529 ) ) ;
#8483 = DIRECTION ( 'NONE',  ( 0.000000000000000000, -0.000000000000000000, -1.000000000000000000 ) ) ;
#8484 = CARTESIAN_POINT ( 'NONE',  ( -5.444914386472299306, 35.14609375108393152, 13.14518615778179722 ) ) ;
#8485 = CARTESIAN_POINT ( 'NONE',  ( 138.2113140151611788, 50.68678854790365307, -15.00000000000138201 ) ) ;
#8486 = CIRCLE ( 'NONE', #20342, 5.000000000000000000 ) ;
#8487 = CARTESIAN_POINT ( 'NONE',  ( 102.0710678118654329, 5.000000000000018652, 9.812500002731184168 ) ) ;
#8488 = CARTESIAN_POINT ( 'NONE',  ( 0.000000000000000000, 40.99999999999999289, 0.000000000000000000 ) ) ;
#8489 = CARTESIAN_POINT ( 'NONE',  ( 13.14518615778179544, 39.36289062608393152, -1.609821015232357215E-15 ) ) ;
#8490 = CARTESIAN_POINT ( 'NONE',  ( 101.7677669529663547, 123.0000000021849615, 1.767766952966350891 ) ) ;
#8491 = CIRCLE ( 'NONE', #23083, 13.57481594606304398 ) ;
#8492 = CARTESIAN_POINT ( 'NONE',  ( 63.39746686938465814, 53.60343507248209249, 14.99999999999997868 ) ) ;
#8493 = DIRECTION ( 'NONE',  ( -0.000000000000000000, -0.000000000000000000, -1.000000000000000000 ) ) ;
#8494 = EDGE_LOOP ( 'NONE', ( #5267, #6038 ) ) ;
#8495 = CARTESIAN_POINT ( 'NONE',  ( 96.84719886470459471, -3.152801135295355994, 7.562500001365592084 ) ) ;
#8496 = CARTESIAN_POINT ( 'NONE',  ( 78.49550141231718214, 36.00000000000000711, -0.9550757908087965653 ) ) ;
#8497 = ORIENTED_EDGE ( 'NONE', *, *, #26923, .T. ) ;
#8498 = DIRECTION ( 'NONE',  ( 0.000000000000000000, 0.000000000000000000, 1.000000000000000000 ) ) ;
#8499 = CARTESIAN_POINT ( 'NONE',  ( 98.15313185440925281, -4.458734124999987891, 10.62500000136559208 ) ) ;
#8500 = CARTESIAN_POINT ( 'NONE',  ( 65.00000000000000000, 38.12265625216787157, 13.57481594606304576 ) ) ;
#8501 = CARTESIAN_POINT ( 'NONE',  ( -8.049105076161786076E-16, 40.35507812608393152, -13.14518615778179544 ) ) ;
#8502 = DIRECTION ( 'NONE',  ( 0.000000000000000000, 0.000000000000000000, 1.000000000000000000 ) ) ;
#8503 = CARTESIAN_POINT ( 'NONE',  ( 104.4587341249999781, 80.12500000136560629, 1.846868145590721655 ) ) ;
#8504 = CARTESIAN_POINT ( 'NONE',  ( 78.14518615778179367, 37.97382812608393721, -1.609821015232357215E-15 ) ) ;
#8505 = CARTESIAN_POINT ( 'NONE',  ( 99.99999999999998579, 101.5015231886685854, -52.62500000273118417 ) ) ;
#8506 = CARTESIAN_POINT ( 'NONE',  ( -13.14518615778179544, 39.75976562608393294, 0.000000000000000000 ) ) ;
#8507 = CIRCLE ( 'NONE', #28087, 5.000000000000000000 ) ;
#8508 = EDGE_LOOP ( 'NONE', ( #26743, #1737, #26131, #19562 ) ) ;
#8509 = DIRECTION ( 'NONE',  ( -1.000000000000000000, 0.000000000000000000, 0.000000000000000000 ) ) ;
#8510 = CARTESIAN_POINT ( 'NONE',  ( 104.9999999999999716, -2.071067811865467956, 11.56250000273118594 ) ) ;
#8511 = CARTESIAN_POINT ( 'NONE',  ( 107.0000000000000000, 110.0000000000000000, -51.49999999453763877 ) ) ;
#8512 = CARTESIAN_POINT ( 'NONE',  ( 120.7049497278729575, 32.11992187608393579, 9.295050272127047819 ) ) ;
#8513 = VERTEX_POINT ( 'NONE', #2254 ) ;
#8514 = CYLINDRICAL_SURFACE ( 'NONE', #2213, 13.57481594606304576 ) ;
#8515 = CARTESIAN_POINT ( 'NONE',  ( 2.414731522848535132E-15, 40.15664062608393436, 13.14518615778179544 ) ) ;
#8516 = CARTESIAN_POINT ( 'NONE',  ( 95.54126587499995082, 79.50000000136560629, 1.846868145590724986 ) ) ;
#8517 = CARTESIAN_POINT ( 'NONE',  ( 116.8548138422182205, 37.37851562608393863, 0.000000000000000000 ) ) ;
#8518 = CARTESIAN_POINT ( 'NONE',  ( 55.40115559117954547, 38.61875000216787157, -9.598844408820458085 ) ) ;
#8519 = DIRECTION ( 'NONE',  ( 0.000000000000000000, 0.000000000000000000, 1.000000000000000000 ) ) ;
#8520 = CARTESIAN_POINT ( 'NONE',  ( 2.493653234604083739E-15, 36.53515625216787299, 13.57481594606304576 ) ) ;
#8521 = CARTESIAN_POINT ( 'NONE',  ( 94.99999999999995737, 1.387778780781445676E-14, 5.999999999999998224 ) ) ;
#8522 = CARTESIAN_POINT ( 'NONE',  ( 99.99999999999995737, 5.000000000000018652, 1.749999999999999778 ) ) ;
#8523 = CARTESIAN_POINT ( 'NONE',  ( 200.4449143864723055, 37.13046875108393152, -13.14518615778179900 ) ) ;
#8524 = AXIS2_PLACEMENT_3D ( 'NONE', #19179, #5806, #18896 ) ;
#8525 = VECTOR ( 'NONE', #21398, 1000.000000000000000 ) ;
#8526 = FACE_OUTER_BOUND ( 'NONE', #22463, .T. ) ;
#8527 = CARTESIAN_POINT ( 'NONE',  ( 13.57481594606304753, 34.40195312716787157, -5.622872871577873966 ) ) ;
#8528 = CARTESIAN_POINT ( 'NONE',  ( 98.96446609406726225, 122.5500000021849587, -2.499999999999997780 ) ) ;
#8529 = CARTESIAN_POINT ( 'NONE',  ( 104.9999999999999716, -2.071067811865452857, 10.56250000273118417 ) ) ;
#8530 = CARTESIAN_POINT ( 'NONE',  ( 107.0000000000000142, 112.2744378736303190, -54.90000000000000568 ) ) ;
#8531 = CARTESIAN_POINT ( 'NONE',  ( -13.14518615778179900, 38.32109375108394289, -5.444914386472297529 ) ) ;
#8532 = CARTESIAN_POINT ( 'NONE',  ( 9.295050272127046043, 37.87460937608393152, -9.295050272127046043 ) ) ;
#8533 = CARTESIAN_POINT ( 'NONE',  ( 181.4251840539369596, 38.61874999999999147, 0.000000000000000000 ) ) ;
#8534 = CARTESIAN_POINT ( 'NONE',  ( 59.37712712842205320, 40.05742187499998863, -13.57481594606297293 ) ) ;
#8535 = CARTESIAN_POINT ( 'NONE',  ( 95.54126587499995082, -1.846868145590724986, 1.750000001365591862 ) ) ;
#8536 = CARTESIAN_POINT ( 'NONE',  ( 59.55508561352770158, 38.32109375108394289, 13.14518615778179722 ) ) ;
#8537 = CARTESIAN_POINT ( 'NONE',  ( 95.54126587499996504, 1.387778780781445676E-14, 1.437500001365591196 ) ) ;
#8538 = CARTESIAN_POINT ( 'NONE',  ( 105.6631189606246295, 114.1144967660473242, -45.30000000546237970 ) ) ;
#8539 = CARTESIAN_POINT ( 'NONE',  ( 104.4587341249999923, 93.37499999863439371, -1.846868145590737198 ) ) ;
#8540 = CARTESIAN_POINT ( 'NONE',  ( 55.81982418635200105, 50.00000000000000000, 9.999999999999982236 ) ) ;
#8541 = CARTESIAN_POINT ( 'NONE',  ( -9.598844408820458085, 39.31328124999999574, -9.598844408820458085 ) ) ;
#8542 = CARTESIAN_POINT ( 'NONE',  ( 130.0000000000000000, 39.36289062608393152, 13.14518615778179544 ) ) ;
#8543 = ORIENTED_EDGE ( 'NONE', *, *, #18490, .F. ) ;
#8544 = CARTESIAN_POINT ( 'NONE',  ( 103.5355339059327093, 82.62500000000000000, -3.535533905932755072 ) ) ;
#8545 = CARTESIAN_POINT ( 'NONE',  ( 95.54126587499999346, 92.74999999863439371, -1.846868145590737864 ) ) ;
#8546 = EDGE_LOOP ( 'NONE', ( #12717, #1597, #9060, #7066 ) ) ;
#8547 = CARTESIAN_POINT ( 'NONE',  ( 95.67376207875069838, 115.9545556584642867, -45.30000000000000426 ) ) ;
#8548 = CARTESIAN_POINT ( 'NONE',  ( 70.44491438647230552, 33.36015625108393579, -13.14518615778179900 ) ) ;
#8549 = ORIENTED_EDGE ( 'NONE', *, *, #11558, .T. ) ;
#8550 =( BOUNDED_CURVE ( )  B_SPLINE_CURVE ( 2, ( #22504, #24920, #25064, #24495, #995, #24643, #11644, #9525, #18225 ),
 .UNSPECIFIED., .F., .F. ) 
 B_SPLINE_CURVE_WITH_KNOTS ( ( 3, 2, 2, 2, 3 ),
 ( 0.5625000000000004441, 0.5729166666666669627, 0.5833333333333337034, 0.5937500000000002220, 0.6041666666666668517 ),
 .UNSPECIFIED. ) 
 CURVE ( )  GEOMETRIC_REPRESENTATION_ITEM ( )  RATIONAL_B_SPLINE_CURVE ( ( 0.9999999999999967804, 0.9238795325112899581, 1.000000000000000000, 0.9238795325112867385, 1.000000000000000000, 0.9238795325112867385, 1.000000000000000000, 0.9238795325112850731, 1.000000000000001554 ) ) 
 REPRESENTATION_ITEM ( '' )  );
#8551 = LINE ( 'NONE', #17383, #21293 ) ;
#8552 = CARTESIAN_POINT ( 'NONE',  ( 101.8468681455906903, -4.458734124999987891, 1.000000001365592528 ) ) ;
#8553 = ORIENTED_EDGE ( 'NONE', *, *, #23321, .T. ) ;
#8554 = CARTESIAN_POINT ( 'NONE',  ( -5.444914386472299306, 34.55078125108393294, 13.14518615778179722 ) ) ;
#8555 = CARTESIAN_POINT ( 'NONE',  ( -8.049105076161786076E-16, 39.75976562608394005, -13.14518615778179544 ) ) ;
#8556 = CARTESIAN_POINT ( 'NONE',  ( 195.0000000000000000, 36.13828125216787157, -13.57481594606304576 ) ) ;
#8557 = CARTESIAN_POINT ( 'NONE',  ( -9.295050272127046043, 37.27929687608393294, -9.295050272127046043 ) ) ;
#8558 = CARTESIAN_POINT ( 'NONE',  ( 108.0825317500000153, 110.0000000000000000, -44.12500000273119127 ) ) ;
#8559 = CARTESIAN_POINT ( 'NONE',  ( 195.7238719380222562, 53.51529642094860861, 14.99999999999994671 ) ) ;
#8560 = CARTESIAN_POINT ( 'NONE',  ( 120.7049497278729575, 38.46992187608393721, 9.295050272127047819 ) ) ;
#8561 = VERTEX_POINT ( 'NONE', #19625 ) ;
#8562 = CARTESIAN_POINT ( 'NONE',  ( -5.444914386472297529, 38.22187500108393010, -13.14518615778179900 ) ) ;
#8563 = EDGE_CURVE ( 'NONE', #19876, #12833, #12158, .T. ) ;
#8564 = CARTESIAN_POINT ( 'NONE',  ( 116.8548138422182063, 35.84062500108394289, 5.444914386472304635 ) ) ;
#8565 = CARTESIAN_POINT ( 'NONE',  ( 59.37712712842213136, 38.46992187499999716, -13.57481594606304753 ) ) ;
#8566 = VECTOR ( 'NONE', #19751, 1000.000000000000000 ) ;
#8567 = CARTESIAN_POINT ( 'NONE',  ( 103.1528011352953342, 3.152801135295383084, 14.31250000136559208 ) ) ;
#8568 = DIRECTION ( 'NONE',  ( 1.000000000000000000, 0.000000000000000000, 0.000000000000000000 ) ) ;
#8569 = CARTESIAN_POINT ( 'NONE',  ( 101.8468681455906903, -4.458734124999987891, 4.750000001365592084 ) ) ;
#8570 = CARTESIAN_POINT ( 'NONE',  ( 102.4976396683250925, 102.3130555110000159, -52.52500000273119696 ) ) ;
#8571 = MECHANICAL_DESIGN_GEOMETRIC_PRESENTATION_REPRESENTATION (  '', ( #5458 ), #14919 ) ;
#8572 = CARTESIAN_POINT ( 'NONE',  ( 13.57481594606304931, 39.06523437716786873, 5.622872871577868636 ) ) ;
#8573 = CARTESIAN_POINT ( 'NONE',  ( 98.15313185440923860, 80.87500000136560629, 4.458734124999987891 ) ) ;
#8574 = CARTESIAN_POINT ( 'NONE',  ( 99.99999999999997158, 118.4984768113314146, -46.12499999726881583 ) ) ;
#8575 = CARTESIAN_POINT ( 'NONE',  ( -5.444914386472297529, 39.80937500108392868, -13.14518615778179900 ) ) ;
#8576 = CARTESIAN_POINT ( 'NONE',  ( 106.5389055433250860, 105.2492070361643215, -51.07499999726882578 ) ) ;
#8577 = ORIENTED_EDGE ( 'NONE', *, *, #18586, .F. ) ;
#8578 = CARTESIAN_POINT ( 'NONE',  ( 99.14382582708708469, 124.1000000010924822, 2.066987299999979655 ) ) ;
#8579 = PLANE ( 'NONE',  #2980 ) ;
#8580 = DIRECTION ( 'NONE',  ( 1.000000000000000000, -0.000000000000000000, -7.228014483236696740E-18 ) ) ;
#8581 = DIRECTION ( 'NONE',  ( 0.000000000000000000, -1.000000000000000000, 3.469446951953611231E-16 ) ) ;
#8582 = CARTESIAN_POINT ( 'NONE',  ( 185.7049497278729575, 38.07304687608393579, -9.295050272127046043 ) ) ;
#8583 = ORIENTED_EDGE ( 'NONE', *, *, #27226, .T. ) ;
#8584 = DIRECTION ( 'NONE',  ( -0.000000000000000000, 1.000000000000000000, -0.000000000000000000 ) ) ;
#8585 = FACE_OUTER_BOUND ( 'NONE', #10412, .T. ) ;
#8586 = AXIS2_PLACEMENT_3D ( 'NONE', #7779, #1241, #10458 ) ;
#8587 = CARTESIAN_POINT ( 'NONE',  ( 143.5748159460630688, 39.80937499999999574, -1.662435489736055892E-15 ) ) ;
#8588 = VERTEX_POINT ( 'NONE', #5376 ) ;
#8589 = CARTESIAN_POINT ( 'NONE',  ( 97.83688103937537051, 103.3426043859339103, -51.60000000000000853 ) ) ;
#8590 = CARTESIAN_POINT ( 'NONE',  ( 124.3771271284221314, 37.67617187499999432, -13.57481594606304753 ) ) ;
#8591 = DIRECTION ( 'NONE',  ( 1.000000000000000000, 0.000000000000000000, 0.000000000000000000 ) ) ;
#8592 = CARTESIAN_POINT ( 'NONE',  ( 116.4251840539369596, 31.57421875216786944, 0.000000000000000000 ) ) ;
#8593 = CARTESIAN_POINT ( 'NONE',  ( -5.622872871577965448, 34.00507812499998295, 13.57481594606295161 ) ) ;
#8594 =( BOUNDED_CURVE ( )  B_SPLINE_CURVE ( 2, ( #6803, #19925, #17636, #24631, #4682, #26195, #13198, #408, #2959 ),
 .UNSPECIFIED., .F., .T. ) 
 B_SPLINE_CURVE_WITH_KNOTS ( ( 3, 2, 2, 2, 3 ),
 ( 0.06250000000000004163, 0.07291666666666665741, 0.08333333333333325932, 0.09374999999999987510, 0.1041666666666664909 ),
 .UNSPECIFIED. ) 
 CURVE ( )  GEOMETRIC_REPRESENTATION_ITEM ( )  RATIONAL_B_SPLINE_CURVE ( ( 0.9999999999999996669, 0.9238795325112870716, 1.000000000000000000, 0.9238795325112867385, 1.000000000000000000, 0.9238795325112867385, 1.000000000000000000, 0.9238795325112880708, 0.9999999999999986677 ) ) 
 REPRESENTATION_ITEM ( '' )  );
#8595 = CARTESIAN_POINT ( 'NONE',  ( 51.85481384221819923, 40.70234375108393721, -5.444914386472297529 ) ) ;
#8596 = EDGE_CURVE ( 'NONE', #18417, #8271, #7265, .T. ) ;
#8597 = CARTESIAN_POINT ( 'NONE',  ( -13.57481594606304753, 34.69960937716787441, -5.622872871577872189 ) ) ;
#8598 = CARTESIAN_POINT ( 'NONE',  ( 204.2950502721270425, 34.89804687608393863, -9.295050272127046043 ) ) ;
#8599 = EDGE_LOOP ( 'NONE', ( #13688, #13326 ) ) ;
#8600 = EDGE_CURVE ( 'NONE', #3776, #22871, #25662, .T. ) ;
#8601 = EDGE_LOOP ( 'NONE', ( #4018, #12572, #17379, #9608 ) ) ;
#8602 = CARTESIAN_POINT ( 'NONE',  ( 9.295050272127046043, 38.86679687608393863, -9.295050272127046043 ) ) ;
#8603 = CARTESIAN_POINT ( 'NONE',  ( 104.4587341249999781, -1.846868145590721655, 10.12500000136559386 ) ) ;
#8604 = CARTESIAN_POINT ( 'NONE',  ( 59.55508561352770158, 40.40468750108393436, -13.14518615778179722 ) ) ;
#8605 = CARTESIAN_POINT ( 'NONE',  ( 51.42518405393695957, 36.33671875216787583, 0.000000000000000000 ) ) ;
#8606 = CARTESIAN_POINT ( 'NONE',  ( 204.2950502721270425, 39.26367187608393294, 9.295050272127046043 ) ) ;
#8607 = CARTESIAN_POINT ( 'NONE',  ( -13.14518615778179722, 40.70234375108392300, -5.444914386472297529 ) ) ;
#8608 = CARTESIAN_POINT ( 'NONE',  ( 99.99999999999998579, 90.00000000000000000, 2.999999999999982681 ) ) ;
#8609 = CARTESIAN_POINT ( 'NONE',  ( 94.99999999999995737, -2.071067811865475949, 12.06249999999999822 ) ) ;
#8610 = VECTOR ( 'NONE', #14866, 1000.000000000000000 ) ;
#8611 = FACE_OUTER_BOUND ( 'NONE', #10738, .T. ) ;
#8612 = CARTESIAN_POINT ( 'NONE',  ( 102.4976396683250783, 117.6869444889999841, -54.22499999726881725 ) ) ;
#8613 = EDGE_CURVE ( 'NONE', #17637, #13728, #5456, .T. ) ;
#8614 = VERTEX_POINT ( 'NONE', #24614 ) ;
#8615 = CARTESIAN_POINT ( 'NONE',  ( 9.598844408820459861, 37.32890624999999574, 9.598844408820456309 ) ) ;
#8616 = CARTESIAN_POINT ( 'NONE',  ( -13.14518615778179189, 37.42812500108393436, 5.444914386472304635 ) ) ;
#8617 = CARTESIAN_POINT ( 'NONE',  ( 99.99999999999995737, 5.000000000000018652, 0.8750000027311858330 ) ) ;
#8618 = CARTESIAN_POINT ( 'NONE',  ( 130.0000000000000000, 36.98164062608393721, 13.14518615778179544 ) ) ;
#8619 = CARTESIAN_POINT ( 'NONE',  ( 55.70494972787295751, 32.51679687608393721, -9.295050272127046043 ) ) ;
#8620 = CARTESIAN_POINT ( 'NONE',  ( 195.0000000000000000, 38.56914062608393579, 13.14518615778179544 ) ) ;
#8621 = CARTESIAN_POINT ( 'NONE',  ( 63.97819628124013036, 36.00000000000001421, 13.11239906893439233 ) ) ;
#8622 = CARTESIAN_POINT ( 'NONE',  ( 13.14518615778179544, 33.01289062608393010, -1.609821015232357215E-15 ) ) ;
#8623 = FACE_OUTER_BOUND ( 'NONE', #295, .T. ) ;
#8624 = CARTESIAN_POINT ( 'NONE',  ( 190.6259778691825204, 36.00000000000002132, 12.40367315690597749 ) ) ;
#8625 = ADVANCED_FACE ( 'NONE', ( #3094, #5092, #6929, #7350, #13754 ), #22193, .F. ) ;
#8626 = CARTESIAN_POINT ( 'NONE',  ( 13.14518615778179544, 33.21132812608393436, -1.609821015232357215E-15 ) ) ;
#8627 = CARTESIAN_POINT ( 'NONE',  ( 99.99999999999998579, 118.4984768113314146, -51.62500000273119127 ) ) ;
#8628 = CARTESIAN_POINT ( 'NONE',  ( -9.295050272127046043, 34.10429687608393579, -9.295050272127046043 ) ) ;
#8629 =( BOUNDED_CURVE ( )  B_SPLINE_CURVE ( 2, ( #10647, #14510, #19353, #28056, #8522, #17208, #1707, #19076, #25913 ),
 .UNSPECIFIED., .F., .T. ) 
 B_SPLINE_CURVE_WITH_KNOTS ( ( 3, 2, 2, 2, 3 ),
 ( 0.9285714285714284921, 0.9374999999999998890, 0.9464285714285712858, 0.9553571428571427937, 0.9642857142857141906 ),
 .UNSPECIFIED. ) 
 CURVE ( )  GEOMETRIC_REPRESENTATION_ITEM ( )  RATIONAL_B_SPLINE_CURVE ( ( 1.000000000000000888, 0.9238795325112857393, 1.000000000000000000, 0.9238795325112867385, 1.000000000000000000, 0.9238795325112867385, 1.000000000000000000, 0.9238795325112877377, 0.9999999999999990008 ) ) 
 REPRESENTATION_ITEM ( '' )  );
#8630 = DIRECTION ( 'NONE',  ( 0.000000000000000000, -1.000000000000000000, 0.000000000000000000 ) ) ;
#8631 = CARTESIAN_POINT ( 'NONE',  ( 103.5355339059327093, 79.75000000273119838, -3.535533905932755072 ) ) ;
#8632 = AXIS2_PLACEMENT_3D ( 'NONE', #16262, #17979, #27258 ) ;
#8633 = ADVANCED_FACE ( 'NONE', ( #11614 ), #11334, .F. ) ;
#8634 = CARTESIAN_POINT ( 'NONE',  ( 97.50000000000000000, 124.1499999999999915, -1.035533905932742416 ) ) ;
#8635 = CARTESIAN_POINT ( 'NONE',  ( 0.000000000000000000, 0.000000000000000000, 0.000000000000000000 ) ) ;
#8636 = CARTESIAN_POINT ( 'NONE',  ( 99.99999999999995737, -4.458734124999988779, 8.687500001365592084 ) ) ;
#8637 = VERTEX_POINT ( 'NONE', #9216 ) ;
#8638 = CARTESIAN_POINT ( 'NONE',  ( 98.96446609406727646, 122.8500000021849416, 2.499999999999977796 ) ) ;
#8639 = CARTESIAN_POINT ( 'NONE',  ( 98.15313185440925281, 4.458734125000016313, 12.25000000136559208 ) ) ;
#8640 = CARTESIAN_POINT ( 'NONE',  ( 59.37712712842203189, 37.77539062716787299, -13.57481594606295339 ) ) ;
#8641 = EDGE_CURVE ( 'NONE', #6724, #19008, #16189, .T. ) ;
#8642 = VECTOR ( 'NONE', #13282, 1000.000000000000000 ) ;
#8643 = CARTESIAN_POINT ( 'NONE',  ( 3.878385410779738418, 31.34156310770110565, -13.57481594606304931 ) ) ;
#8644 = CARTESIAN_POINT ( 'NONE',  ( -8.312177448680279460E-16, 36.93203125216787441, -13.57481594606304576 ) ) ;
#8645 = CARTESIAN_POINT ( 'NONE',  ( 104.4587341249999781, 83.25000000136560629, -1.846868145590750299 ) ) ;
#8646 = CARTESIAN_POINT ( 'NONE',  ( 65.00000000000000000, 36.58476562608393579, -13.14518615778179544 ) ) ;
#8647 = CARTESIAN_POINT ( 'NONE',  ( 104.9952793366501851, 116.8754121666685393, -49.82500000273120122 ) ) ;
#8648 = CARTESIAN_POINT ( 'NONE',  ( -13.14518615778179544, 40.55351562608393579, 0.000000000000000000 ) ) ;
#8649 = ORIENTED_EDGE ( 'NONE', *, *, #13672, .F. ) ;
#8650 = CARTESIAN_POINT ( 'NONE',  ( 103.5355339059327093, 80.75000000273119838, -3.535533905932755072 ) ) ;
#8651 = CARTESIAN_POINT ( 'NONE',  ( 139.2950502721270425, 32.31835937608393294, 9.295050272127046043 ) ) ;
#8652 = VERTEX_POINT ( 'NONE', #26620 ) ;
#8653 = CARTESIAN_POINT ( 'NONE',  ( -8.049105076161786076E-16, 38.17226562608394147, -13.14518615778179544 ) ) ;
#8654 = CARTESIAN_POINT ( 'NONE',  ( 5.622872871577878406, 37.37851562716787157, 13.57481594606304576 ) ) ;
#8655 = CARTESIAN_POINT ( 'NONE',  ( 116.8548138422182063, 38.12265625108393152, -5.444914386472297529 ) ) ;
#8656 = CARTESIAN_POINT ( 'NONE',  ( 51.42518405393695957, 32.41757812716787157, 5.622872871577880183 ) ) ;
#8657 = AXIS2_PLACEMENT_3D ( 'NONE', #20894, #1377, #25028 ) ;
#8658 = CARTESIAN_POINT ( 'NONE',  ( 12.25119088044477600, 35.99999999999998579, 5.405483146087242119 ) ) ;
#8659 = CARTESIAN_POINT ( 'NONE',  ( -13.57481594606304753, 34.69960937716787441, -5.622872871577873077 ) ) ;
#8660 = CARTESIAN_POINT ( 'NONE',  ( 103.5355339059327093, 3.535533905932755072, 4.624999999999999112 ) ) ;
#8661 = CARTESIAN_POINT ( 'NONE',  ( 91.91746824999998466, 110.0000000000000000, -47.87499999726882294 ) ) ;
#8662 = VECTOR ( 'NONE', #23751, 1000.000000000000000 ) ;
#8663 = CARTESIAN_POINT ( 'NONE',  ( 185.7049497278729575, 39.06523437608392868, 9.295050272127047819 ) ) ;
#8664 = CARTESIAN_POINT ( 'NONE',  ( 74.59884440882045453, 38.91640624999999432, 9.598844408820456309 ) ) ;
#8665 = CARTESIAN_POINT ( 'NONE',  ( 139.2950502721270425, 36.28710937608393294, -9.295050272127046043 ) ) ;
#8666 = CARTESIAN_POINT ( 'NONE',  ( 65.00000000000000000, -7.395377635281828788, -13.57481594606305109 ) ) ;
#8667 = CARTESIAN_POINT ( 'NONE',  ( 0.000000000000000000, 10.00000000000000178, 0.000000000000000000 ) ) ;
#8668 = CARTESIAN_POINT ( 'NONE',  ( 129.1578924045353460, 53.50112910130382460, 14.99999999999996803 ) ) ;
#8669 = CARTESIAN_POINT ( 'NONE',  ( 13.57481594606304931, 35.79101562499999289, 5.622872871577869525 ) ) ;
#8670 = CARTESIAN_POINT ( 'NONE',  ( 91.00000000000000000, 110.0000000000000000, -55.00000000000000711 ) ) ;
#8671 = CARTESIAN_POINT ( 'NONE',  ( -13.14518615778179544, 35.98945312608393721, 0.000000000000000000 ) ) ;
#8672 = CARTESIAN_POINT ( 'NONE',  ( -9.295050272127046043, 40.45429687608393721, -9.295050272127046043 ) ) ;
#8673 = CARTESIAN_POINT ( 'NONE',  ( 200.6228728715778686, 33.31054687499999289, 13.57481594606304576 ) ) ;
#8674 = EDGE_CURVE ( 'NONE', #18802, #27424, #18193, .T. ) ;
#8675 = CARTESIAN_POINT ( 'NONE',  ( 108.0825317500000011, 107.3738262389971680, -46.47500000273118559 ) ) ;
#8676 = CARTESIAN_POINT ( 'NONE',  ( 99.99999999999995737, 85.00000000000000000, 4.999999999999990230 ) ) ;
#8677 = CARTESIAN_POINT ( 'NONE',  ( 59.55508561352770158, 36.73359375108393010, 13.14518615778179722 ) ) ;
#8678 = AXIS2_PLACEMENT_3D ( 'NONE', #2311, #2021, #10968 ) ;
#8679 = CARTESIAN_POINT ( 'NONE',  ( 95.54126587499996504, 1.387778780781445676E-14, 0.4375000013655920839 ) ) ;
#8680 = CARTESIAN_POINT ( 'NONE',  ( 2.493653234604083739E-15, 35.74140625216787015, 13.57481594606304576 ) ) ;
#8681 = CARTESIAN_POINT ( 'NONE',  ( 98.15313185440925281, 92.62499999863439371, -4.458734124999994997 ) ) ;
#8682 = LINE ( 'NONE', #21946, #3460 ) ;
#8683 = CARTESIAN_POINT ( 'NONE',  ( 9.598844408820459861, 36.53515624999999289, 9.598844408820456309 ) ) ;
#8684 = CARTESIAN_POINT ( 'NONE',  ( 104.3262379212492590, 104.0454443415356991, -45.29999999999999716 ) ) ;
#8685 = ORIENTED_EDGE ( 'NONE', *, *, #21200, .F. ) ;
#8686 = CARTESIAN_POINT ( 'NONE',  ( 102.0710678118654329, 83.68750000000001421, -5.000000000000018652 ) ) ;
#8687 = AXIS2_PLACEMENT_3D ( 'NONE', #21022, #1503, #3492 ) ;
#8688 = CARTESIAN_POINT ( 'NONE',  ( 98.15313185440925281, 93.99999999863439371, 4.458734124999979898 ) ) ;
#8689 = EDGE_LOOP ( 'NONE', ( #15677, #4344, #2510, #5590 ) ) ;
#8690 = CARTESIAN_POINT ( 'NONE',  ( 94.33688103937535629, 105.8855032339526758, -50.80000000000001137 ) ) ;
#8691 = CARTESIAN_POINT ( 'NONE',  ( 65.00000000000000000, 33.40976562608393863, -13.14518615778179544 ) ) ;
#8692 = ORIENTED_EDGE ( 'NONE', *, *, #10691, .F. ) ;
#8693 = CARTESIAN_POINT ( 'NONE',  ( 121.6077847083616206, 54.99999999999998579, -15.00000000000000178 ) ) ;
#8694 = CARTESIAN_POINT ( 'NONE',  ( 104.4587341249999639, 1.442382525525748735E-14, 2.187500001365592084 ) ) ;
#8695 = ORIENTED_EDGE ( 'NONE', *, *, #23457, .F. ) ;
#8696 = CARTESIAN_POINT ( 'NONE',  ( 5.444914386472297529, 34.15390625108393863, -13.14518615778179722 ) ) ;
#8697 = CARTESIAN_POINT ( 'NONE',  ( -13.14518615778179900, 39.11484375108394573, -5.444914386472297529 ) ) ;
#8698 = CARTESIAN_POINT ( 'NONE',  ( 208.5748159460630120, 38.37070312716786447, -5.622872871577873077 ) ) ;
#8699 = CARTESIAN_POINT ( 'NONE',  ( 2.414731522848535132E-15, 35.19570312608392726, 13.14518615778179544 ) ) ;
#8700 = CARTESIAN_POINT ( 'NONE',  ( 99.99999999999995737, 1.387778780781445676E-14, 34.79898987322334136 ) ) ;
#8701 = CARTESIAN_POINT ( 'NONE',  ( 196.8143553545835402, 51.46618445021835697, 15.00000000000029843 ) ) ;
#8702 = ORIENTED_EDGE ( 'NONE', *, *, #3595, .F. ) ;
#8703 = CARTESIAN_POINT ( 'NONE',  ( -9.295050272127046043, 37.47773437608393010, -9.295050272127046043 ) ) ;
#8704 = CARTESIAN_POINT ( 'NONE',  ( 130.0000000000000000, 35.19570312608392726, 13.14518615778179544 ) ) ;
#8705 = CARTESIAN_POINT ( 'NONE',  ( 65.00000000000000000, 34.45156249999999432, -13.57481594606304576 ) ) ;
#8706 = CARTESIAN_POINT ( 'NONE',  ( 99.99999999999995737, 5.000000000000018652, 9.749999999999998224 ) ) ;
#8707 = CARTESIAN_POINT ( 'NONE',  ( 103.1528011352953342, 3.152801135295383084, 9.312500001365593860 ) ) ;
#8708 = CARTESIAN_POINT ( 'NONE',  ( 94.99999999999995737, 84.06250000273119838, -2.071067811865491493 ) ) ;
#8709 = CARTESIAN_POINT ( 'NONE',  ( 104.4587341249999639, 1.442382525525748735E-14, 13.93750000136559208 ) ) ;
#8710 = CARTESIAN_POINT ( 'NONE',  ( 99.99999999999998579, 118.4984768113314004, -49.62500000273118417 ) ) ;
#8711 = CARTESIAN_POINT ( 'NONE',  ( 99.99999999999998579, 110.0000000000000000, -145.0000000000000284 ) ) ;
#8712 = LINE ( 'NONE', #25821, #24428 ) ;
#8713 = CARTESIAN_POINT ( 'NONE',  ( 95.00472066334981491, 103.1245878333314465, -49.32499999726881867 ) ) ;
#8714 = CARTESIAN_POINT ( 'NONE',  ( 5.444914386472302859, 37.03125000108393294, 13.14518615778179189 ) ) ;
#8715 = CARTESIAN_POINT ( 'NONE',  ( 130.0000000000000000, 50.00000000000000000, 13.57481594606302799 ) ) ;
#8716 = ORIENTED_EDGE ( 'NONE', *, *, #5209, .F. ) ;
#8717 = CARTESIAN_POINT ( 'NONE',  ( 94.99999999999995737, 1.387778780781445676E-14, 34.79898987322334136 ) ) ;
#8718 =( BOUNDED_CURVE ( )  B_SPLINE_CURVE ( 2, ( #27921, #23642, #12643, #25916, #8382, #19498, #10512, #25770, #4117 ),
 .UNSPECIFIED., .F., .F. ) 
 B_SPLINE_CURVE_WITH_KNOTS ( ( 3, 2, 2, 2, 3 ),
 ( 0.2291666666666665741, 0.2395833333333332316, 0.2499999999999998335, 0.2604166666666665186, 0.2708333333333330928 ),
 .UNSPECIFIED. ) 
 CURVE ( )  GEOMETRIC_REPRESENTATION_ITEM ( )  RATIONAL_B_SPLINE_CURVE ( ( 1.000000000000000666, 0.9238795325112861834, 1.000000000000000000, 0.9238795325112867385, 1.000000000000000000, 0.9238795325112867385, 1.000000000000000000, 0.9238795325112884038, 0.9999999999999983347 ) ) 
 REPRESENTATION_ITEM ( '' )  );
#8719 = CARTESIAN_POINT ( 'NONE',  ( 120.4011555911795455, 37.03125000216787299, -9.598844408820458085 ) ) ;
#8720 = CARTESIAN_POINT ( 'NONE',  ( 99.20899822134843760, 123.0000000000000000, -1.909647267044714436 ) ) ;
#8721 = ADVANCED_FACE ( 'NONE', ( #11761 ), #26903, .T. ) ;
#8722 = CARTESIAN_POINT ( 'NONE',  ( 189.5550856135277229, 38.02343750108394005, -13.14518615778179900 ) ) ;
#8723 = VERTEX_POINT ( 'NONE', #22623 ) ;
#8724 = CARTESIAN_POINT ( 'NONE',  ( 78.14518615778179367, 36.38632812608393863, -1.609821015232357215E-15 ) ) ;
#8725 = DIRECTION ( 'NONE',  ( -1.000000000000000000, 0.000000000000000000, 0.000000000000000000 ) ) ;
#8726 = CARTESIAN_POINT ( 'NONE',  ( 95.54126587499996504, 1.387778780781445676E-14, 13.68750000136559386 ) ) ;
#8727 = ORIENTED_EDGE ( 'NONE', *, *, #12749, .F. ) ;
#8728 = CARTESIAN_POINT ( 'NONE',  ( 93.00000000000001421, 112.2744378736303332, -52.10000000000000853 ) ) ;
#8729 = CARTESIAN_POINT ( 'NONE',  ( 5.622872871577780707, 33.70742187716788152, -13.57481594606313990 ) ) ;
#8730 = CARTESIAN_POINT ( 'NONE',  ( 102.0710678118654329, 93.06249999726880162, -5.000000000000023093 ) ) ;
#8731 = CARTESIAN_POINT ( 'NONE',  ( 139.2950502721270425, 39.26367187608393294, 9.295050272127046043 ) ) ;
#8732 = DIRECTION ( 'NONE',  ( -0.000000000000000000, -0.000000000000000000, -1.000000000000000000 ) ) ;
#8733 = CARTESIAN_POINT ( 'NONE',  ( 103.5355339059327235, 94.74999999726881583, 3.535533905932724874 ) ) ;
#8734 = CARTESIAN_POINT ( 'NONE',  ( 74.29505027212704249, 39.46210937608393721, 9.295050272127046043 ) ) ;
#8735 = LINE ( 'NONE', #15275, #4600 ) ;
#8736 = CARTESIAN_POINT ( 'NONE',  ( 185.7049497278729575, 35.29492187608393294, 9.295050272127047819 ) ) ;
#8737 = ORIENTED_EDGE ( 'NONE', *, *, #22715, .F. ) ;
#8738 = EDGE_LOOP ( 'NONE', ( #25846, #26458, #7064, #17039 ) ) ;
#8739 = ORIENTED_EDGE ( 'NONE', *, *, #6071, .F. ) ;
#8740 = CARTESIAN_POINT ( 'NONE',  ( -9.295050272127044266, 38.46992187608393721, 9.295050272127047819 ) ) ;
#8741 = FILL_AREA_STYLE_COLOUR ( '', #26386 ) ;
#8742 = CARTESIAN_POINT ( 'NONE',  ( 103.1528011352953342, 3.152801135295383084, 12.31250000136559208 ) ) ;
#8743 = CARTESIAN_POINT ( 'NONE',  ( 103.5355339059327235, 91.12500000000000000, -3.535533905932738197 ) ) ;
#8744 = PRODUCT_DEFINITION_SHAPE ( 'NONE', 'NONE',  #22512 ) ;
#8745 = CARTESIAN_POINT ( 'NONE',  ( 98.15313185440923860, 82.62500000136560629, 4.458734124999987891 ) ) ;
#8746 = CARTESIAN_POINT ( 'NONE',  ( 185.7049497278729575, 39.06523437608392868, 9.295050272127047819 ) ) ;
#8747 = CARTESIAN_POINT ( 'NONE',  ( 2.414731522848535132E-15, 37.77539062608393294, 13.14518615778179544 ) ) ;
#8748 = CARTESIAN_POINT ( 'NONE',  ( 188.8822400544688378, 54.65941425414899157, 14.99999999999995026 ) ) ;
#8749 = FACE_OUTER_BOUND ( 'NONE', #18558, .T. ) ;
#8750 = CARTESIAN_POINT ( 'NONE',  ( 181.8548138422182205, 40.75195312608393294, 0.000000000000000000 ) ) ;
#8751 = CARTESIAN_POINT ( 'NONE',  ( 108.0825317499999869, 107.3738262389971538, -50.72499999726881015 ) ) ;
#8752 = VERTEX_POINT ( 'NONE', #27325 ) ;
#8753 = CARTESIAN_POINT ( 'NONE',  ( 5.622872871577878406, 36.48554687499999716, 13.57481594606304576 ) ) ;
#8754 = CARTESIAN_POINT ( 'NONE',  ( 13.14518615778179900, 37.82500000108392868, -5.444914386472297529 ) ) ;
#8755 = CARTESIAN_POINT ( 'NONE',  ( 104.9999999999999716, 1.449011120738813565E-14, 3.625000002731184612 ) ) ;
#8756 = CARTESIAN_POINT ( 'NONE',  ( 139.2950502721270425, 35.49335937608393721, 9.295050272127046043 ) ) ;
#8757 = CARTESIAN_POINT ( 'NONE',  ( 70.44491438647230552, 33.16171875108393152, -13.14518615778179900 ) ) ;
#8758 = AXIS2_PLACEMENT_3D ( 'NONE', #5983, #3985, #25369 ) ;
#8759 = CARTESIAN_POINT ( 'NONE',  ( 208.1451861577817795, 38.02343750108395426, -5.444914386472297529 ) ) ;
#8760 = EDGE_CURVE ( 'NONE', #13376, #21990, #9268, .T. ) ;
#8761 =( BOUNDED_CURVE ( )  B_SPLINE_CURVE ( 1, ( #26035, #28043 ),
 .UNSPECIFIED., .F., .F. ) 
 B_SPLINE_CURVE_WITH_KNOTS ( ( 2, 2 ),
 ( 0.000000000000000000, 1.000000000000000000 ),
 .UNSPECIFIED. ) 
 CURVE ( )  GEOMETRIC_REPRESENTATION_ITEM ( )  RATIONAL_B_SPLINE_CURVE ( ( 0.9684275895297407288, 0.9684275895297407288 ) ) 
 REPRESENTATION_ITEM ( '' )  );
#8762 = FACE_BOUND ( 'NONE', #20039, .T. ) ;
#8763 = CARTESIAN_POINT ( 'NONE',  ( -13.14518615778179189, 31.87187500108393223, 5.444914386472304635 ) ) ;
#8764 = CYLINDRICAL_SURFACE ( 'NONE', #6751, 5.000000000000004441 ) ;
#8765 = CYLINDRICAL_SURFACE ( 'NONE', #5762, 13.57481594606304576 ) ;
#8766 = CARTESIAN_POINT ( 'NONE',  ( 91.91746824999998466, 112.6261737610028320, -51.22500000273119980 ) ) ;
#8767 = CARTESIAN_POINT ( 'NONE',  ( -5.444914386472299306, 35.93984375108392726, 13.14518615778179722 ) ) ;
#8768 = DIRECTION ( 'NONE',  ( -0.000000000000000000, -1.000000000000000000, -0.000000000000000000 ) ) ;
#8769 = CARTESIAN_POINT ( 'NONE',  ( 97.50000000000000000, 123.4500000021849502, -1.035533905932742416 ) ) ;
#8770 = CARTESIAN_POINT ( 'NONE',  ( -9.598844408820454532, 36.43593750216787441, 9.598844408820459861 ) ) ;
#8771 = CARTESIAN_POINT ( 'NONE',  ( 65.00000000000000000, -7.395377635281828788, 13.57481594606303688 ) ) ;
#8772 = CARTESIAN_POINT ( 'NONE',  ( 99.99999999999995737, 4.458734125000016313, 7.187500001365592084 ) ) ;
#8773 = ORIENTED_EDGE ( 'NONE', *, *, #4109, .T. ) ;
#8774 = CARTESIAN_POINT ( 'NONE',  ( 101.7677669529663547, 123.2000000021849502, -1.767766952966370209 ) ) ;
#8775 = CARTESIAN_POINT ( 'NONE',  ( 99.99999999999995737, -4.458734124999988779, 10.68750000136559208 ) ) ;
#8776 = CARTESIAN_POINT ( 'NONE',  ( 55.40115559117954547, 38.02343750216788010, 9.598844408820459861 ) ) ;
#8777 = AXIS2_PLACEMENT_3D ( 'NONE', #24611, #2805, #5373 ) ;
#8778 = CARTESIAN_POINT ( 'NONE',  ( -9.295050272127046043, 38.07304687608393579, -9.295050272127046043 ) ) ;
#8779 = DIRECTION ( 'NONE',  ( 0.000000000000000000, 1.000000000000000000, 0.000000000000000000 ) ) ;
#8780 = CARTESIAN_POINT ( 'NONE',  ( 99.99999999999995737, 82.43750000136559208, -4.458734125000016313 ) ) ;
#8781 = CARTESIAN_POINT ( 'NONE',  ( 55.70494972787295751, 35.89023437608393152, -9.295050272127046043 ) ) ;
#8782 = EDGE_CURVE ( 'NONE', #9247, #28082, #20901, .T. ) ;
#8783 = CARTESIAN_POINT ( 'NONE',  ( 102.4976396683250925, 117.6869444889999841, -49.72500000273119269 ) ) ;
#8784 = CARTESIAN_POINT ( 'NONE',  ( -9.295050272127046043, 36.48554687608393721, -9.295050272127046043 ) ) ;
#8785 = DIRECTION ( 'NONE',  ( 0.000000000000000000, 0.000000000000000000, -1.000000000000000000 ) ) ;
#8786 = CARTESIAN_POINT ( 'NONE',  ( 124.3771271284221029, 36.38632812499999858, 13.57481594606300135 ) ) ;
#8787 = CARTESIAN_POINT ( 'NONE',  ( 107.0000000000000000, 110.0000000000000000, -50.00000000000000711 ) ) ;
#8788 = CARTESIAN_POINT ( 'NONE',  ( 143.5748159460630404, 36.58476562499999574, 5.622872871577869525 ) ) ;
#8789 = ORIENTED_EDGE ( 'NONE', *, *, #7373, .F. ) ;
#8790 = CARTESIAN_POINT ( 'NONE',  ( -5.444914386472297529, 37.42812500108394147, -13.14518615778179900 ) ) ;
#8791 = CARTESIAN_POINT ( 'NONE',  ( -13.57481594606304753, 37.87460937716787868, -5.622872871577873077 ) ) ;
#8792 = CARTESIAN_POINT ( 'NONE',  ( 139.2950502721270425, 37.67617187608393436, 9.295050272127046043 ) ) ;
#8793 = EDGE_CURVE ( 'NONE', #26308, #19984, #17079, .T. ) ;
#8794 = CARTESIAN_POINT ( 'NONE',  ( 65.00000000000000000, 32.96328125216787441, -13.57481594606304576 ) ) ;
#8795 = CARTESIAN_POINT ( 'NONE',  ( 102.0710678118654329, 83.68750000000002842, -5.000000000000004441 ) ) ;
#8796 = CARTESIAN_POINT ( 'NONE',  ( -5.622872871577873077, 32.51679687716787726, 13.57481594606304753 ) ) ;
#8797 =( BOUNDED_CURVE ( )  B_SPLINE_CURVE ( 2, ( #20953, #9963, #18675, #3150, #11958, #27376, #11817, #20680, #9829 ),
 .UNSPECIFIED., .F., .F. ) 
 B_SPLINE_CURVE_WITH_KNOTS ( ( 3, 2, 2, 2, 3 ),
 ( 0.9285714285714284921, 0.9374999999999998890, 0.9464285714285712858, 0.9553571428571427937, 0.9642857142857141906 ),
 .UNSPECIFIED. ) 
 CURVE ( )  GEOMETRIC_REPRESENTATION_ITEM ( )  RATIONAL_B_SPLINE_CURVE ( ( 1.000000000000000888, 0.9238795325112857393, 1.000000000000000000, 0.9238795325112867385, 1.000000000000000000, 0.9238795325112867385, 1.000000000000000000, 0.9238795325112877377, 0.9999999999999990008 ) ) 
 REPRESENTATION_ITEM ( '' )  );
#8798 = EDGE_CURVE ( 'NONE', #10978, #12157, #369, .T. ) ;
#8799 = CARTESIAN_POINT ( 'NONE',  ( 96.46446609406721961, -3.535533905932727539, 5.124999999999999112 ) ) ;
#8800 = CARTESIAN_POINT ( 'NONE',  ( 99.99999999999998579, 97.00000000000000000, -6.938893903907228378E-15 ) ) ;
#8801 = CARTESIAN_POINT ( 'NONE',  ( 208.1451861577818079, 33.80664062608393294, -1.609821015232357215E-15 ) ) ;
#8802 = CARTESIAN_POINT ( 'NONE',  ( -9.598844408820454532, 34.05468750216788010, 9.598844408820459861 ) ) ;
#8803 = EDGE_CURVE ( 'NONE', #4431, #20608, #8344, .T. ) ;
#8804 = CARTESIAN_POINT ( 'NONE',  ( 135.4449143864723339, 36.33671875108393579, -13.14518615778179722 ) ) ;
#8805 = ORIENTED_EDGE ( 'NONE', *, *, #5209, .T. ) ;
#8806 = DIRECTION ( 'NONE',  ( -5.782411586589357392E-17, 0.000000000000000000, -1.000000000000000000 ) ) ;
#8807 = CARTESIAN_POINT ( 'NONE',  ( 99.99999999999995737, 85.00000000000000000, 4.999999999999990230 ) ) ;
#8808 = DIRECTION ( 'NONE',  ( 0.000000000000000000, 1.000000000000000000, 0.000000000000000000 ) ) ;
#8809 = CARTESIAN_POINT ( 'NONE',  ( 2.493653234604083739E-15, 37.22968749999999716, 13.57481594606304576 ) ) ;
#8810 = DIRECTION ( 'NONE',  ( -1.000000000000000000, -1.040834085586055858E-15, 7.228014483236695200E-18 ) ) ;
#8811 = CARTESIAN_POINT ( 'NONE',  ( 13.14518615778179544, 36.38632812608393863, -1.609821015232357215E-15 ) ) ;
#8812 = CARTESIAN_POINT ( 'NONE',  ( 13.14518615778179544, 37.77539062608393294, -1.609821015232357215E-15 ) ) ;
#8813 = CARTESIAN_POINT ( 'NONE',  ( 200.6228728715778686, 34.40195312499999858, -13.57481594606304753 ) ) ;
#8814 = CONTEXT_DEPENDENT_SHAPE_REPRESENTATION ( #23733, #23076 ) ;
#8815 = CARTESIAN_POINT ( 'NONE',  ( 55.40115559117954547, 40.30546874999999574, 9.598844408820459861 ) ) ;
#8816 = CYLINDRICAL_SURFACE ( 'NONE', #24251, 13.57481594606304576 ) ;
#8817 = CARTESIAN_POINT ( 'NONE',  ( 74.29505027212704249, 34.69960937608393436, -9.295050272127046043 ) ) ;
#8818 = CARTESIAN_POINT ( 'NONE',  ( 101.8468681455907046, -4.458734124999987891, 2.750000001365592528 ) ) ;
#8819 = CARTESIAN_POINT ( 'NONE',  ( 105.6631189606246295, 105.8855032339526758, -43.70000000546238539 ) ) ;
#8820 = CARTESIAN_POINT ( 'NONE',  ( 99.99999999999998579, 95.06249999863440792, 4.458734124999981674 ) ) ;
#8821 = CARTESIAN_POINT ( 'NONE',  ( 97.93315853025627860, 123.0000000000000000, 0.2729566057089571340 ) ) ;
#8822 = CARTESIAN_POINT ( 'NONE',  ( 5.622872871577878406, 37.27929687499999289, 13.57481594606304576 ) ) ;
#8823 = CARTESIAN_POINT ( 'NONE',  ( 120.7049497278729575, 37.47773437608393010, -9.295050272127046043 ) ) ;
#8824 = ORIENTED_EDGE ( 'NONE', *, *, #15132, .T. ) ;
#8825 = ORIENTED_EDGE ( 'NONE', *, *, #956, .F. ) ;
#8826 = CARTESIAN_POINT ( 'NONE',  ( 95.54126587499995082, 80.75000000136560629, 1.846868145590724986 ) ) ;
#8827 = CARTESIAN_POINT ( 'NONE',  ( 99.99999999999995737, 82.87500000273119838, -5.000000000000018652 ) ) ;
#8828 = CARTESIAN_POINT ( 'NONE',  ( 96.84719886470463734, 93.93749999863440792, 3.152801135295351997 ) ) ;
#8829 = CARTESIAN_POINT ( 'NONE',  ( 55.16061839111207377, 36.00000000000002132, -9.004033604613061570 ) ) ;
#8830 = ORIENTED_EDGE ( 'NONE', *, *, #12437, .T. ) ;
#8831 = CARTESIAN_POINT ( 'NONE',  ( 97.83688103937537051, 103.3426043859339103, -52.60000000000001563 ) ) ;
#8832 = CARTESIAN_POINT ( 'NONE',  ( 78.14518615778179367, 33.95546875108393436, 5.444914386472293977 ) ) ;
#8833 = VERTEX_POINT ( 'NONE', #11899 ) ;
#8834 = CARTESIAN_POINT ( 'NONE',  ( 1.662435489736055892E-15, 40.99999999999999289, 13.57481594606304576 ) ) ;
#8835 = ADVANCED_FACE ( 'NONE', ( #20622, #1108 ), #9775, .T. ) ;
#8836 = CARTESIAN_POINT ( 'NONE',  ( 99.99999999999995737, -4.458734124999988779, 3.937500001365591640 ) ) ;
#8837 = EDGE_LOOP ( 'NONE', ( #10448, #25551, #7286, #8577 ) ) ;
#8838 = CARTESIAN_POINT ( 'NONE',  ( 5.444914386472297529, 35.74140625108393721, -13.14518615778179722 ) ) ;
#8839 = CARTESIAN_POINT ( 'NONE',  ( -5.444914386472299306, 38.51953125108393294, 13.14518615778179722 ) ) ;
#8840 = CARTESIAN_POINT ( 'NONE',  ( 195.0000000000000000, 34.94765625216787441, 13.57481594606304576 ) ) ;
#8841 = CARTESIAN_POINT ( 'NONE',  ( 9.295050272127046043, 35.49335937608393010, -9.295050272127046043 ) ) ;
#8842 = CARTESIAN_POINT ( 'NONE',  ( 104.9952793366501709, 103.1245878333314465, -44.42500000273119554 ) ) ;
#8843 = CARTESIAN_POINT ( 'NONE',  ( 84.99999999999998579, 102.0000000000000142, -13.00000000000000533 ) ) ;
#8844 = EDGE_LOOP ( 'NONE', ( #6752, #1772, #10137, #21728 ) ) ;
#8845 = CARTESIAN_POINT ( 'NONE',  ( 5.444914386472297529, 37.32890625108393579, -13.14518615778179900 ) ) ;
#8846 = CARTESIAN_POINT ( 'NONE',  ( 143.1451861577818079, 35.34453125108392868, 5.444914386472293977 ) ) ;
#8847 = CARTESIAN_POINT ( 'NONE',  ( 78.57481594606304043, 33.50898437499999716, -5.622872871577873077 ) ) ;
#8848 = CARTESIAN_POINT ( 'NONE',  ( 59.37712712842205320, 39.36289062716787157, -13.57481594606297293 ) ) ;
#8849 = CARTESIAN_POINT ( 'NONE',  ( 104.4587341249999639, 1.442382525525748735E-14, 12.18750000136559208 ) ) ;
#8850 = CARTESIAN_POINT ( 'NONE',  ( 185.8198241863519797, 50.00000000000000000, 9.999999999999952038 ) ) ;
#8851 = AXIS2_PLACEMENT_3D ( 'NONE', #16118, #11836, #24687 ) ;
#8852 = CARTESIAN_POINT ( 'NONE',  ( 95.54126587499996504, 1.387778780781445676E-14, 0.4375000013655920839 ) ) ;
#8853 = CARTESIAN_POINT ( 'NONE',  ( 106.5389055433251002, 105.2492070361643215, -50.32500000273120122 ) ) ;
#8854 = FACE_OUTER_BOUND ( 'NONE', #11940, .T. ) ;
#8855 = LINE ( 'NONE', #2029, #4418 ) ;
#8856 = CARTESIAN_POINT ( 'NONE',  ( 108.0825317499999869, 112.6261737610028320, -52.52499999726882152 ) ) ;
#8857 = CARTESIAN_POINT ( 'NONE',  ( -5.444914386472299306, 37.72578125108395142, 13.14518615778179722 ) ) ;
#8858 = CARTESIAN_POINT ( 'NONE',  ( 106.5389055433250860, 114.7507929638356785, -48.67499999726882010 ) ) ;
#8859 = VERTEX_POINT ( 'NONE', #25035 ) ;
#8860 = CARTESIAN_POINT ( 'NONE',  ( 101.4615807364564546, 123.6500000010924651, -1.461580736456474794 ) ) ;
#8861 = CARTESIAN_POINT ( 'NONE',  ( 130.0000000000000000, 37.32890625216786873, 13.57481594606304576 ) ) ;
#8862 = CARTESIAN_POINT ( 'NONE',  ( 95.27063293749995410, 84.84375000068281736, -1.387778780781445676E-14 ) ) ;
#8863 = CARTESIAN_POINT ( 'NONE',  ( 208.1451861577818079, 38.56914062608393579, -1.609821015232357215E-15 ) ) ;
#8864 = VERTEX_POINT ( 'NONE', #5517 ) ;
#8865 = CARTESIAN_POINT ( 'NONE',  ( 70.44491438647229131, 36.23750000108393721, 13.14518615778179189 ) ) ;
#8866 = DIRECTION ( 'NONE',  ( -0.000000000000000000, -0.000000000000000000, -1.000000000000000000 ) ) ;
#8867 = CARTESIAN_POINT ( 'NONE',  ( 143.5748159460630688, 39.75976562499999289, 5.622872871577868636 ) ) ;
#8868 = EDGE_LOOP ( 'NONE', ( #17289, #2152, #3856, #18967 ) ) ;
#8869 = CARTESIAN_POINT ( 'NONE',  ( 99.99999999999998579, 102.6397644303321215, -49.50000000000001421 ) ) ;
#8870 = CARTESIAN_POINT ( 'NONE',  ( 9.598844408820459861, 33.45937500216787441, 9.598844408820456309 ) ) ;
#8871 = CARTESIAN_POINT ( 'NONE',  ( 97.93301269999999192, 124.7000000010924623, -0.8561741729129505041 ) ) ;
#8872 = CARTESIAN_POINT ( 'NONE',  ( 116.4251840539369454, 32.31835937716786589, -5.622872871577873077 ) ) ;
#8873 = CARTESIAN_POINT ( 'NONE',  ( 9.295050272127046043, 39.66054687608393436, -9.295050272127046043 ) ) ;
#8874 = CARTESIAN_POINT ( 'NONE',  ( 102.0710678118654613, 94.06249999726880162, -4.999999999999997335 ) ) ;
#8875 = CARTESIAN_POINT ( 'NONE',  ( 74.29505027212704249, 37.08085937608393579, 9.295050272127046043 ) ) ;
#8876 = FACE_OUTER_BOUND ( 'NONE', #9600, .T. ) ;
#8877 = CARTESIAN_POINT ( 'NONE',  ( 185.7049497278729575, 34.30273437608393294, -9.295050272127046043 ) ) ;
#8878 = ORIENTED_EDGE ( 'NONE', *, *, #20853, .F. ) ;
#8879 = EDGE_CURVE ( 'NONE', #19109, #24259, #22902, .T. ) ;
#8880 = VERTEX_POINT ( 'NONE', #1244 ) ;
#8881 = EDGE_LOOP ( 'NONE', ( #23763, #16304, #23292, #14264, #12803, #2305, #795, #18162, #21533, #16455, #20466, #7903, #2636, #15405, #18987 ) ) ;
#8882 = CARTESIAN_POINT ( 'NONE',  ( 13.14518615778179900, 38.81718750108393579, -5.444914386472297529 ) ) ;
#8883 = DIRECTION ( 'NONE',  ( 1.000000000000000000, 0.000000000000000000, 0.000000000000000000 ) ) ;
#8884 = CARTESIAN_POINT ( 'NONE',  ( 99.99999999999995737, 4.458734125000016313, 10.43750000136559208 ) ) ;
#8885 =( BOUNDED_CURVE ( )  B_SPLINE_CURVE ( 2, ( #7892, #12288, #23011, #19143, #16585, #27848, #16727, #5909, #3899 ),
 .UNSPECIFIED., .F., .F. ) 
 B_SPLINE_CURVE_WITH_KNOTS ( ( 3, 2, 2, 2, 3 ),
 ( 0.6041666666666668517, 0.6145833333333334814, 0.6250000000000001110, 0.6354166666666667407, 0.6458333333333333703 ),
 .UNSPECIFIED. ) 
 CURVE ( )  GEOMETRIC_REPRESENTATION_ITEM ( )  RATIONAL_B_SPLINE_CURVE ( ( 0.9999999999999983347, 0.9238795325112884038, 1.000000000000000000, 0.9238795325112867385, 1.000000000000000000, 0.9238795325112867385, 1.000000000000000000, 0.9238795325112867385, 1.000000000000000000 ) ) 
 REPRESENTATION_ITEM ( '' )  );
#8886 = CARTESIAN_POINT ( 'NONE',  ( 55.70494972787295751, 40.45429687608393721, -9.295050272127046043 ) ) ;
#8887 = CARTESIAN_POINT ( 'NONE',  ( 98.15313185440923860, 82.25000000136559208, -4.458734125000016313 ) ) ;
#8888 = CARTESIAN_POINT ( 'NONE',  ( 200.4449143864723055, 38.42031250108393436, 13.14518615778179189 ) ) ;
#8889 = CARTESIAN_POINT ( 'NONE',  ( -5.444914386472297529, 36.63437500108393863, -13.14518615778179722 ) ) ;
#8890 = CARTESIAN_POINT ( 'NONE',  ( 186.7314026716027229, 50.00000000054362914, 10.78867689283715414 ) ) ;
#8891 = AXIS2_PLACEMENT_3D ( 'NONE', #21937, #2553, #6950 ) ;
#8892 = CARTESIAN_POINT ( 'NONE',  ( 99.99999999999995737, -4.999999999999990230, 12.25000000000000000 ) ) ;
#8893 = CARTESIAN_POINT ( 'NONE',  ( 74.59884440882045453, 39.90859374999999432, -9.598844408820458085 ) ) ;
#8894 = CARTESIAN_POINT ( 'NONE',  ( 91.91746824999997045, 107.3738262389971538, -51.52499999726882152 ) ) ;
#8895 = VERTEX_POINT ( 'NONE', #18621 ) ;
#8896 = CARTESIAN_POINT ( 'NONE',  ( 9.598844408820459861, 35.74140624999999716, 9.598844408820456309 ) ) ;
#8897 = CARTESIAN_POINT ( 'NONE',  ( 13.14518615778179900, 37.72578125108393721, 5.444914386472293977 ) ) ;
#8898 = VECTOR ( 'NONE', #8732, 1000.000000000000000 ) ;
#8899 = VECTOR ( 'NONE', #14532, 1000.000000000000000 ) ;
#8900 = ORIENTED_EDGE ( 'NONE', *, *, #22594, .F. ) ;
#8901 = CARTESIAN_POINT ( 'NONE',  ( 116.8548138422182063, 37.62656250108393863, 5.444914386472304635 ) ) ;
#8902 = CARTESIAN_POINT ( 'NONE',  ( 70.44491438647230552, 33.65781250108393152, 13.14518615778179189 ) ) ;
#8903 = CARTESIAN_POINT ( 'NONE',  ( 195.0000000000000000, 35.79101562608394005, -13.14518615778179544 ) ) ;
#8904 = ORIENTED_EDGE ( 'NONE', *, *, #19539, .T. ) ;
#8905 = CARTESIAN_POINT ( 'NONE',  ( 102.0710678118653902, 95.06249999726880162, -5.000000000000047073 ) ) ;
#8906 = CARTESIAN_POINT ( 'NONE',  ( 128.4945078184423153, 53.60078691996341149, -15.00000000000000000 ) ) ;
#8907 = CARTESIAN_POINT ( 'NONE',  ( 70.62287287157796811, 40.75195312499999289, -13.57481594606294095 ) ) ;
#8908 = CARTESIAN_POINT ( 'NONE',  ( 104.9952793366501709, 116.8754121666685393, -53.82500000273119412 ) ) ;
#8909 = CARTESIAN_POINT ( 'NONE',  ( 104.9999999999999716, 1.449011120738813565E-14, 10.49999999999999822 ) ) ;
#8910 = CARTESIAN_POINT ( 'NONE',  ( 98.96446609406727646, 122.8500000021849416, 2.499999999999977796 ) ) ;
#8911 = CARTESIAN_POINT ( 'NONE',  ( -9.598844408820458085, 36.23750000216787726, -9.598844408820458085 ) ) ;
#8912 = EDGE_CURVE ( 'NONE', #17550, #13582, #20939, .T. ) ;
#8913 =( NAMED_UNIT ( * ) SI_UNIT ( $, .STERADIAN. ) SOLID_ANGLE_UNIT ( ) );
#8914 = VERTEX_POINT ( 'NONE', #26354 ) ;
#8915 = CARTESIAN_POINT ( 'NONE',  ( 96.84719886470459471, 3.152801135295383084, 9.312500001365593860 ) ) ;
#8916 = VECTOR ( 'NONE', #12419, 1000.000000000000000 ) ;
#8917 = CARTESIAN_POINT ( 'NONE',  ( 99.99999999999998579, 123.5500000010924850, -2.066987299999998751 ) ) ;
#8918 = CARTESIAN_POINT ( 'NONE',  ( 103.1528011352953342, -3.152801135295355106, 12.81250000136559208 ) ) ;
#8919 = CARTESIAN_POINT ( 'NONE',  ( 125.4284083674797046, 51.44262710532316873, 15.00000000000193978 ) ) ;
#8920 = CARTESIAN_POINT ( 'NONE',  ( -13.14518615778179189, 39.80937500108392868, 5.444914386472304635 ) ) ;
#8921 = FACE_BOUND ( 'NONE', #3481, .T. ) ;
#8922 = CARTESIAN_POINT ( 'NONE',  ( 98.15313185440925281, 80.50000000136560629, -4.458734125000016313 ) ) ;
#8923 = CARTESIAN_POINT ( 'NONE',  ( 78.14518615778179367, 35.64218750108393152, -5.444914386472297529 ) ) ;
#8924 = CARTESIAN_POINT ( 'NONE',  ( 104.9952793366501851, 103.1245878333314323, -44.67500000273118843 ) ) ;
#8925 = CARTESIAN_POINT ( 'NONE',  ( -5.444914386472299306, 36.73359375108393010, 13.14518615778179722 ) ) ;
#8926 = CYLINDRICAL_SURFACE ( 'NONE', #16661, 5.000000000000004441 ) ;
#8927 = FACE_OUTER_BOUND ( 'NONE', #23393, .T. ) ;
#8928 = CARTESIAN_POINT ( 'NONE',  ( 104.9999999999999716, 82.56250000000002842, -2.071067811865491937 ) ) ;
#8929 = CARTESIAN_POINT ( 'NONE',  ( 120.4011555911795455, 37.72578124999999005, -9.598844408820458085 ) ) ;
#8930 = ORIENTED_EDGE ( 'NONE', *, *, #12640, .T. ) ;
#8931 = CARTESIAN_POINT ( 'NONE',  ( 99.99999999999998579, 90.00000000000000000, -4.999999999999996447 ) ) ;
#8932 =( BOUNDED_CURVE ( )  B_SPLINE_CURVE ( 2, ( #9941, #12206, #14765, #4101, #23348 ),
 .UNSPECIFIED., .F., .F. ) 
 B_SPLINE_CURVE_WITH_KNOTS ( ( 3, 2, 3 ),
 ( 0.000000000000000000, 0.01041666666666679446, 0.02083333333333358892 ),
 .UNSPECIFIED. ) 
 CURVE ( )  GEOMETRIC_REPRESENTATION_ITEM ( )  RATIONAL_B_SPLINE_CURVE ( ( 1.000000000000000000, 0.9238795325112867385, 1.000000000000000000, 0.9238795325112848511, 1.000000000000001776 ) ) 
 REPRESENTATION_ITEM ( '' )  );
#8933 = CARTESIAN_POINT ( 'NONE',  ( -8.049105076161786076E-16, 36.58476562608393579, -13.14518615778179544 ) ) ;
#8934 = CARTESIAN_POINT ( 'NONE',  ( 9.598844408820459861, 38.22187500216787015, 9.598844408820456309 ) ) ;
#8935 = CARTESIAN_POINT ( 'NONE',  ( 116.8548138422182063, 37.32890625108393579, -5.444914386472297529 ) ) ;
#8936 = CARTESIAN_POINT ( 'NONE',  ( 78.57481594606304043, 34.30273437716787299, 5.622872871577869525 ) ) ;
#8937 = CARTESIAN_POINT ( 'NONE',  ( 6.831134457305117813, 36.00000000000001421, 11.35217666745981369 ) ) ;
#8938 = CARTESIAN_POINT ( 'NONE',  ( 13.57481594606304931, 31.92148437716787512, 5.622872871577869525 ) ) ;
#8939 = AXIS2_PLACEMENT_3D ( 'NONE', #23426, #23152, #1493 ) ;
#8940 = CARTESIAN_POINT ( 'NONE',  ( 94.99999999999995737, 2.071067811865491048, 2.937499999999999112 ) ) ;
#8941 = CARTESIAN_POINT ( 'NONE',  ( 108.0825317499999869, 112.6261737610028320, -48.77499999726882152 ) ) ;
#8942 = EDGE_CURVE ( 'NONE', #11, #10673, #6812, .T. ) ;
#8943 = CARTESIAN_POINT ( 'NONE',  ( 200.4449143864723055, 33.16171875108393152, -13.14518615778179900 ) ) ;
#8944 = CYLINDRICAL_SURFACE ( 'NONE', #22470, 13.57481594606304576 ) ;
#8945 = CARTESIAN_POINT ( 'NONE',  ( 99.99999999999998579, 93.25000000000000000, -4.999999999999997335 ) ) ;
#8947 = ORIENTED_EDGE ( 'NONE', *, *, #14071, .F. ) ;
#8946 = FACE_OUTER_BOUND ( 'NONE', #10353, .T. ) ;
#8948 = CARTESIAN_POINT ( 'NONE',  ( 195.0000000000000000, 36.83281249999999574, -13.57481594606304576 ) ) ;
#8949 = CARTESIAN_POINT ( 'NONE',  ( 123.8834397602831672, 54.66944451632671331, 14.99999999999996625 ) ) ;
#8950 = CARTESIAN_POINT ( 'NONE',  ( 13.57481594606304753, 38.27148437500000711, -5.622872871577873077 ) ) ;
#8951 = CARTESIAN_POINT ( 'NONE',  ( 93.00000000000000000, 112.2744378736303190, -54.10000000000000853 ) ) ;
#8952 = AXIS2_PLACEMENT_3D ( 'NONE', #2594, #310, #6989 ) ;
#8953 = CARTESIAN_POINT ( 'NONE',  ( -13.14518615778179544, 37.57695312608393579, 0.000000000000000000 ) ) ;
#8954 = CARTESIAN_POINT ( 'NONE',  ( 13.14518615778179900, 37.03125000108393294, -5.444914386472297529 ) ) ;
#8955 = EDGE_CURVE ( 'NONE', #26695, #17655, #10161, .T. ) ;
#8956 = CARTESIAN_POINT ( 'NONE',  ( 181.4251840539369596, 34.69960937499999432, 5.622872871577880183 ) ) ;
#8957 = DIRECTION ( 'NONE',  ( 1.000000000000000000, -3.469446951953519526E-16, -2.385244779468110248E-16 ) ) ;
#8958 = CARTESIAN_POINT ( 'NONE',  ( 13.57481594606304576, 39.01562500000000000, -1.662435489736055892E-15 ) ) ;
#8959 = CARTESIAN_POINT ( 'NONE',  ( 59.55508561352770158, 35.93984375108392726, 13.14518615778179722 ) ) ;
#8960 = EDGE_CURVE ( 'NONE', #8135, #9261, #25925, .T. ) ;
#8961 = CARTESIAN_POINT ( 'NONE',  ( 95.54126587499996504, 1.387778780781445676E-14, 3.437500001365592972 ) ) ;
#8962 = CARTESIAN_POINT ( 'NONE',  ( 99.11671166979772352, 122.9999999999999858, 2.356244385768401894 ) ) ;
#8963 = VERTEX_POINT ( 'NONE', #26497 ) ;
#8964 = CARTESIAN_POINT ( 'NONE',  ( -8.312177448680279460E-16, 36.83281249999999574, -13.57481594606304576 ) ) ;
#8965 = CARTESIAN_POINT ( 'NONE',  ( -5.622872871577873077, 35.59257812499999574, 13.57481594606304753 ) ) ;
#8966 = CARTESIAN_POINT ( 'NONE',  ( 139.2950502721270425, 36.28710937608393294, 9.295050272127046043 ) ) ;
#8967 = EDGE_CURVE ( 'NONE', #11725, #2410, #6399, .T. ) ;
#8968 = ORIENTED_EDGE ( 'NONE', *, *, #20977, .T. ) ;
#8969 = CARTESIAN_POINT ( 'NONE',  ( 99.99999999999995737, 79.93750000136559208, 4.458734124999988779 ) ) ;
#8970 = CARTESIAN_POINT ( 'NONE',  ( 97.92893218813451028, 83.31250000273122680, 4.999999999999989342 ) ) ;
#8971 = CARTESIAN_POINT ( 'NONE',  ( 99.99999999999998579, 92.56249999863440792, -4.458734124999994997 ) ) ;
#8972 = CARTESIAN_POINT ( 'NONE',  ( 64.00443877494754474, 35.99999999999999289, -13.45766439703026407 ) ) ;
#8973 = EDGE_CURVE ( 'NONE', #4933, #2793, #9019, .T. ) ;
#8974 = CARTESIAN_POINT ( 'NONE',  ( 93.00000000000000000, 112.2744378736303332, -53.10000000000000142 ) ) ;
#8975 = CARTESIAN_POINT ( 'NONE',  ( 78.14518615778179367, 33.16171875108393863, 5.444914386472293977 ) ) ;
#8976 = ORIENTED_EDGE ( 'NONE', *, *, #22015, .F. ) ;
#8977 = CARTESIAN_POINT ( 'NONE',  ( 2.493653234604083739E-15, 32.56640625216787299, 13.57481594606304576 ) ) ;
#8978 = CARTESIAN_POINT ( 'NONE',  ( 104.4587341249999781, 1.846868145590750299, 4.250000001365592084 ) ) ;
#8979 = ORIENTED_EDGE ( 'NONE', *, *, #26208, .F. ) ;
#8980 = CARTESIAN_POINT ( 'NONE',  ( 9.180175813647991845, 55.00000000000000000, -9.999999999999998224 ) ) ;
#8981 = CARTESIAN_POINT ( 'NONE',  ( 13.14518615778179544, 39.56132812608393579, -1.609821015232357215E-15 ) ) ;
#8982 = UNCERTAINTY_MEASURE_WITH_UNIT (LENGTH_MEASURE( 1.000000000000000082E-05 ), #9848, 'distance_accuracy_value', 'NONE');
#8983 = CARTESIAN_POINT ( 'NONE',  ( 181.4251840539369596, 33.95546875216787441, 0.000000000000000000 ) ) ;
#8984 = ORIENTED_EDGE ( 'NONE', *, *, #850, .F. ) ;
#8985 = CARTESIAN_POINT ( 'NONE',  ( 9.295050272127047819, 35.29492187608393294, 9.295050272127046043 ) ) ;
#8986 = PRODUCT_DEFINITION_SHAPE ( 'NONE', 'NONE',  #2652 ) ;
#8987 = EDGE_CURVE ( 'NONE', #11020, #5734, #13352, .T. ) ;
#8988 = CARTESIAN_POINT ( 'NONE',  ( 116.8548138422182205, 36.83281250108393579, 5.444914386472304635 ) ) ;
#8989 = VERTEX_POINT ( 'NONE', #18224 ) ;
#8990 = CARTESIAN_POINT ( 'NONE',  ( 2.414731522848535132E-15, 34.60039062608393579, 13.14518615778179544 ) ) ;
#8991 = CARTESIAN_POINT ( 'NONE',  ( 124.5550856135277087, 35.64218750108392442, -13.14518615778179900 ) ) ;
#8992 = CARTESIAN_POINT ( 'NONE',  ( 51.42518405393695957, 34.64999999999999147, 0.000000000000000000 ) ) ;
#8993 = CARTESIAN_POINT ( 'NONE',  ( 100.8561741729129153, 124.5000000010924737, -2.066987299999999195 ) ) ;
#8994 = CARTESIAN_POINT ( 'NONE',  ( 101.8468681455906903, 4.458734125000016313, 10.37500000136559208 ) ) ;
#8995 = CARTESIAN_POINT ( 'NONE',  ( 104.9999999999999716, 1.449011120738813565E-14, 34.79898987322334136 ) ) ;
#8997 = EDGE_CURVE ( 'NONE', #8127, #2410, #27687, .T. ) ;
#8996 = CARTESIAN_POINT ( 'NONE',  ( 104.4587341249999639, 1.442382525525748735E-14, 12.93750000136559208 ) ) ;
#8998 = CARTESIAN_POINT ( 'NONE',  ( 104.9952793366501851, 103.1245878333314323, -48.42500000273120264 ) ) ;
#8999 = CARTESIAN_POINT ( 'NONE',  ( 2.493653234604083739E-15, 34.84843749999999574, 13.57481594606304576 ) ) ;
#9000 = CIRCLE ( 'NONE', #2171, 3.000000000000004441 ) ;
#9001 = CARTESIAN_POINT ( 'NONE',  ( 102.0710678118654329, 83.43750000273121259, 4.999999999999999112 ) ) ;
#9002 = CARTESIAN_POINT ( 'NONE',  ( 104.9952793366501567, 103.1245878333314465, -50.92499999726882010 ) ) ;
#9003 = CARTESIAN_POINT ( 'NONE',  ( -13.14518615778179544, 37.57695312608393579, 0.000000000000000000 ) ) ;
#9004 = EDGE_CURVE ( 'NONE', #162, #5815, #13064, .T. ) ;
#9005 = CARTESIAN_POINT ( 'NONE',  ( 97.83688103937535629, 116.6573956140660897, -46.89999999453763735 ) ) ;
#9006 = ORIENTED_EDGE ( 'NONE', *, *, #25843, .F. ) ;
#9007 = CARTESIAN_POINT ( 'NONE',  ( 195.0000000000000000, 52.00000000000000711, 11.57481594606302266 ) ) ;
#9008 = CARTESIAN_POINT ( 'NONE',  ( 101.4615807364564546, 122.6500000010924794, -1.461580736456474794 ) ) ;
#9009 = DIRECTION ( 'NONE',  ( -0.000000000000000000, -1.000000000000000000, -0.000000000000000000 ) ) ;
#9010 = CARTESIAN_POINT ( 'NONE',  ( 189.5550856135277229, 38.81718750108393579, -13.14518615778179900 ) ) ;
#9011 = ORIENTED_EDGE ( 'NONE', *, *, #10160, .F. ) ;
#9012 = CARTESIAN_POINT ( 'NONE',  ( 99.99999999999998579, 129.0000000000000000, 12.50000000000001066 ) ) ;
#9013 = CARTESIAN_POINT ( 'NONE',  ( 9.598844408820459861, 39.80937500216786873, 9.598844408820456309 ) ) ;
#9014 = CARTESIAN_POINT ( 'NONE',  ( 103.1528011352953342, -3.152801135295355106, 13.06250000136559208 ) ) ;
#9015 = VERTEX_POINT ( 'NONE', #11359 ) ;
#9016 = CARTESIAN_POINT ( 'NONE',  ( 93.46109445667491400, 114.7507929638356785, -51.57500000273120122 ) ) ;
#9017 = CARTESIAN_POINT ( 'NONE',  ( -9.295050272127046043, 39.66054687608393436, -9.295050272127046043 ) ) ;
#9018 = CARTESIAN_POINT ( 'NONE',  ( 97.50000000000000000, 123.3999999999999915, -9.540979117872439019E-15 ) ) ;
#9019 = CIRCLE ( 'NONE', #4487, 4.999999999999997335 ) ;
#9020 = CARTESIAN_POINT ( 'NONE',  ( 135.6228728715778971, 31.82226562716787654, 13.57481594606304576 ) ) ;
#9021 = CARTESIAN_POINT ( 'NONE',  ( 99.99999999999998579, 110.0000000000000000, -145.0000000000000284 ) ) ;
#9022 =( GEOMETRIC_REPRESENTATION_CONTEXT ( 3 ) GLOBAL_UNCERTAINTY_ASSIGNED_CONTEXT ( ( #25449 ) ) GLOBAL_UNIT_ASSIGNED_CONTEXT ( ( #27860, #21159, #10450 ) ) REPRESENTATION_CONTEXT ( 'NONE', 'WORKASPACE' ) );
#9023 = CARTESIAN_POINT ( 'NONE',  ( 97.92893218813452449, 92.56249999726881583, 4.999999999999983125 ) ) ;
#9024 = CARTESIAN_POINT ( 'NONE',  ( 70.44491438647230552, 38.91640625108393436, -13.14518615778179900 ) ) ;
#9025 = CARTESIAN_POINT ( 'NONE',  ( 62.72385315545274409, 51.46995505939283078, -14.99999999999999822 ) ) ;
#9026 = CARTESIAN_POINT ( 'NONE',  ( 189.5550856135277229, 32.66562500108393863, -13.14518615778179900 ) ) ;
#9027 = EDGE_CURVE ( 'NONE', #16597, #23528, #11080, .T. ) ;
#9028 = LINE ( 'NONE', #17720, #18513 ) ;
#9029 = ORIENTED_EDGE ( 'NONE', *, *, #22243, .T. ) ;
#9030 = EDGE_LOOP ( 'NONE', ( #11869, #22814, #11579, #9289 ) ) ;
#9031 = CARTESIAN_POINT ( 'NONE',  ( 9.295050272127047819, 40.25585937608393294, 9.295050272127046043 ) ) ;
#9032 = CARTESIAN_POINT ( 'NONE',  ( 95.54126587499996504, 1.846868145590750077, 12.62500000136559208 ) ) ;
#9033 = CARTESIAN_POINT ( 'NONE',  ( 78.14518615778180788, 39.41250000108393436, -5.444914386472297529 ) ) ;
#9034 = CARTESIAN_POINT ( 'NONE',  ( 59.37712712842218821, 36.48554687716787726, 13.57481594606311504 ) ) ;
#9035 = CARTESIAN_POINT ( 'NONE',  ( 195.0000000000000000, 38.37070312608393152, 13.14518615778179544 ) ) ;
#9036 = CARTESIAN_POINT ( 'NONE',  ( -13.14518615778179189, 38.42031250108393436, 5.444914386472304635 ) ) ;
#9037 = CARTESIAN_POINT ( 'NONE',  ( 195.0000000000000000, 38.51953125216787299, -13.57481594606304576 ) ) ;
#9038 = CARTESIAN_POINT ( 'NONE',  ( 91.91746824999997045, 107.3738262389971538, -55.52499999726882862 ) ) ;
#9039 = VECTOR ( 'NONE', #12896, 1000.000000000000000 ) ;
#9040 = CIRCLE ( 'NONE', #15809, 3.000000000000004441 ) ;
#9041 = ORIENTED_EDGE ( 'NONE', *, *, #5070, .T. ) ;
#9042 = CARTESIAN_POINT ( 'NONE',  ( -13.57481594606304576, 36.23749999999999005, 0.000000000000000000 ) ) ;
#9043 = CARTESIAN_POINT ( 'NONE',  ( -5.444914386472297529, 37.22968750108393721, -13.14518615778179900 ) ) ;
#9044 = VECTOR ( 'NONE', #2550, 999.9999999999997726 ) ;
#9045 = VERTEX_POINT ( 'NONE', #5259 ) ;
#9046 = PLANE ( 'NONE',  #23429 ) ;
#9047 = CARTESIAN_POINT ( 'NONE',  ( 59.55508561352770158, 34.05468750108393294, -13.14518615778179900 ) ) ;
#9048 = CARTESIAN_POINT ( 'NONE',  ( 189.5550856135277229, 38.51953125108393294, 13.14518615778179722 ) ) ;
#9049 = EDGE_LOOP ( 'NONE', ( #14719, #9743, #7018, #19855 ) ) ;
#9050 = LINE ( 'NONE', #13295, #5700 ) ;
#9051 = CARTESIAN_POINT ( 'NONE',  ( -13.14518615778179900, 31.77265625108393365, -5.444914386472297529 ) ) ;
#9052 =( BOUNDED_CURVE ( )  B_SPLINE_CURVE ( 2, ( #15752, #6917, #15610, #20722, #24312, #24455, #5331, #13996, #1204 ),
 .UNSPECIFIED., .F., .F. ) 
 B_SPLINE_CURVE_WITH_KNOTS ( ( 3, 2, 2, 2, 3 ),
 ( 0.5000000000000000000, 0.5089285714285713969, 0.5178571428571429047, 0.5267857142857143016, 0.5357142857142856984 ),
 .UNSPECIFIED. ) 
 CURVE ( )  GEOMETRIC_REPRESENTATION_ITEM ( )  RATIONAL_B_SPLINE_CURVE ( ( 1.000000000000000000, 0.9238795325112867385, 1.000000000000000000, 0.9238795325112867385, 1.000000000000000000, 0.9238795325112867385, 1.000000000000000000, 0.9238795325112867385, 1.000000000000000000 ) ) 
 REPRESENTATION_ITEM ( '' )  );
#9053 = CARTESIAN_POINT ( 'NONE',  ( 99.99999999999998579, 124.1000000021849416, -2.499999999999997780 ) ) ;
#9054 = CARTESIAN_POINT ( 'NONE',  ( 74.59884440882045453, 40.70234374999999716, -9.598844408820458085 ) ) ;
#9055 = CARTESIAN_POINT ( 'NONE',  ( 0.000000000000000000, -7.395377635281828788, 11.57481594606304398 ) ) ;
#9056 = CARTESIAN_POINT ( 'NONE',  ( 94.99999999999995737, -2.071067811865466624, 2.187500002731185056 ) ) ;
#9057 = CARTESIAN_POINT ( 'NONE',  ( 60.07497321633574217, 49.99999999893042713, 12.67776588291749462 ) ) ;
#9058 = EDGE_LOOP ( 'NONE', ( #5031, #14291, #5282, #20124 ) ) ;
#9059 = CARTESIAN_POINT ( 'NONE',  ( 96.84719886470459471, -3.152801135295355994, 9.562500001365593860 ) ) ;
#9060 = ORIENTED_EDGE ( 'NONE', *, *, #25499, .T. ) ;
#9061 = CARTESIAN_POINT ( 'NONE',  ( 99.99999999999998579, 124.3500000010924822, -2.066987299999998751 ) ) ;
#9062 = CARTESIAN_POINT ( 'NONE',  ( 98.15313185440925281, -4.458734124999987891, 7.625000001365592084 ) ) ;
#9063 = CARTESIAN_POINT ( 'NONE',  ( 99.99999999999998579, 90.00000000000000000, -6.938893903907228378E-15 ) ) ;
#9064 = CARTESIAN_POINT ( 'NONE',  ( -13.14518615778179544, 36.58476562608393579, 0.000000000000000000 ) ) ;
#9065 = CARTESIAN_POINT ( 'NONE',  ( 99.99999999999998579, 123.0000000000000000, -5.204170427930421283E-15 ) ) ;
#9066 = CARTESIAN_POINT ( 'NONE',  ( 103.1528011352953342, 81.31250000136559208, -3.152801135295383084 ) ) ;
#9067 = CARTESIAN_POINT ( 'NONE',  ( 74.29505027212704249, 35.69179687608394147, -9.295050272127046043 ) ) ;
#9068 = CARTESIAN_POINT ( 'NONE',  ( 97.50236033167492167, 117.6869444889999841, -53.52500000273118985 ) ) ;
#9069 = CARTESIAN_POINT ( 'NONE',  ( 9.295050272127046043, 36.28710937608393294, -9.295050272127046043 ) ) ;
#9070 = CARTESIAN_POINT ( 'NONE',  ( 2.493653234604083739E-15, 33.26093749999999716, 13.57481594606304576 ) ) ;
#9071 = CARTESIAN_POINT ( 'NONE',  ( 105.6631189606246153, 114.1144967660473242, -55.29999999453764303 ) ) ;
#9072 = CARTESIAN_POINT ( 'NONE',  ( 124.3771271284221314, 37.67617187499999432, -13.57481594606304753 ) ) ;
#9073 = EDGE_LOOP ( 'NONE', ( #19668, #18083, #16582, #24136 ) ) ;
#9074 = VERTEX_POINT ( 'NONE', #11929 ) ;
#9075 = CARTESIAN_POINT ( 'NONE',  ( 97.92893218813451028, -4.999999999999989342, 8.187500000000000000 ) ) ;
#9076 = CARTESIAN_POINT ( 'NONE',  ( -13.14518615778179900, 38.32109375108394289, -5.444914386472297529 ) ) ;
#9077 = CARTESIAN_POINT ( 'NONE',  ( -13.57481594606304576, 37.18007812716787441, 5.622872871577880183 ) ) ;
#9078 = CARTESIAN_POINT ( 'NONE',  ( 103.5355339059327093, -3.535533905932726206, 9.500000002731184168 ) ) ;
#9079 = CARTESIAN_POINT ( 'NONE',  ( 116.8548138422182063, 36.53515625108392584, -5.444914386472297529 ) ) ;
#9080 = CARTESIAN_POINT ( 'NONE',  ( 51.42518405393695957, 34.79882812716787299, 5.622872871577880183 ) ) ;
#9081 = EDGE_CURVE ( 'NONE', #20134, #152, #15843, .T. ) ;
#9082 = CARTESIAN_POINT ( 'NONE',  ( 99.99999999999995737, 83.75000000000000000, -5.000000000000018652 ) ) ;
#9083 = CARTESIAN_POINT ( 'NONE',  ( -5.622872871577873077, 33.31054687716787299, 13.57481594606304753 ) ) ;
#9084 = CIRCLE ( 'NONE', #6352, 7.000000000000006217 ) ;
#9085 = DIRECTION ( 'NONE',  ( 0.000000000000000000, 0.000000000000000000, 1.000000000000000000 ) ) ;
#9086 = CARTESIAN_POINT ( 'NONE',  ( 108.0825317500000011, 110.0000000000000000, -46.87499999726882294 ) ) ;
#9087 = CARTESIAN_POINT ( 'NONE',  ( 204.2950502721270425, 34.50117187608393010, 9.295050272127046043 ) ) ;
#9088 = CYLINDRICAL_SURFACE ( 'NONE', #21107, 13.57481594606304398 ) ;
#9089 = AXIS2_PLACEMENT_3D ( 'NONE', #3758, #7883, #5759 ) ;
#9090 = CARTESIAN_POINT ( 'NONE',  ( 103.5355339059327093, 81.62500000000000000, -3.535533905932755072 ) ) ;
#9091 = ORIENTED_EDGE ( 'NONE', *, *, #14686, .T. ) ;
#9092 = DIRECTION ( 'NONE',  ( 8.659560562354927928E-17, -0.7071067811865482389, 0.7071067811865469066 ) ) ;
#9093 = CARTESIAN_POINT ( 'NONE',  ( 0.000000000000000000, 23.00000000000000000, 0.000000000000000000 ) ) ;
#9094 = CARTESIAN_POINT ( 'NONE',  ( 130.7197605961091824, 53.51499872091923038, 14.99999999999996447 ) ) ;
#9095 = CARTESIAN_POINT ( 'NONE',  ( 2.493653234604083739E-15, 38.02343749999999289, 13.57481594606304576 ) ) ;
#9096 = CARTESIAN_POINT ( 'NONE',  ( 104.3262379212492448, 115.9545556584642867, -45.70000000000000995 ) ) ;
#9097 = CARTESIAN_POINT ( 'NONE',  ( 5.444914386472302859, 36.23750000108393721, 13.14518615778179189 ) ) ;
#9098 = CARTESIAN_POINT ( 'NONE',  ( -13.14518615778179189, 37.42812500108393436, 5.444914386472304635 ) ) ;
#9099 = CARTESIAN_POINT ( 'NONE',  ( 200.6228728715778686, 35.98945312499999716, -13.57481594606304753 ) ) ;
#9100 = CARTESIAN_POINT ( 'NONE',  ( 104.7293670624999748, 90.71874999795159056, -6.938893903907228378E-15 ) ) ;
#9101 = CARTESIAN_POINT ( 'NONE',  ( 95.54126587499996504, 1.387778780781445676E-14, 0.6875000013655923059 ) ) ;
#9102 = CARTESIAN_POINT ( 'NONE',  ( 51.85481384221820633, 35.79101562608393294, 0.000000000000000000 ) ) ;
#9103 =( BOUNDED_SURFACE ( )  B_SPLINE_SURFACE ( 1, 2, ( 
 ( #25330, #6226, #19191, #12342, #27620, #10759, #27893, #5816, #17040, #14892, #8077, #16773, #19047, #5952, #3811, #4089, #12754, #1953, #17605, #26165, #6773, #11175, #8774, #22178, #11461, #15459, #6632, #20180, #377, #8638, #7048, #15316, #13166, #17328, #11318, #22037, #19893, #230, #4651, #4937, #15170 ),
 ( #15747, #26312, #24030, #24174, #9061, #17463, #2657, #26023, #13310, #4509, #6494, #17756, #23889, #24451, #21905, #2379, #4368, #20040, #2513, #26459, #8917, #6913, #13600, #9200, #519, #15604, #13024, #21761, #22323, #24307, #11037, #19747, #4793, #13452, #2238, #17894, #10900, #26602, #2794, #19608, #93 ) ),
 .UNSPECIFIED., .F., .F., .F. ) 
 B_SPLINE_SURFACE_WITH_KNOTS ( ( 2, 2 ),
 ( 3, 2, 2, 2, 2, 2, 2, 2, 2, 2, 2, 2, 2, 2, 2, 2, 2, 2, 2, 2, 3 ),
 ( 0.000000000000000000, 1.000000000000000000 ),
 ( 0.000000000000000000, 0.04166666666666666435, 0.08333333333333332871, 0.1250000000000000000, 0.1666666666666666574, 0.2083333333333333426, 0.2500000000000000000, 0.2916666666666666852, 0.3333333333333333148, 0.3750000000000000000, 0.4166666666666666852, 0.4583333333333333148, 0.5000000000000000000, 0.5416666666666666297, 0.5833333333333333703, 0.6250000000000000000, 0.6666666666666666297, 0.7083333333333333703, 0.7500000000000000000, 0.7916666666666666297, 0.8333333333333333703 ),
 .UNSPECIFIED. ) 
 GEOMETRIC_REPRESENTATION_ITEM ( )  RATIONAL_B_SPLINE_SURFACE ( (
 ( 1.000000000000000000, 0.9238795325112867385, 1.000000000000000000, 0.9238795325112867385, 1.000000000000000000, 0.9238795325112867385, 1.000000000000000000, 0.9238795325112867385, 1.000000000000000000, 0.9238795325112867385, 1.000000000000000000, 0.9238795325112867385, 1.000000000000000000, 0.9238795325112867385, 1.000000000000000000, 0.9238795325112867385, 1.000000000000000000, 0.9238795325112867385, 1.000000000000000000, 0.9238795325112867385, 1.000000000000000000, 0.9238795325112867385, 1.000000000000000000, 0.9238795325112867385, 1.000000000000000000, 0.9238795325112867385, 1.000000000000000000, 0.9238795325112867385, 1.000000000000000000, 0.9238795325112867385, 1.000000000000000000, 0.9238795325112867385, 1.000000000000000000, 0.9238795325112867385, 1.000000000000000000, 0.9238795325112867385, 1.000000000000000000, 0.9238795325112867385, 1.000000000000000000, 0.9238795325112867385, 1.000000000000000000),
 ( 1.000000000000000000, 0.9238795325112867385, 1.000000000000000000, 0.9238795325112867385, 1.000000000000000000, 0.9238795325112867385, 1.000000000000000000, 0.9238795325112867385, 1.000000000000000000, 0.9238795325112867385, 1.000000000000000000, 0.9238795325112867385, 1.000000000000000000, 0.9238795325112867385, 1.000000000000000000, 0.9238795325112867385, 1.000000000000000000, 0.9238795325112867385, 1.000000000000000000, 0.9238795325112867385, 1.000000000000000000, 0.9238795325112867385, 1.000000000000000000, 0.9238795325112867385, 1.000000000000000000, 0.9238795325112867385, 1.000000000000000000, 0.9238795325112867385, 1.000000000000000000, 0.9238795325112867385, 1.000000000000000000, 0.9238795325112867385, 1.000000000000000000, 0.9238795325112867385, 1.000000000000000000, 0.9238795325112867385, 1.000000000000000000, 0.9238795325112867385, 1.000000000000000000, 0.9238795325112867385, 1.000000000000000000) ) ) 
 REPRESENTATION_ITEM ( '' )  SURFACE ( )  );
#9104 = CARTESIAN_POINT ( 'NONE',  ( 103.1528011352953342, 3.152801135295383084, 2.062500001365591640 ) ) ;
#9105 = CARTESIAN_POINT ( 'NONE',  ( 97.56535394163772423, 123.0000000000000142, 0.5875565381436620438 ) ) ;
#9106 = CARTESIAN_POINT ( 'NONE',  ( 99.99999999999998579, 93.12499999726881583, -4.999999999999997335 ) ) ;
#9107 = CARTESIAN_POINT ( 'NONE',  ( -13.57481594606304753, 37.77539062499999289, -5.622872871577873077 ) ) ;
#9108 = CARTESIAN_POINT ( 'NONE',  ( 139.2950502721270425, 38.66835937608393436, 9.295050272127046043 ) ) ;
#9109 = ORIENTED_EDGE ( 'NONE', *, *, #16138, .F. ) ;
#9110 = CARTESIAN_POINT ( 'NONE',  ( 96.84719886470459471, 80.56250000136559208, -3.152801135295383084 ) ) ;
#9111 = FACE_OUTER_BOUND ( 'NONE', #20130, .T. ) ;
#9112 = CARTESIAN_POINT ( 'NONE',  ( 99.99999999999995737, 81.37500000273119838, 4.999999999999990230 ) ) ;
#9113 = CARTESIAN_POINT ( 'NONE',  ( 98.15313185440925281, 93.62499999863440792, -4.458734124999994997 ) ) ;
#9114 = CARTESIAN_POINT ( 'NONE',  ( 96.84719886470463734, 95.18749999863440792, 3.152801135295351997 ) ) ;
#9115 = CARTESIAN_POINT ( 'NONE',  ( 102.1631189606246295, 103.3426043859339103, -48.40000000000001279 ) ) ;
#9116 = CARTESIAN_POINT ( 'NONE',  ( 51.42518405393695957, 39.46210937499999005, 5.622872871577880183 ) ) ;
#9117 = ORIENTED_EDGE ( 'NONE', *, *, #7591, .T. ) ;
#9118 = EDGE_CURVE ( 'NONE', #27809, #1909, #12001, .T. ) ;
#9119 = CARTESIAN_POINT ( 'NONE',  ( 214.9999999999999716, 75.00000000000000000, 0.000000000000000000 ) ) ;
#9120 = CARTESIAN_POINT ( 'NONE',  ( 96.84719886470459471, -3.152801135295355994, 0.8125000013655924169 ) ) ;
#9121 = EDGE_CURVE ( 'NONE', #25739, #18276, #20425, .T. ) ;
#9122 = ORIENTED_EDGE ( 'NONE', *, *, #116, .F. ) ;
#9123 = CARTESIAN_POINT ( 'NONE',  ( 13.14518615778179900, 35.64218750108393152, -5.444914386472297529 ) ) ;
#9124 = CARTESIAN_POINT ( 'NONE',  ( 200.6228728715778686, 35.79101562716787299, 13.57481594606304576 ) ) ;
#9125 = CARTESIAN_POINT ( 'NONE',  ( 5.444914386472302859, 32.07031250108393294, 13.14518615778179189 ) ) ;
#9126 = CARTESIAN_POINT ( 'NONE',  ( 9.598844408820456309, 36.83281250216787583, -9.598844408820458085 ) ) ;
#9127 = CARTESIAN_POINT ( 'NONE',  ( 130.0000000000000000, 36.98164062608393721, 13.14518615778179544 ) ) ;
#9128 = ORIENTED_EDGE ( 'NONE', *, *, #5622, .F. ) ;
#9129 = CARTESIAN_POINT ( 'NONE',  ( 9.295050272127046043, 36.48554687608393721, -9.295050272127046043 ) ) ;
#9130 = FACE_OUTER_BOUND ( 'NONE', #16005, .T. ) ;
#9131 = CARTESIAN_POINT ( 'NONE',  ( 55.40115559117954547, 35.34453124999998863, -9.598844408820458085 ) ) ;
#9132 = CARTESIAN_POINT ( 'NONE',  ( 102.0669872999999797, 124.3500000010924822, -9.794112055954760458E-15 ) ) ;
#9133 = CARTESIAN_POINT ( 'NONE',  ( 103.1528011352953342, -3.152801135295355106, 13.06250000136559208 ) ) ;
#9134 = CARTESIAN_POINT ( 'NONE',  ( 99.99999999999995737, 85.00000000000000000, -1.387778780781445676E-14 ) ) ;
#9135 = AXIS2_PLACEMENT_3D ( 'NONE', #9404, #26672, #20395 ) ;
#9136 = CARTESIAN_POINT ( 'NONE',  ( 104.4587341249999639, 1.442382525525748735E-14, 1.937500001365591640 ) ) ;
#9137 = CARTESIAN_POINT ( 'NONE',  ( 91.91746824999998466, 107.3738262389971538, -49.02500000273119696 ) ) ;
#9138 = DIRECTION ( 'NONE',  ( 5.782411586589357392E-17, -0.000000000000000000, 1.000000000000000000 ) ) ;
#9139 = DIRECTION ( 'NONE',  ( -0.000000000000000000, 1.000000000000000000, -0.000000000000000000 ) ) ;
#9140 = CARTESIAN_POINT ( 'NONE',  ( 102.4976396683250783, 117.6869444889999841, -48.22499999726881725 ) ) ;
#9141 = CARTESIAN_POINT ( 'NONE',  ( -13.14518615778179189, 35.24531250108393721, 5.444914386472304635 ) ) ;
#9142 = CARTESIAN_POINT ( 'NONE',  ( 106.5389055433250860, 105.2492070361643215, -53.07499999726881867 ) ) ;
#9143 = ORIENTED_EDGE ( 'NONE', *, *, #6712, .T. ) ;
#9144 = CARTESIAN_POINT ( 'NONE',  ( 98.53841926354351699, 123.8500000010924680, -1.461580736456474794 ) ) ;
#9145 = SHAPE_REPRESENTATION ( 'Suction Cups Set (x4)', ( #26844 ), #17253 ) ;
#9146 = CARTESIAN_POINT ( 'NONE',  ( 98.53841926354351699, 123.0500000010924850, 1.461580736456455920 ) ) ;
#9147 = DIRECTION ( 'NONE',  ( 5.782411586589357392E-17, 3.469446951953611231E-16, 1.000000000000000000 ) ) ;
#9148 = VECTOR ( 'NONE', #25138, 1000.000000000000000 ) ;
#9149 = CARTESIAN_POINT ( 'NONE',  ( 208.1451861577818079, 36.18789062608393436, -1.609821015232357215E-15 ) ) ;
#9150 = EDGE_LOOP ( 'NONE', ( #17015, #16319, #17844, #20861 ) ) ;
#9151 = EDGE_CURVE ( 'NONE', #10542, #20304, #13923, .T. ) ;
#9152 = EDGE_CURVE ( 'NONE', #23528, #4431, #3234, .T. ) ;
#9153 = CARTESIAN_POINT ( 'NONE',  ( 98.15313185440925281, -4.458734124999987891, 9.875000001365593860 ) ) ;
#9154 = ORIENTED_EDGE ( 'NONE', *, *, #8967, .F. ) ;
#9155 = CARTESIAN_POINT ( 'NONE',  ( 108.0825317500000011, 112.6261737610028320, -54.27500000273118275 ) ) ;
#9156 = CIRCLE ( 'NONE', #7059, 5.000000000000004441 ) ;
#9157 = FACE_OUTER_BOUND ( 'NONE', #5559, .T. ) ;
#9158 = CARTESIAN_POINT ( 'NONE',  ( 100.8561741729129153, 122.9000000010924936, -2.066987299999999195 ) ) ;
#9159 = EDGE_CURVE ( 'NONE', #10007, #26290, #14073, .T. ) ;
#9160 = CARTESIAN_POINT ( 'NONE',  ( 139.5988444088204687, 31.87187500216787228, 9.598844408820456309 ) ) ;
#9161 = CARTESIAN_POINT ( 'NONE',  ( -9.295050272127046043, 40.65273437608393436, -9.295050272127046043 ) ) ;
#9162 = CARTESIAN_POINT ( 'NONE',  ( 99.99999999999998579, 95.12499999726881583, -4.999999999999997335 ) ) ;
#9163 = CARTESIAN_POINT ( 'NONE',  ( 78.14518615778179367, 37.22968750108393721, -5.444914386472297529 ) ) ;
#9164 = CARTESIAN_POINT ( 'NONE',  ( 61.02018555418613488, 50.00000000123296218, -13.01613927312751429 ) ) ;
#9165 = CARTESIAN_POINT ( 'NONE',  ( 108.0825317500000011, 107.3738262389971680, -50.47500000273119269 ) ) ;
#9166 = CARTESIAN_POINT ( 'NONE',  ( 204.2950502721270425, 33.11210937608393579, 9.295050272127046043 ) ) ;
#9167 = EDGE_CURVE ( 'NONE', #6002, #24722, #18509, .T. ) ;
#9168 = DIRECTION ( 'NONE',  ( -1.000000000000000000, 0.000000000000000000, 0.000000000000000000 ) ) ;
#9169 = ORIENTED_EDGE ( 'NONE', *, *, #14543, .F. ) ;
#9170 = CARTESIAN_POINT ( 'NONE',  ( -5.444914386472297529, 35.04687500108393294, -13.14518615778179900 ) ) ;
#9171 = CARTESIAN_POINT ( 'NONE',  ( 95.54126587499996504, 1.846868145590750077, 11.62500000136559031 ) ) ;
#9172 = CARTESIAN_POINT ( 'NONE',  ( 51.85481384221820633, 38.17226562608393436, 0.000000000000000000 ) ) ;
#9173 = CARTESIAN_POINT ( 'NONE',  ( 0.000000000000000000, 20.53589838486225361, 23.00000000000001421 ) ) ;
#9174 = CARTESIAN_POINT ( 'NONE',  ( 99.99999999999995737, -4.999999999999990230, 2.249999999999998668 ) ) ;
#9175 = ORIENTED_EDGE ( 'NONE', *, *, #28145, .T. ) ;
#9176 = CARTESIAN_POINT ( 'NONE',  ( 13.14518615778179722, 36.43593750108394147, -5.444914386472297529 ) ) ;
#9177 = CARTESIAN_POINT ( 'NONE',  ( 87.00000000000000000, 120.0000000000000000, -43.00000000000000000 ) ) ;
#9178 = CARTESIAN_POINT ( 'NONE',  ( 181.8548138422182205, 38.42031250108393436, 5.444914386472304635 ) ) ;
#9179 = CARTESIAN_POINT ( 'NONE',  ( 95.00472066334982912, 103.1245878333314323, -51.32499999726880446 ) ) ;
#9180 = ORIENTED_EDGE ( 'NONE', *, *, #16115, .T. ) ;
#9181 = CARTESIAN_POINT ( 'NONE',  ( -5.622872871577873077, 33.21132812499999432, 13.57481594606304753 ) ) ;
#9182 = CARTESIAN_POINT ( 'NONE',  ( -13.14518615778179900, 34.15390625108393863, -5.444914386472297529 ) ) ;
#9183 = ORIENTED_EDGE ( 'NONE', *, *, #608, .T. ) ;
#9184 = CARTESIAN_POINT ( 'NONE',  ( 124.5550856135277087, 33.75703125108393721, 13.14518615778179722 ) ) ;
#9185 = CARTESIAN_POINT ( 'NONE',  ( 65.00000000000000000, 35.19570312608392726, 13.14518615778179544 ) ) ;
#9186 = CARTESIAN_POINT ( 'NONE',  ( 204.2950502721270425, 36.28710937608393294, 9.295050272127046043 ) ) ;
#9187 = EDGE_LOOP ( 'NONE', ( #23937, #19249, #19062, #17736, #14281, #3652, #19700, #18386, #12753, #26619, #660, #5918, #6357, #27951, #8737, #4285 ) ) ;
#9188 = CARTESIAN_POINT ( 'NONE',  ( 101.4615807364564546, 124.0500000010924850, 1.461580736456455476 ) ) ;
#9189 = CARTESIAN_POINT ( 'NONE',  ( -13.14518615778179900, 33.36015625108393579, -5.444914386472297529 ) ) ;
#9190 = CARTESIAN_POINT ( 'NONE',  ( 102.4999999999999858, 123.9000000021849530, -9.847140817659276890E-15 ) ) ;
#9191 = EDGE_CURVE ( 'NONE', #15219, #3701, #3290, .T. ) ;
#9192 = CARTESIAN_POINT ( 'NONE',  ( 120.4011555911795455, 40.20625000216787726, -9.598844408820458085 ) ) ;
#9193 = CARTESIAN_POINT ( 'NONE',  ( 108.0825317500000011, 107.3738262389971680, -52.22500000273119269 ) ) ;
#9194 = DIRECTION ( 'NONE',  ( -0.000000000000000000, 1.000000000000000000, -0.000000000000000000 ) ) ;
#9195 = CARTESIAN_POINT ( 'NONE',  ( -9.598844408820454532, 34.84843750216787583, 9.598844408820459861 ) ) ;
#9196 = CARTESIAN_POINT ( 'NONE',  ( 67.52958399517125088, 49.99999999938368944, 13.34625891065909897 ) ) ;
#9197 = SHAPE_REPRESENTATION_RELATIONSHIP ( 'NONE' , 'NONE' ,  #19878, #15807 ) ;
#9198 = CARTESIAN_POINT ( 'NONE',  ( 95.54126587499996504, 1.387778780781445676E-14, 3.437500001365592972 ) ) ;
#9199 = VERTEX_POINT ( 'NONE', #10205 ) ;
#9200 = CARTESIAN_POINT ( 'NONE',  ( 102.0669872999999939, 123.4000000010924936, -0.8561741729129507261 ) ) ;
#9201 = CARTESIAN_POINT ( 'NONE',  ( 95.54126587499996504, 1.387778780781445676E-14, 7.437500001365592084 ) ) ;
#9202 = DIRECTION ( 'NONE',  ( -0.000000000000000000, -1.000000000000000000, -0.000000000000000000 ) ) ;
#9203 = CARTESIAN_POINT ( 'NONE',  ( 9.295050272127047819, 35.29492187608393294, 9.295050272127046043 ) ) ;
#9204 = DIRECTION ( 'NONE',  ( 0.000000000000000000, 1.000000000000000000, 0.000000000000000000 ) ) ;
#9205 = CARTESIAN_POINT ( 'NONE',  ( 93.00000000000000000, 107.7255621263696668, -52.40000000546238113 ) ) ;
#9206 = CARTESIAN_POINT ( 'NONE',  ( 55.70494972787295751, 35.29492187608393294, 9.295050272127047819 ) ) ;
#9207 = CARTESIAN_POINT ( 'NONE',  ( 189.3771271284220745, 37.67617187499999432, -13.57481594606304753 ) ) ;
#9208 = CARTESIAN_POINT ( 'NONE',  ( -13.14518615778179722, 37.32890625108393579, -5.444914386472297529 ) ) ;
#9209 = CARTESIAN_POINT ( 'NONE',  ( 99.99999999999998579, 138.0000000000000000, -12.50000000000002132 ) ) ;
#9210 = CARTESIAN_POINT ( 'NONE',  ( 8.259611528887869980, 50.00000000056319038, 10.79618466885915851 ) ) ;
#9211 = CARTESIAN_POINT ( 'NONE',  ( 99.99999999999998579, 138.0000000000000000, 12.50000000000001066 ) ) ;
#9212 = CARTESIAN_POINT ( 'NONE',  ( 130.0000000000000000, 36.83281249999999574, -13.57481594606304576 ) ) ;
#9213 = ORIENTED_EDGE ( 'NONE', *, *, #3429, .T. ) ;
#9214 = VECTOR ( 'NONE', #1366, 1000.000000000000000 ) ;
#9215 = ORIENTED_EDGE ( 'NONE', *, *, #5672, .F. ) ;
#9216 = CARTESIAN_POINT ( 'NONE',  ( -8.312177448680279460E-16, 34.55078125216787299, -13.57481594606304576 ) ) ;
#9217 = CARTESIAN_POINT ( 'NONE',  ( -8.049105076161786076E-16, 35.79101562608394005, -13.14518615778179544 ) ) ;
#9218 = CARTESIAN_POINT ( 'NONE',  ( 13.57481594606304753, 37.57695312716787583, -5.622872871577873077 ) ) ;
#9219 =( BOUNDED_CURVE ( )  B_SPLINE_CURVE ( 2, ( #20478, #1100, #4801, #2801, #13460, #20047, #24459, #9207, #17901 ),
 .UNSPECIFIED., .F., .F. ) 
 B_SPLINE_CURVE_WITH_KNOTS ( ( 3, 2, 2, 2, 3 ),
 ( 0.3125000000000002220, 0.3229166666666668517, 0.3333333333333334259, 0.3437500000000000555, 0.3541666666666666852 ),
 .UNSPECIFIED. ) 
 CURVE ( )  GEOMETRIC_REPRESENTATION_ITEM ( )  RATIONAL_B_SPLINE_CURVE ( ( 0.9999999999999983347, 0.9238795325112884038, 1.000000000000000000, 0.9238795325112867385, 1.000000000000000000, 0.9238795325112867385, 1.000000000000000000, 0.9238795325112867385, 1.000000000000000000 ) ) 
 REPRESENTATION_ITEM ( '' )  );
#9220 = CARTESIAN_POINT ( 'NONE',  ( 102.0710678118654329, 5.000000000000018652, 8.812500002731182391 ) ) ;
#9221 = CARTESIAN_POINT ( 'NONE',  ( 120.7049497278729575, 33.50898437608393010, 9.295050272127047819 ) ) ;
#9222 = CARTESIAN_POINT ( 'NONE',  ( 59.37712712842213136, 34.60039062716786873, -13.57481594606304753 ) ) ;
#9223 = DIRECTION ( 'NONE',  ( 1.000000000000000000, 0.000000000000000000, -2.385244779468110248E-16 ) ) ;
#9224 = CARTESIAN_POINT ( 'NONE',  ( 13.57481594606304931, 33.50898437716787015, 5.622872871577869525 ) ) ;
#9225 = CARTESIAN_POINT ( 'NONE',  ( 0.000000000000000000, 36.00000000000000000, 0.000000000000000000 ) ) ;
#9226 = CARTESIAN_POINT ( 'NONE',  ( 91.91746824999998466, 110.0000000000000000, -45.87499999726882294 ) ) ;
#9227 = CARTESIAN_POINT ( 'NONE',  ( 13.57481594606304753, 39.95820312716787726, -5.622872871577873077 ) ) ;
#9228 = CARTESIAN_POINT ( 'NONE',  ( 185.7049497278729575, 35.89023437608393152, 9.295050272127047819 ) ) ;
#9229 = CARTESIAN_POINT ( 'NONE',  ( -13.57481594606304398, 31.62382812716787228, 5.622872871577880183 ) ) ;
#9230 = FACE_OUTER_BOUND ( 'NONE', #964, .T. ) ;
#9231 = VECTOR ( 'NONE', #8584, 1000.000000000000000 ) ;
#9232 = CARTESIAN_POINT ( 'NONE',  ( 99.99999999999998579, 130.0000000000000000, -0.5000000000000138778 ) ) ;
#9233 = CARTESIAN_POINT ( 'NONE',  ( 97.92893218813455292, 94.56249999726881583, 5.000000000000023981 ) ) ;
#9234 = CARTESIAN_POINT ( 'NONE',  ( 94.99999999999995737, 1.387778780781445676E-14, 10.12500000273118594 ) ) ;
#9235 = LINE ( 'NONE', #17927, #16953 ) ;
#9236 = CARTESIAN_POINT ( 'NONE',  ( 5.622872871577871301, 35.98945312499999716, -13.57481594606304753 ) ) ;
#9237 = CARTESIAN_POINT ( 'NONE',  ( -9.180175813648000727, 55.00000000000014211, -9.999999999999998224 ) ) ;
#9238 = CARTESIAN_POINT ( 'NONE',  ( 2.414731522848535132E-15, 34.60039062608393579, 13.14518615778179544 ) ) ;
#9239 = CARTESIAN_POINT ( 'NONE',  ( 2.414731522848535132E-15, 35.19570312608392726, 13.14518615778179544 ) ) ;
#9240 = CARTESIAN_POINT ( 'NONE',  ( 195.0000000000000000, 33.65781249999999147, -13.57481594606304576 ) ) ;
#9241 = CARTESIAN_POINT ( 'NONE',  ( 13.57481594606304931, 37.47773437716787726, 5.622872871577869525 ) ) ;
#9242 = CARTESIAN_POINT ( 'NONE',  ( 13.57481594606304931, 38.96601562499999005, 5.622872871577868636 ) ) ;
#9243 = CARTESIAN_POINT ( 'NONE',  ( 55.70494972787295751, 35.09648437608392868, 9.295050272127047819 ) ) ;
#9244 = ADVANCED_FACE ( 'NONE', ( #22932 ), #12618, .F. ) ;
#9245 = CARTESIAN_POINT ( 'NONE',  ( 195.0000000000000000, -7.395377635281828788, 13.57481594606302266 ) ) ;
#9246 = CARTESIAN_POINT ( 'NONE',  ( 99.49163138471199375, 123.0000000000000000, -2.452424707819559568 ) ) ;
#9247 = VERTEX_POINT ( 'NONE', #25477 ) ;
#9248 = CARTESIAN_POINT ( 'NONE',  ( 97.99846057881282491, 123.0000000000000142, -0.5333343844930795719 ) ) ;
#9249 = CARTESIAN_POINT ( 'NONE',  ( -5.622872871577873077, 37.67617187499999432, -13.57481594606304753 ) ) ;
#9250 = CARTESIAN_POINT ( 'NONE',  ( 116.8548138422182063, 37.62656250108393863, 5.444914386472304635 ) ) ;
#9251 = ORIENTED_EDGE ( 'NONE', *, *, #11405, .T. ) ;
#9252 = CARTESIAN_POINT ( 'NONE',  ( 94.99999999999995737, 80.00000000000000000, -1.387778780781445676E-14 ) ) ;
#9253 = CARTESIAN_POINT ( 'NONE',  ( 100.9550382616159538, 122.9999999999999716, 2.227387293901141430 ) ) ;
#9254 = CARTESIAN_POINT ( 'NONE',  ( 104.9999999999999574, 82.56250000273119838, 2.071067811865462627 ) ) ;
#9255 = CARTESIAN_POINT ( 'NONE',  ( 97.92893218813452449, 93.31250000000001421, -4.999999999999997335 ) ) ;
#9256 = CARTESIAN_POINT ( 'NONE',  ( 95.54126587499999346, 95.12499999863439371, 1.846868145590722543 ) ) ;
#9257 = CARTESIAN_POINT ( 'NONE',  ( 94.33688103937534208, 114.1144967660473242, -51.20000000000000995 ) ) ;
#9258 = CARTESIAN_POINT ( 'NONE',  ( 78.57481594606304043, 40.55351562499998863, 5.622872871577869525 ) ) ;
#9259 = VERTEX_POINT ( 'NONE', #1822 ) ;
#9260 = CARTESIAN_POINT ( 'NONE',  ( 102.0710678118654329, 5.000000000000018652, 13.68750000000000000 ) ) ;
#9261 = VERTEX_POINT ( 'NONE', #12064 ) ;
#9262 = CARTESIAN_POINT ( 'NONE',  ( -13.14518615778179900, 35.14609375108393152, -5.444914386472297529 ) ) ;
#9263 = CARTESIAN_POINT ( 'NONE',  ( 195.0000000000000000, 34.15390625216787157, 13.57481594606304576 ) ) ;
#9264 = CARTESIAN_POINT ( 'NONE',  ( -13.14518615778179722, 34.15390625108393863, -5.444914386472297529 ) ) ;
#9265 = DIRECTION ( 'NONE',  ( 0.000000000000000000, 0.000000000000000000, 1.000000000000000000 ) ) ;
#9266 = CARTESIAN_POINT ( 'NONE',  ( 116.8548138422182205, 37.57695312608393579, 0.000000000000000000 ) ) ;
#9267 = CARTESIAN_POINT ( 'NONE',  ( 9.295050272127047819, 33.90585937608393863, 9.295050272127046043 ) ) ;
#9268 =( BOUNDED_CURVE ( )  B_SPLINE_CURVE ( 2, ( #5654, #17128, #23040 ),
 .UNSPECIFIED., .F., .F. ) 
 B_SPLINE_CURVE_WITH_KNOTS ( ( 3, 3 ),
 ( 0.9375000000000000000, 0.9448586968893691873 ),
 .UNSPECIFIED. ) 
 CURVE ( )  GEOMETRIC_REPRESENTATION_ITEM ( )  RATIONAL_B_SPLINE_CURVE ( ( 1.000000000000000000, 0.9462258450566536361, 0.9684275698016389100 ) ) 
 REPRESENTATION_ITEM ( '' )  );
#9269 = CARTESIAN_POINT ( 'NONE',  ( 105.6631189606246295, 105.8855032339526758, -49.70000000546237828 ) ) ;
#9270 = CARTESIAN_POINT ( 'NONE',  ( 70.62287287157786864, 33.60820312499998863, -13.57481594606304753 ) ) ;
#9271 = CARTESIAN_POINT ( 'NONE',  ( 99.99999999999998579, 91.75000000000000000, 4.999999999999984013 ) ) ;
#9272 = DIRECTION ( 'NONE',  ( 1.000000000000000000, 0.000000000000000000, 0.000000000000000000 ) ) ;
#9273 = CARTESIAN_POINT ( 'NONE',  ( 104.4587341249999781, 1.846868145590750299, 12.25000000136559208 ) ) ;
#9275 = CARTESIAN_POINT ( 'NONE',  ( 99.99999999999998579, 123.7000000021849502, 2.499999999999978684 ) ) ;
#9274 = AXIS2_PLACEMENT_3D ( 'NONE', #19218, #6250, #23501 ) ;
#9276 = CARTESIAN_POINT ( 'NONE',  ( 101.8468681455907046, 4.458734125000016313, 14.12500000136559208 ) ) ;
#9277 = CARTESIAN_POINT ( 'NONE',  ( 104.9952793366501851, 103.1245878333314323, -46.42500000273119554 ) ) ;
#9278 = CARTESIAN_POINT ( 'NONE',  ( 103.1528011352953484, 91.43749999863440792, 3.152801135295352886 ) ) ;
#9279 = CARTESIAN_POINT ( 'NONE',  ( 91.91746824999997045, 107.3738262389971680, -51.52499999726882152 ) ) ;
#9280 = CARTESIAN_POINT ( 'NONE',  ( 2.414731522848535132E-15, 36.98164062608393721, 13.14518615778179544 ) ) ;
#9281 = VERTEX_POINT ( 'NONE', #20789 ) ;
#9282 = CYLINDRICAL_SURFACE ( 'NONE', #23658, 13.57481594606304398 ) ;
#9283 = CARTESIAN_POINT ( 'NONE',  ( 95.00000000000000000, 91.56249999999998579, 2.071067811865463959 ) ) ;
#9284 = CARTESIAN_POINT ( 'NONE',  ( 84.99999999999998579, 97.00000000000000000, -13.00000000000000355 ) ) ;
#9285 = CARTESIAN_POINT ( 'NONE',  ( 181.8548138422181921, 35.04687500108393294, 5.444914386472304635 ) ) ;
#9286 = EDGE_LOOP ( 'NONE', ( #27974, #19573, #20621, #27720 ) ) ;
#9287 = CARTESIAN_POINT ( 'NONE',  ( 203.2685973283972771, 50.00000000054347993, -10.78867689283658216 ) ) ;
#9288 = CARTESIAN_POINT ( 'NONE',  ( 98.15313185440925281, -4.458734124999987891, 12.87500000136559208 ) ) ;
#9289 = ORIENTED_EDGE ( 'NONE', *, *, #17160, .T. ) ;
#9290 = CARTESIAN_POINT ( 'NONE',  ( 99.99999999999998579, 117.3602355696678501, -46.50000000000001421 ) ) ;
#9291 = CARTESIAN_POINT ( 'NONE',  ( -9.295050272127044266, 36.68398437608392726, 9.295050272127047819 ) ) ;
#9292 = DIRECTION ( 'NONE',  ( -5.782411586589357392E-17, 0.000000000000000000, -1.000000000000000000 ) ) ;
#9293 = CARTESIAN_POINT ( 'NONE',  ( 124.5550856135277087, 37.22968750108393721, -13.14518615778179900 ) ) ;
#9294 = CARTESIAN_POINT ( 'NONE',  ( 99.99999999999995737, 82.87500000273119838, -5.000000000000018652 ) ) ;
#9295 = CARTESIAN_POINT ( 'NONE',  ( -13.14518615778179544, 34.99726562608393721, 0.000000000000000000 ) ) ;
#9296 = ADVANCED_FACE ( 'NONE', ( #27489 ), #10487, .T. ) ;
#9297 = CARTESIAN_POINT ( 'NONE',  ( 103.5355339059327235, 93.99999999726881583, -3.535533905932738197 ) ) ;
#9298 =( BOUNDED_SURFACE ( )  B_SPLINE_SURFACE ( 1, 2, ( 
 ( #25211, #5699, #14366, #11945, #3557, #24791, #15940, #20943, #5419, #12214, #9392, #7390, #14089, #27085, #16376, #16083, #26800, #7250, #5564, #24656, #14227, #13939, #3409, #5129, #13796, #22519, #20381, #866, #9539, #22665, #3135, #11805, #20528, #25624, #8518, #3973, #12360, #8233, #14913, #23221, #19067, #21217, #21492, #23633, #10219, #27912, #25353, #1840, #12905, #18930, #1973, #5969, #19348, #10641, #5836, #12490, #4245, #1425, #6106, #18796, #6244, #10084, #14638, #3697, #4110, #23356, #1701, #17058, #8098, #27503, #3829, #14504, #16924, #25762, #27775, #16792, #7958, #10359, #14773, #25491, #28051, #17203, #25908, #6378, #23493, #12776, #12633, #16658, #21078, #21360, #15052, #23769, #27638, #10503, #19210, #8374, #1567, #24475, #2111, #19767, #11339, #4672, #10920, #22060, #24330, #2400, #13334, #6935, #15478, #11057, #22199, #9080, #6649, #539, #17626, #9222, #24193, #4387, #250, #15629, #15190, #8936, #26332, #15335, #23907, #6514, #20060, #13045, #2535, #15767, #21779, #10778, #6793, #17914, #11198, #26625, #17484, #2678, #7072, #13186, #2258, #19630, #13475, #19915, #111, #398, #17775, #21924, #8794, #26479, #4814, #4959, #26183, #21635, #24051, #17347, #4526, #19490, #28188, #8656, #26044, #7355, #25040, #18346, #11905, #14189, #972, #18488, #27197, #16048, #13621, #9780, #3100, #22908, #26765, #16340, #5097, #24619, #5381, #11766, #5238, #9498, #2949 ),
 ( #16194, #3370, #12041, #11620, #24756, #7209, #20765, #13760, #5522, #20490, #9641, #7648, #14050, #1250, #2813, #22343, #9912, #18627, #13903, #7499, #27330, #22630, #7789, #27050, #16476, #25171, #11482, #20199, #24901, #20345, #18199, #22771, #3237, #20629, #22484, #684, #1113, #15902, #9359, #18052, #832, #26909, #19026, #21178, #6070, #27738, #12452, #21318, #8479, #12593, #3660, #17169, #25587, #5661, #10465, #14877, #14324, #12177, #18888, #8198, #10319, #21460, #23184, #8337, #27875, #10179, #25454, #23045, #3793, #16888, #18761, #6207, #23456, #20907, #1659, #1800, #17021, #12736, #25724, #14736, #1938, #1389, #3934, #19173, #23592, #23320, #4074, #10607, #19314, #28015, #3518, #10050, #27465, #7922, #16753, #16619, #25311, #5800, #14466, #5934, #12321, #27598, #8059, #21042, #1527, #14602, #4633, #24015, #9185, #2497, #6899, #504, #4209, #10884, #11017, #2362, #13436, #15153, #360, #19874, #2220, #17449, #25871, #4493, #19730, #10743, #26440, #15441, #12868, #13150, #13291, #9047, #4775, #17738, #21888, #22163, #21598, #215, #11159, #8902, #15299, #15586, #17590, #26297, #24294, #6758, #2075, #24156, #6340, #8757, #15014, #2641, #11303, #22020, #26148, #20024, #19593, #76, #4351, #23736, #19454, #28152, #8619, #6615, #17307, #26007, #6478, #23872, #13005, #21745, #9320, #647, #9606, #7321, #9461, #13726, #7173, #22874, #18308, #20165, #3339, #25004, #5062 ) ),
 .UNSPECIFIED., .F., .F., .F. ) 
 B_SPLINE_SURFACE_WITH_KNOTS ( ( 2, 2 ),
 ( 3, 2, 2, 2, 2, 2, 2, 2, 2, 2, 2, 2, 2, 2, 2, 2, 2, 2, 2, 2, 2, 2, 2, 2, 2, 2, 2, 2, 2, 2, 2, 2, 2, 2, 2, 2, 2, 2, 2, 2, 2, 2, 2, 2, 2, 2, 2, 2, 2, 2, 2, 2, 2, 2, 2, 2, 2, 2, 2, 2, 2, 2, 2, 2, 2, 2, 2, 2, 2, 2, 2, 2, 2, 2, 2, 2, 2, 2, 2, 2, 2, 2, 2, 2, 2, 2, 2, 2, 2, 2, 2, 3 ),
 ( 0.000000000000000000, 1.000000000000000000 ),
 ( 0.000000000000000000, 0.01041666666666666609, 0.02083333333333333218, 0.03125000000000000000, 0.04166666666666666435, 0.05208333333333333565, 0.06250000000000000000, 0.07291666666666667129, 0.08333333333333332871, 0.09375000000000000000, 0.1041666666666666713, 0.1145833333333333287, 0.1250000000000000000, 0.1354166666666666574, 0.1458333333333333426, 0.1562500000000000000, 0.1666666666666666574, 0.1770833333333333426, 0.1875000000000000000, 0.1979166666666666574, 0.2083333333333333426, 0.2187500000000000000, 0.2291666666666666574, 0.2395833333333333426, 0.2500000000000000000, 0.2604166666666666852, 0.2708333333333333148, 0.2812500000000000000, 0.2916666666666666852, 0.3020833333333333148, 0.3125000000000000000, 0.3229166666666666852, 0.3333333333333333148, 0.3437500000000000000, 0.3541666666666666852, 0.3645833333333333148, 0.3750000000000000000, 0.3854166666666666852, 0.3958333333333333148, 0.4062500000000000000, 0.4166666666666666852, 0.4270833333333333148, 0.4375000000000000000, 0.4479166666666666852, 0.4583333333333333148, 0.4687500000000000000, 0.4791666666666666852, 0.4895833333333333148, 0.5000000000000000000, 0.5104166666666666297, 0.5208333333333333703, 0.5312500000000000000, 0.5416666666666666297, 0.5520833333333333703, 0.5625000000000000000, 0.5729166666666666297, 0.5833333333333333703, 0.5937500000000000000, 0.6041666666666666297, 0.6145833333333333703, 0.6250000000000000000, 0.6354166666666666297, 0.6458333333333333703, 0.6562500000000000000, 0.6666666666666666297, 0.6770833333333333703, 0.6875000000000000000, 0.6979166666666666297, 0.7083333333333333703, 0.7187500000000000000, 0.7291666666666666297, 0.7395833333333333703, 0.7500000000000000000, 0.7604166666666666297, 0.7708333333333333703, 0.7812500000000000000, 0.7916666666666666297, 0.8020833333333333703, 0.8125000000000000000, 0.8229166666666666297, 0.8333333333333333703, 0.8437500000000000000, 0.8541666666666666297, 0.8645833333333333703, 0.8750000000000000000, 0.8854166666666666297, 0.8958333333333333703, 0.9062500000000000000, 0.9166666666666666297, 0.9270833333333333703, 0.9375000000000000000, 0.9448586970929392370 ),
 .UNSPECIFIED. ) 
 GEOMETRIC_REPRESENTATION_ITEM ( )  RATIONAL_B_SPLINE_SURFACE ( (
 ( 1.000000000000000000, 0.9238795325112867385, 1.000000000000000000, 0.9238795325112867385, 1.000000000000000000, 0.9238795325112867385, 1.000000000000000000, 0.9238795325112867385, 1.000000000000000000, 0.9238795325112867385, 1.000000000000000000, 0.9238795325112867385, 1.000000000000000000, 0.9238795325112867385, 1.000000000000000000, 0.9238795325112867385, 1.000000000000000000, 0.9238795325112867385, 1.000000000000000000, 0.9238795325112867385, 1.000000000000000000, 0.9238795325112867385, 1.000000000000000000, 0.9238795325112867385, 1.000000000000000000, 0.9238795325112867385, 1.000000000000000000, 0.9238795325112867385, 1.000000000000000000, 0.9238795325112867385, 1.000000000000000000, 0.9238795325112867385, 1.000000000000000000, 0.9238795325112867385, 1.000000000000000000, 0.9238795325112867385, 1.000000000000000000, 0.9238795325112867385, 1.000000000000000000, 0.9238795325112867385, 1.000000000000000000, 0.9238795325112867385, 1.000000000000000000, 0.9238795325112867385, 1.000000000000000000, 0.9238795325112867385, 1.000000000000000000, 0.9238795325112867385, 1.000000000000000000, 0.9238795325112867385, 1.000000000000000000, 0.9238795325112867385, 1.000000000000000000, 0.9238795325112867385, 1.000000000000000000, 0.9238795325112867385, 1.000000000000000000, 0.9238795325112867385, 1.000000000000000000, 0.9238795325112867385, 1.000000000000000000, 0.9238795325112867385, 1.000000000000000000, 0.9238795325112867385, 1.000000000000000000, 0.9238795325112867385, 1.000000000000000000, 0.9238795325112867385, 1.000000000000000000, 0.9238795325112867385, 1.000000000000000000, 0.9238795325112867385, 1.000000000000000000, 0.9238795325112867385, 1.000000000000000000, 0.9238795325112867385, 1.000000000000000000, 0.9238795325112867385, 1.000000000000000000, 0.9238795325112867385, 1.000000000000000000, 0.9238795325112867385, 1.000000000000000000, 0.9238795325112867385, 1.000000000000000000, 0.9238795325112867385, 1.000000000000000000, 0.9238795325112867385, 1.000000000000000000, 0.9238795325112867385, 1.000000000000000000, 0.9238795325112867385, 1.000000000000000000, 0.9238795325112867385, 1.000000000000000000, 0.9238795325112867385, 1.000000000000000000, 0.9238795325112867385, 1.000000000000000000, 0.9238795325112867385, 1.000000000000000000, 0.9238795325112867385, 1.000000000000000000, 0.9238795325112867385, 1.000000000000000000, 0.9238795325112867385, 1.000000000000000000, 0.9238795325112867385, 1.000000000000000000, 0.9238795325112867385, 1.000000000000000000, 0.9238795325112867385, 1.000000000000000000, 0.9238795325112867385, 1.000000000000000000, 0.9238795325112867385, 1.000000000000000000, 0.9238795325112867385, 1.000000000000000000, 0.9238795325112867385, 1.000000000000000000, 0.9238795325112867385, 1.000000000000000000, 0.9238795325112867385, 1.000000000000000000, 0.9238795325112867385, 1.000000000000000000, 0.9238795325112867385, 1.000000000000000000, 0.9238795325112867385, 1.000000000000000000, 0.9238795325112867385, 1.000000000000000000, 0.9238795325112867385, 1.000000000000000000, 0.9238795325112867385, 1.000000000000000000, 0.9238795325112867385, 1.000000000000000000, 0.9238795325112867385, 1.000000000000000000, 0.9238795325112867385, 1.000000000000000000, 0.9238795325112867385, 1.000000000000000000, 0.9238795325112867385, 1.000000000000000000, 0.9238795325112867385, 1.000000000000000000, 0.9238795325112867385, 1.000000000000000000, 0.9238795325112867385, 1.000000000000000000, 0.9238795325112867385, 1.000000000000000000, 0.9238795325112867385, 1.000000000000000000, 0.9238795325112867385, 1.000000000000000000, 0.9238795325112867385, 1.000000000000000000, 0.9238795325112867385, 1.000000000000000000, 0.9238795325112867385, 1.000000000000000000, 0.9238795325112867385, 1.000000000000000000, 0.9238795325112867385, 1.000000000000000000, 0.9238795325112867385, 1.000000000000000000, 0.9238795325112867385, 1.000000000000000000, 0.9238795325112867385, 1.000000000000000000, 0.9238795325112867385, 1.000000000000000000, 0.9238795325112867385, 1.000000000000000000, 0.9238795325112867385, 1.000000000000000000, 0.9462258435690522607, 0.9684275710300105366),
 ( 1.000000000000000000, 0.9238795325112867385, 1.000000000000000000, 0.9238795325112867385, 1.000000000000000000, 0.9238795325112867385, 1.000000000000000000, 0.9238795325112867385, 1.000000000000000000, 0.9238795325112867385, 1.000000000000000000, 0.9238795325112867385, 1.000000000000000000, 0.9238795325112867385, 1.000000000000000000, 0.9238795325112867385, 1.000000000000000000, 0.9238795325112867385, 1.000000000000000000, 0.9238795325112867385, 1.000000000000000000, 0.9238795325112867385, 1.000000000000000000, 0.9238795325112867385, 1.000000000000000000, 0.9238795325112867385, 1.000000000000000000, 0.9238795325112867385, 1.000000000000000000, 0.9238795325112867385, 1.000000000000000000, 0.9238795325112867385, 1.000000000000000000, 0.9238795325112867385, 1.000000000000000000, 0.9238795325112867385, 1.000000000000000000, 0.9238795325112867385, 1.000000000000000000, 0.9238795325112867385, 1.000000000000000000, 0.9238795325112867385, 1.000000000000000000, 0.9238795325112867385, 1.000000000000000000, 0.9238795325112867385, 1.000000000000000000, 0.9238795325112867385, 1.000000000000000000, 0.9238795325112867385, 1.000000000000000000, 0.9238795325112867385, 1.000000000000000000, 0.9238795325112867385, 1.000000000000000000, 0.9238795325112867385, 1.000000000000000000, 0.9238795325112867385, 1.000000000000000000, 0.9238795325112867385, 1.000000000000000000, 0.9238795325112867385, 1.000000000000000000, 0.9238795325112867385, 1.000000000000000000, 0.9238795325112867385, 1.000000000000000000, 0.9238795325112867385, 1.000000000000000000, 0.9238795325112867385, 1.000000000000000000, 0.9238795325112867385, 1.000000000000000000, 0.9238795325112867385, 1.000000000000000000, 0.9238795325112867385, 1.000000000000000000, 0.9238795325112867385, 1.000000000000000000, 0.9238795325112867385, 1.000000000000000000, 0.9238795325112867385, 1.000000000000000000, 0.9238795325112867385, 1.000000000000000000, 0.9238795325112867385, 1.000000000000000000, 0.9238795325112867385, 1.000000000000000000, 0.9238795325112867385, 1.000000000000000000, 0.9238795325112867385, 1.000000000000000000, 0.9238795325112867385, 1.000000000000000000, 0.9238795325112867385, 1.000000000000000000, 0.9238795325112867385, 1.000000000000000000, 0.9238795325112867385, 1.000000000000000000, 0.9238795325112867385, 1.000000000000000000, 0.9238795325112867385, 1.000000000000000000, 0.9238795325112867385, 1.000000000000000000, 0.9238795325112867385, 1.000000000000000000, 0.9238795325112867385, 1.000000000000000000, 0.9238795325112867385, 1.000000000000000000, 0.9238795325112867385, 1.000000000000000000, 0.9238795325112867385, 1.000000000000000000, 0.9238795325112867385, 1.000000000000000000, 0.9238795325112867385, 1.000000000000000000, 0.9238795325112867385, 1.000000000000000000, 0.9238795325112867385, 1.000000000000000000, 0.9238795325112867385, 1.000000000000000000, 0.9238795325112867385, 1.000000000000000000, 0.9238795325112867385, 1.000000000000000000, 0.9238795325112867385, 1.000000000000000000, 0.9238795325112867385, 1.000000000000000000, 0.9238795325112867385, 1.000000000000000000, 0.9238795325112867385, 1.000000000000000000, 0.9238795325112867385, 1.000000000000000000, 0.9238795325112867385, 1.000000000000000000, 0.9238795325112867385, 1.000000000000000000, 0.9238795325112867385, 1.000000000000000000, 0.9238795325112867385, 1.000000000000000000, 0.9238795325112867385, 1.000000000000000000, 0.9238795325112867385, 1.000000000000000000, 0.9238795325112867385, 1.000000000000000000, 0.9238795325112867385, 1.000000000000000000, 0.9238795325112867385, 1.000000000000000000, 0.9238795325112867385, 1.000000000000000000, 0.9238795325112867385, 1.000000000000000000, 0.9238795325112867385, 1.000000000000000000, 0.9238795325112867385, 1.000000000000000000, 0.9238795325112867385, 1.000000000000000000, 0.9238795325112867385, 1.000000000000000000, 0.9238795325112867385, 1.000000000000000000, 0.9238795325112867385, 1.000000000000000000, 0.9238795325112867385, 1.000000000000000000, 0.9238795325112867385, 1.000000000000000000, 0.9238795325112867385, 1.000000000000000000, 0.9462258435690522607, 0.9684275710300105366) ) ) 
 REPRESENTATION_ITEM ( '' )  SURFACE ( )  );
#9299 = CARTESIAN_POINT ( 'NONE',  ( 78.14518615778179367, 37.97382812608393721, -1.609821015232357215E-15 ) ) ;
#9300 = CARTESIAN_POINT ( 'NONE',  ( 64.60300058535341350, 51.45716825712325715, -15.00000000000000178 ) ) ;
#9301 = CARTESIAN_POINT ( 'NONE',  ( 91.91746824999999887, 110.0000000000000000, -53.37500000273119838 ) ) ;
#9302 = CARTESIAN_POINT ( 'NONE',  ( 198.7556381558599696, 31.78804748261757140, -13.14518615778179367 ) ) ;
#9303 = FACE_OUTER_BOUND ( 'NONE', #27849, .T. ) ;
#9304 = CARTESIAN_POINT ( 'NONE',  ( 13.14518615778179900, 35.64218750108393152, -5.444914386472297529 ) ) ;
#9305 = CARTESIAN_POINT ( 'NONE',  ( 101.8468681455907046, -4.458734124999987891, 9.000000001365592084 ) ) ;
#9306 = EDGE_CURVE ( 'NONE', #3132, #24544, #15999, .T. ) ;
#9307 = CARTESIAN_POINT ( 'NONE',  ( 74.29505027212704249, 37.67617187608393436, 9.295050272127046043 ) ) ;
#9308 = CARTESIAN_POINT ( 'NONE',  ( 107.0000000000000142, 110.0000000000000000, -55.00000000000000711 ) ) ;
#9309 = EDGE_CURVE ( 'NONE', #4613, #18339, #541, .T. ) ;
#9310 = CARTESIAN_POINT ( 'NONE',  ( 5.444914386472297529, 38.12265625108393863, -13.14518615778179722 ) ) ;
#9311 = CARTESIAN_POINT ( 'NONE',  ( 104.4587341249999923, 91.62499999863439371, -1.846868145590737198 ) ) ;
#9312 = CARTESIAN_POINT ( 'NONE',  ( 181.8548138422182205, 39.16445312608393436, 0.000000000000000000 ) ) ;
#9313 = CARTESIAN_POINT ( 'NONE',  ( 106.5389055433250860, 114.7507929638356785, -50.67499999726882010 ) ) ;
#9314 = ORIENTED_EDGE ( 'NONE', *, *, #13713, .F. ) ;
#9315 = CIRCLE ( 'NONE', #18878, 5.000000000000004441 ) ;
#9316 = CARTESIAN_POINT ( 'NONE',  ( 3.878385297391210518, 32.03609435653363136, -13.57481594606304576 ) ) ;
#9317 = CARTESIAN_POINT ( 'NONE',  ( 9.295050272127046043, 33.11210937608393579, -9.295050272127046043 ) ) ;
#9318 = ORIENTED_EDGE ( 'NONE', *, *, #6735, .T. ) ;
#9319 = CARTESIAN_POINT ( 'NONE',  ( 116.8548138422182063, 33.55859375108393294, -5.444914386472297529 ) ) ;
#9320 = CARTESIAN_POINT ( 'NONE',  ( 74.29505027212704249, 32.11992187608393579, 9.295050272127046043 ) ) ;
#9321 = EDGE_CURVE ( 'NONE', #16572, #6030, #8219, .T. ) ;
#9322 = CARTESIAN_POINT ( 'NONE',  ( 204.2950502721270425, 33.31054687608394005, -9.295050272127046043 ) ) ;
#9323 = ORIENTED_EDGE ( 'NONE', *, *, #80, .F. ) ;
#9324 = CARTESIAN_POINT ( 'NONE',  ( 94.99999999999995737, 1.387778780781445676E-14, 13.00000000000000000 ) ) ;
#9325 = CARTESIAN_POINT ( 'NONE',  ( -0.3286002765684034599, 53.49358765998907472, -14.99999999999999822 ) ) ;
#9326 = CARTESIAN_POINT ( 'NONE',  ( 130.0000000000000000, -7.395377635281828788, -13.57481594606305997 ) ) ;
#9327 = DIRECTION ( 'NONE',  ( 0.000000000000000000, 1.000000000000000000, 0.000000000000000000 ) ) ;
#9328 = CARTESIAN_POINT ( 'NONE',  ( 91.91746824999998466, 112.6261737610028320, -47.22500000273119269 ) ) ;
#9329 = CARTESIAN_POINT ( 'NONE',  ( 65.00000000000000000, -7.395377635281828788, -7.517135062566165128E-15 ) ) ;
#9330 = CARTESIAN_POINT ( 'NONE',  ( -13.57481594606304753, 33.90585937716787868, -5.622872871577872189 ) ) ;
#9331 = CARTESIAN_POINT ( 'NONE',  ( 181.8548138422182205, 40.75195312608393294, 0.000000000000000000 ) ) ;
#9332 = EDGE_CURVE ( 'NONE', #24121, #1428, #17661, .T. ) ;
#9333 = AXIS2_PLACEMENT_3D ( 'NONE', #24635, #11783, #27485 ) ;
#9334 = ORIENTED_EDGE ( 'NONE', *, *, #484, .F. ) ;
#9335 = CARTESIAN_POINT ( 'NONE',  ( 96.84719886470459471, 3.152801135295383084, 5.312500001365592972 ) ) ;
#9336 = ORIENTED_EDGE ( 'NONE', *, *, #25348, .F. ) ;
#9337 = CARTESIAN_POINT ( 'NONE',  ( -12.85950995607747949, 36.00000000000000711, -3.245221471867173246 ) ) ;
#9338 = CARTESIAN_POINT ( 'NONE',  ( 104.4587341249999781, -1.846868145590721655, 9.875000001365593860 ) ) ;
#9339 = EDGE_CURVE ( 'NONE', #11544, #20557, #18649, .T. ) ;
#9340 = CARTESIAN_POINT ( 'NONE',  ( 5.444914386472297529, 34.74921875108394431, -13.14518615778179900 ) ) ;
#9341 = CARTESIAN_POINT ( 'NONE',  ( -10.78684676818434518, 35.99999999999998579, 7.561388982944274417 ) ) ;
#9342 = CARTESIAN_POINT ( 'NONE',  ( 104.9999999999999858, 95.87499999726881583, -6.938893903907228378E-15 ) ) ;
#9343 = CARTESIAN_POINT ( 'NONE',  ( 103.1528011352953484, 92.18749999863440792, 3.152801135295352886 ) ) ;
#9344 =( BOUNDED_CURVE ( )  B_SPLINE_CURVE ( 2, ( #4830, #11492, #13489, #22210, #11350, #551, #5108, #9233, #17925 ),
 .UNSPECIFIED., .F., .T. ) 
 B_SPLINE_CURVE_WITH_KNOTS ( ( 3, 2, 2, 2, 3 ),
 ( 0.6500000000000005773, 0.6750000000000005995, 0.7000000000000006217, 0.7250000000000006439, 0.7500000000000006661 ),
 .UNSPECIFIED. ) 
 CURVE ( )  GEOMETRIC_REPRESENTATION_ITEM ( )  RATIONAL_B_SPLINE_CURVE ( ( 0.9999999999999983347, 0.9238795325112884038, 1.000000000000000000, 0.9238795325112867385, 1.000000000000000000, 0.9238795325112867385, 1.000000000000000000, 0.9238795325112847401, 1.000000000000001998 ) ) 
 REPRESENTATION_ITEM ( '' )  );
#9345 = CARTESIAN_POINT ( 'NONE',  ( 97.50236033167492167, 117.6869444889999841, -47.52500000273119696 ) ) ;
#9346 = CARTESIAN_POINT ( 'NONE',  ( -9.295050272127044266, 37.47773437608393010, 9.295050272127047819 ) ) ;
#9347 = ADVANCED_FACE ( 'NONE', ( #16504 ), #25198, .T. ) ;
#9348 = VECTOR ( 'NONE', #5575, 1000.000000000000000 ) ;
#9349 = AXIS2_PLACEMENT_3D ( 'NONE', #3723, #21243, #23381 ) ;
#9350 = CARTESIAN_POINT ( 'NONE',  ( 2.493653234604083739E-15, 34.94765625216787441, 13.57481594606304576 ) ) ;
#9351 = CARTESIAN_POINT ( 'NONE',  ( 143.5748159460630688, 40.60312499999999858, -1.662435489736055892E-15 ) ) ;
#9352 = CARTESIAN_POINT ( 'NONE',  ( 116.4251840539369596, 34.64999999999999147, 0.000000000000000000 ) ) ;
#9353 = EDGE_CURVE ( 'NONE', #21949, #26975, #14001, .T. ) ;
#9354 = ORIENTED_EDGE ( 'NONE', *, *, #21989, .T. ) ;
#9355 = CARTESIAN_POINT ( 'NONE',  ( -13.14518615778179900, 34.35234375108393579, -5.444914386472297529 ) ) ;
#9356 = CARTESIAN_POINT ( 'NONE',  ( -9.598844408820458085, 33.85625000216787583, -9.598844408820458085 ) ) ;
#9357 = CARTESIAN_POINT ( 'NONE',  ( 99.99999999999995737, -4.999999999999990230, 11.37500000273118594 ) ) ;
#9358 = CARTESIAN_POINT ( 'NONE',  ( 139.2950502721270425, 34.69960937608393436, -9.295050272127046043 ) ) ;
#9359 = CARTESIAN_POINT ( 'NONE',  ( 74.29505027212704249, 38.66835937608393436, -9.295050272127046043 ) ) ;
#9360 = CARTESIAN_POINT ( 'NONE',  ( 9.598844408820456309, 37.62656250216787157, -9.598844408820458085 ) ) ;
#9361 = CARTESIAN_POINT ( 'NONE',  ( -9.598844408820458085, 33.85625000216787583, -9.598844408820458085 ) ) ;
#9362 = CARTESIAN_POINT ( 'NONE',  ( 97.92893218813451028, -4.999999999999989342, 2.187499999999998224 ) ) ;
#9363 = CARTESIAN_POINT ( 'NONE',  ( 108.0825317499999869, 112.6261737610028320, -50.77499999726882152 ) ) ;
#9364 = CARTESIAN_POINT ( 'NONE',  ( -13.57481594606304753, 40.25585937716787299, -5.622872871577873077 ) ) ;
#9365 = CARTESIAN_POINT ( 'NONE',  ( 204.2950502721270425, 35.29492187608393294, 9.295050272127046043 ) ) ;
#9366 = CARTESIAN_POINT ( 'NONE',  ( 185.8198241863519797, 55.00000000000000000, -10.00000000000000000 ) ) ;
#9367 = CARTESIAN_POINT ( 'NONE',  ( 99.14382582708707048, 123.9000000010924794, 2.066987299999979211 ) ) ;
#9368 = CARTESIAN_POINT ( 'NONE',  ( 92.99999999999998579, 110.0000000000000000, -50.49999999453763877 ) ) ;
#9369 = CARTESIAN_POINT ( 'NONE',  ( -13.57481594606304398, 35.49335937499999005, 5.622872871577880183 ) ) ;
#9370 = DIRECTION ( 'NONE',  ( -0.000000000000000000, -0.000000000000000000, -1.000000000000000000 ) ) ;
#9371 = CARTESIAN_POINT ( 'NONE',  ( -5.622872871577873077, 33.70742187500000142, -13.57481594606304753 ) ) ;
#9372 = CARTESIAN_POINT ( 'NONE',  ( 94.33688103937537051, 114.1144967660473242, -54.20000000000000284 ) ) ;
#9373 = CARTESIAN_POINT ( 'NONE',  ( 13.14518615778179544, 33.21132812608393436, -1.609821015232357215E-15 ) ) ;
#9374 = CARTESIAN_POINT ( 'NONE',  ( 5.444914386472302859, 36.83281250108392868, 13.14518615778179189 ) ) ;
#9375 = CARTESIAN_POINT ( 'NONE',  ( 13.14518615778179722, 34.65000000108393152, -5.444914386472297529 ) ) ;
#9376 = CARTESIAN_POINT ( 'NONE',  ( -9.598844408820454532, 34.84843750216787583, 9.598844408820459861 ) ) ;
#9377 = CARTESIAN_POINT ( 'NONE',  ( -9.598844408820454532, 38.02343750216788010, 9.598844408820459861 ) ) ;
#9378 = CARTESIAN_POINT ( 'NONE',  ( 103.1528011352953342, 83.81250000136560629, 3.152801135295355106 ) ) ;
#9379 = CARTESIAN_POINT ( 'NONE',  ( 51.85481384221820633, 32.61601562608393579, 0.000000000000000000 ) ) ;
#9380 = CARTESIAN_POINT ( 'NONE',  ( 108.0825317500000011, 107.3738262389971538, -52.47500000273118559 ) ) ;
#9381 = CARTESIAN_POINT ( 'NONE',  ( 102.4515117831381730, 123.0000000000000000, -0.5701068363804095984 ) ) ;
#9382 =( BOUNDED_SURFACE ( )  B_SPLINE_SURFACE ( 1, 2, ( 
 ( #26752, #20753, #14177, #7911, #27449, #25157, #5648, #9901, #12308, #3359, #12030, #27319, #16605, #14453, #16463, #18613, #1238, #25298, #23170, #7775, #12165, #14310, #23032, #20893, #3504, #1376, #16328, #10037, #18749, #5786, #5510, #25027, #3645, #22895, #6665, #26350, #2127, #26494, #23649, #13058, #19643, #12920, #15066, #6809, #22077, #26059, #4688, #21795, #15350, #8531, #1988, #17501, #15205, #19786, #26201, #268, #23925, #17792, #4124, #15497, #25922, #24209, #2274, #10933, #8953, #24066, #13348, #12789, #21938, #17643, #10654, #2554, #11214, #21507, #4542, #19930, #13204, #14929, #2415, #6527, #28065, #19362, #17217, #4404, #413, #126, #11074, #6396, #8811, #10792, #23783, #9097, #4259, #21652, #19506, #20429, #8671, #17363, #13919, #11639, #26784, #15787, #7229, #7519, #990, #4975, #11355, #18069, #847, #5112, #11784, #15920, #20507, #24636, #13640, #16066, #13777, #11925, #2964, #11498, #22788, #24490, #27068, #9799, #9238, #24915, #9658, #16214, #18505, #22355, #18219, #5399, #15646, #18360, #14068, #2830, #22499, #20362, #9520, #20215, #6951, #24344, #20647, #3258, #1130, #700, #26928, #7371, #556, #4835, #13496, #22647, #9373, #22216, #24774, #2694, #20078, #17930, #26640, #7087, #5255, #3116, #12472, #20785, #16639, #14487, #3389, #1681, #8216, #1266, #14620, #21198, #9930, #19048, #23337, #27486, #10340, #27756, #16906, #25603, #3540, #21340, #27621 ),
 ( #7942, #23204, #14755, #6088, #25474, #23475, #3812, #10067, #3954, #21060, #25193, #12060, #25331, #18645, #5817, #5544, #18779, #1818, #14208, #7808, #12613, #27211, #27350, #10484, #7666, #12343, #16358, #16498, #25058, #22928, #3679, #5680, #14347, #23062, #12197, #20925, #1408, #8079, #1549, #10201, #18911, #16774, #5953, #6663, #11073, #11353, #15644, #26492, #266, #26638, #12918, #13493, #26348, #15203, #19641, #8950, #13346, #28202, #4401, #10790, #9095, #411, #4540, #13202, #2272, #15065, #26057, #6525, #17499, #6949, #2692, #15348, #124, #21792, #24342, #554, #8809, #6807, #23923, #19783, #15495, #13056, #24206, #17928, #4686, #26198, #21936, #21650, #23780, #10931, #4833, #22075, #22213, #24063, #4257, #2124, #2413, #17641, #2552, #11211, #20075, #9236, #19928, #19504, #17789, #8669, #17361, #22353, #9656, #7369, #11923, #18358, #20645, #16064, #9927, #15783, #7664, #18066, #18504, #13918, #3114, #1128, #7517, #27210, #24488, #14066, #9797, #2828, #5541, #16356, #13638, #27066, #25055, #16211, #18642, #24914, #18216, #20212, #11496, #698, #24772, #14204, #26926, #5397, #26782, #7085, #845, #9371, #7227, #5253, #11782, #22925, #22645, #24634, #3386, #12056, #15918, #22786, #20782, #3256, #4973, #1264, #20505, #5110, #13775, #22497, #988, #2962, #11637, #20359, #9518, #27347, #21058, #12193, #5677, #10197, #23334, #25741, #8075, #16635, #25471, #1679, #27483 ) ),
 .UNSPECIFIED., .F., .F., .T. ) 
 B_SPLINE_SURFACE_WITH_KNOTS ( ( 2, 2 ),
 ( 3, 2, 2, 2, 2, 2, 2, 2, 2, 2, 2, 2, 2, 2, 2, 2, 2, 2, 2, 2, 2, 2, 2, 2, 2, 2, 2, 2, 2, 2, 2, 2, 2, 2, 2, 2, 2, 2, 2, 2, 2, 2, 2, 2, 2, 2, 2, 2, 2, 2, 2, 2, 2, 2, 2, 2, 2, 2, 2, 2, 2, 2, 2, 2, 2, 2, 2, 2, 2, 2, 2, 2, 2, 2, 2, 2, 2, 2, 2, 2, 2, 2, 2, 2, 2, 2, 2, 2, 2, 2, 2, 3 ),
 ( 0.000000000000000000, 1.000000000000000000 ),
 ( 0.000000000000000000, 0.01041666666666666609, 0.02083333333333333218, 0.03125000000000000000, 0.04166666666666666435, 0.05208333333333333565, 0.06250000000000000000, 0.07291666666666667129, 0.08333333333333332871, 0.09375000000000000000, 0.1041666666666666713, 0.1145833333333333287, 0.1250000000000000000, 0.1354166666666666574, 0.1458333333333333426, 0.1562500000000000000, 0.1666666666666666574, 0.1770833333333333426, 0.1875000000000000000, 0.1979166666666666574, 0.2083333333333333426, 0.2187500000000000000, 0.2291666666666666574, 0.2395833333333333426, 0.2500000000000000000, 0.2604166666666666852, 0.2708333333333333148, 0.2812500000000000000, 0.2916666666666666852, 0.3020833333333333148, 0.3125000000000000000, 0.3229166666666666852, 0.3333333333333333148, 0.3437500000000000000, 0.3541666666666666852, 0.3645833333333333148, 0.3750000000000000000, 0.3854166666666666852, 0.3958333333333333148, 0.4062500000000000000, 0.4166666666666666852, 0.4270833333333333148, 0.4375000000000000000, 0.4479166666666666852, 0.4583333333333333148, 0.4687500000000000000, 0.4791666666666666852, 0.4895833333333333148, 0.5000000000000000000, 0.5104166666666666297, 0.5208333333333333703, 0.5312500000000000000, 0.5416666666666666297, 0.5520833333333333703, 0.5625000000000000000, 0.5729166666666666297, 0.5833333333333333703, 0.5937500000000000000, 0.6041666666666666297, 0.6145833333333333703, 0.6250000000000000000, 0.6354166666666666297, 0.6458333333333333703, 0.6562500000000000000, 0.6666666666666666297, 0.6770833333333333703, 0.6875000000000000000, 0.6979166666666666297, 0.7083333333333333703, 0.7187500000000000000, 0.7291666666666666297, 0.7395833333333333703, 0.7500000000000000000, 0.7604166666666666297, 0.7708333333333333703, 0.7812500000000000000, 0.7916666666666666297, 0.8020833333333333703, 0.8125000000000000000, 0.8229166666666666297, 0.8333333333333333703, 0.8437500000000000000, 0.8541666666666666297, 0.8645833333333333703, 0.8750000000000000000, 0.8854166666666666297, 0.8958333333333333703, 0.9062500000000000000, 0.9166666666666666297, 0.9270833333333333703, 0.9375000000000000000, 0.9448586968893691873 ),
 .UNSPECIFIED. ) 
 GEOMETRIC_REPRESENTATION_ITEM ( )  RATIONAL_B_SPLINE_SURFACE ( (
 ( 1.000000000000000000, 0.9238795325112867385, 1.000000000000000000, 0.9238795325112867385, 1.000000000000000000, 0.9238795325112867385, 1.000000000000000000, 0.9238795325112867385, 1.000000000000000000, 0.9238795325112867385, 1.000000000000000000, 0.9238795325112867385, 1.000000000000000000, 0.9238795325112867385, 1.000000000000000000, 0.9238795325112867385, 1.000000000000000000, 0.9238795325112867385, 1.000000000000000000, 0.9238795325112867385, 1.000000000000000000, 0.9238795325112867385, 1.000000000000000000, 0.9238795325112867385, 1.000000000000000000, 0.9238795325112867385, 1.000000000000000000, 0.9238795325112867385, 1.000000000000000000, 0.9238795325112867385, 1.000000000000000000, 0.9238795325112867385, 1.000000000000000000, 0.9238795325112867385, 1.000000000000000000, 0.9238795325112867385, 1.000000000000000000, 0.9238795325112867385, 1.000000000000000000, 0.9238795325112867385, 1.000000000000000000, 0.9238795325112867385, 1.000000000000000000, 0.9238795325112867385, 1.000000000000000000, 0.9238795325112867385, 1.000000000000000000, 0.9238795325112867385, 1.000000000000000000, 0.9238795325112867385, 1.000000000000000000, 0.9238795325112867385, 1.000000000000000000, 0.9238795325112867385, 1.000000000000000000, 0.9238795325112867385, 1.000000000000000000, 0.9238795325112867385, 1.000000000000000000, 0.9238795325112867385, 1.000000000000000000, 0.9238795325112867385, 1.000000000000000000, 0.9238795325112867385, 1.000000000000000000, 0.9238795325112867385, 1.000000000000000000, 0.9238795325112867385, 1.000000000000000000, 0.9238795325112867385, 1.000000000000000000, 0.9238795325112867385, 1.000000000000000000, 0.9238795325112867385, 1.000000000000000000, 0.9238795325112867385, 1.000000000000000000, 0.9238795325112867385, 1.000000000000000000, 0.9238795325112867385, 1.000000000000000000, 0.9238795325112867385, 1.000000000000000000, 0.9238795325112867385, 1.000000000000000000, 0.9238795325112867385, 1.000000000000000000, 0.9238795325112867385, 1.000000000000000000, 0.9238795325112867385, 1.000000000000000000, 0.9238795325112867385, 1.000000000000000000, 0.9238795325112867385, 1.000000000000000000, 0.9238795325112867385, 1.000000000000000000, 0.9238795325112867385, 1.000000000000000000, 0.9238795325112867385, 1.000000000000000000, 0.9238795325112867385, 1.000000000000000000, 0.9238795325112867385, 1.000000000000000000, 0.9238795325112867385, 1.000000000000000000, 0.9238795325112867385, 1.000000000000000000, 0.9238795325112867385, 1.000000000000000000, 0.9238795325112867385, 1.000000000000000000, 0.9238795325112867385, 1.000000000000000000, 0.9238795325112867385, 1.000000000000000000, 0.9238795325112867385, 1.000000000000000000, 0.9238795325112867385, 1.000000000000000000, 0.9238795325112867385, 1.000000000000000000, 0.9238795325112867385, 1.000000000000000000, 0.9238795325112867385, 1.000000000000000000, 0.9238795325112867385, 1.000000000000000000, 0.9238795325112867385, 1.000000000000000000, 0.9238795325112867385, 1.000000000000000000, 0.9238795325112867385, 1.000000000000000000, 0.9238795325112867385, 1.000000000000000000, 0.9238795325112867385, 1.000000000000000000, 0.9238795325112867385, 1.000000000000000000, 0.9238795325112867385, 1.000000000000000000, 0.9238795325112867385, 1.000000000000000000, 0.9238795325112867385, 1.000000000000000000, 0.9238795325112867385, 1.000000000000000000, 0.9238795325112867385, 1.000000000000000000, 0.9238795325112867385, 1.000000000000000000, 0.9238795325112867385, 1.000000000000000000, 0.9238795325112867385, 1.000000000000000000, 0.9238795325112867385, 1.000000000000000000, 0.9238795325112867385, 1.000000000000000000, 0.9238795325112867385, 1.000000000000000000, 0.9238795325112867385, 1.000000000000000000, 0.9238795325112867385, 1.000000000000000000, 0.9238795325112867385, 1.000000000000000000, 0.9238795325112867385, 1.000000000000000000, 0.9238795325112867385, 1.000000000000000000, 0.9238795325112867385, 1.000000000000000000, 0.9238795325112867385, 1.000000000000000000, 0.9238795325112867385, 1.000000000000000000, 0.9238795325112867385, 1.000000000000000000, 0.9462258450566536361, 0.9684275698016389100),
 ( 1.000000000000000000, 0.9238795325112867385, 1.000000000000000000, 0.9238795325112867385, 1.000000000000000000, 0.9238795325112867385, 1.000000000000000000, 0.9238795325112867385, 1.000000000000000000, 0.9238795325112867385, 1.000000000000000000, 0.9238795325112867385, 1.000000000000000000, 0.9238795325112867385, 1.000000000000000000, 0.9238795325112867385, 1.000000000000000000, 0.9238795325112867385, 1.000000000000000000, 0.9238795325112867385, 1.000000000000000000, 0.9238795325112867385, 1.000000000000000000, 0.9238795325112867385, 1.000000000000000000, 0.9238795325112867385, 1.000000000000000000, 0.9238795325112867385, 1.000000000000000000, 0.9238795325112867385, 1.000000000000000000, 0.9238795325112867385, 1.000000000000000000, 0.9238795325112867385, 1.000000000000000000, 0.9238795325112867385, 1.000000000000000000, 0.9238795325112867385, 1.000000000000000000, 0.9238795325112867385, 1.000000000000000000, 0.9238795325112867385, 1.000000000000000000, 0.9238795325112867385, 1.000000000000000000, 0.9238795325112867385, 1.000000000000000000, 0.9238795325112867385, 1.000000000000000000, 0.9238795325112867385, 1.000000000000000000, 0.9238795325112867385, 1.000000000000000000, 0.9238795325112867385, 1.000000000000000000, 0.9238795325112867385, 1.000000000000000000, 0.9238795325112867385, 1.000000000000000000, 0.9238795325112867385, 1.000000000000000000, 0.9238795325112867385, 1.000000000000000000, 0.9238795325112867385, 1.000000000000000000, 0.9238795325112867385, 1.000000000000000000, 0.9238795325112867385, 1.000000000000000000, 0.9238795325112867385, 1.000000000000000000, 0.9238795325112867385, 1.000000000000000000, 0.9238795325112867385, 1.000000000000000000, 0.9238795325112867385, 1.000000000000000000, 0.9238795325112867385, 1.000000000000000000, 0.9238795325112867385, 1.000000000000000000, 0.9238795325112867385, 1.000000000000000000, 0.9238795325112867385, 1.000000000000000000, 0.9238795325112867385, 1.000000000000000000, 0.9238795325112867385, 1.000000000000000000, 0.9238795325112867385, 1.000000000000000000, 0.9238795325112867385, 1.000000000000000000, 0.9238795325112867385, 1.000000000000000000, 0.9238795325112867385, 1.000000000000000000, 0.9238795325112867385, 1.000000000000000000, 0.9238795325112867385, 1.000000000000000000, 0.9238795325112867385, 1.000000000000000000, 0.9238795325112867385, 1.000000000000000000, 0.9238795325112867385, 1.000000000000000000, 0.9238795325112867385, 1.000000000000000000, 0.9238795325112867385, 1.000000000000000000, 0.9238795325112867385, 1.000000000000000000, 0.9238795325112867385, 1.000000000000000000, 0.9238795325112867385, 1.000000000000000000, 0.9238795325112867385, 1.000000000000000000, 0.9238795325112867385, 1.000000000000000000, 0.9238795325112867385, 1.000000000000000000, 0.9238795325112867385, 1.000000000000000000, 0.9238795325112867385, 1.000000000000000000, 0.9238795325112867385, 1.000000000000000000, 0.9238795325112867385, 1.000000000000000000, 0.9238795325112867385, 1.000000000000000000, 0.9238795325112867385, 1.000000000000000000, 0.9238795325112867385, 1.000000000000000000, 0.9238795325112867385, 1.000000000000000000, 0.9238795325112867385, 1.000000000000000000, 0.9238795325112867385, 1.000000000000000000, 0.9238795325112867385, 1.000000000000000000, 0.9238795325112867385, 1.000000000000000000, 0.9238795325112867385, 1.000000000000000000, 0.9238795325112867385, 1.000000000000000000, 0.9238795325112867385, 1.000000000000000000, 0.9238795325112867385, 1.000000000000000000, 0.9238795325112867385, 1.000000000000000000, 0.9238795325112867385, 1.000000000000000000, 0.9238795325112867385, 1.000000000000000000, 0.9238795325112867385, 1.000000000000000000, 0.9238795325112867385, 1.000000000000000000, 0.9238795325112867385, 1.000000000000000000, 0.9238795325112867385, 1.000000000000000000, 0.9238795325112867385, 1.000000000000000000, 0.9238795325112867385, 1.000000000000000000, 0.9238795325112867385, 1.000000000000000000, 0.9238795325112867385, 1.000000000000000000, 0.9238795325112867385, 1.000000000000000000, 0.9238795325112867385, 1.000000000000000000, 0.9462258450566536361, 0.9684275698016389100) ) ) 
 REPRESENTATION_ITEM ( '' )  SURFACE ( )  );
#9383 = DIRECTION ( 'NONE',  ( 0.000000000000000000, 0.000000000000000000, -1.000000000000000000 ) ) ;
#9384 = CARTESIAN_POINT ( 'NONE',  ( 13.57481594606304576, 32.66562499999999858, -1.662435489736055892E-15 ) ) ;
#9385 = CARTESIAN_POINT ( 'NONE',  ( 124.5550856135277087, 38.22187500108393010, -13.14518615778179900 ) ) ;
#9386 = EDGE_CURVE ( 'NONE', #4933, #3340, #17333, .T. ) ;
#9387 = ORIENTED_EDGE ( 'NONE', *, *, #606, .T. ) ;
#9388 = CARTESIAN_POINT ( 'NONE',  ( 94.99999999999995737, 80.93750000000000000, -2.071067811865491048 ) ) ;
#9389 = CARTESIAN_POINT ( 'NONE',  ( 99.99999999999998579, 94.75000000000000000, 4.999999999999984013 ) ) ;
#9390 = CARTESIAN_POINT ( 'NONE',  ( 103.5355339059327093, 79.75000000273119838, -3.535533905932755072 ) ) ;
#9391 = CARTESIAN_POINT ( 'NONE',  ( 104.9999999999999716, 93.06249999999998579, -2.071067811865478170 ) ) ;
#9392 = CARTESIAN_POINT ( 'NONE',  ( 74.59884440882045453, 39.80937500216786873, 9.598844408820456309 ) ) ;
#9393 = CARTESIAN_POINT ( 'NONE',  ( 91.91746824999997045, 112.6261737610028320, -49.72499999726881725 ) ) ;
#9394 = CARTESIAN_POINT ( 'NONE',  ( 71.94442362476911512, 31.75150628229955529, -11.16113343896966370 ) ) ;
#9395 = ORIENTED_EDGE ( 'NONE', *, *, #13660, .T. ) ;
#9396 = CARTESIAN_POINT ( 'NONE',  ( 97.92893218813459555, 95.56249999726881583, 5.000000000000046185 ) ) ;
#9397 = CARTESIAN_POINT ( 'NONE',  ( 104.9999999999999574, -2.071067811865462627, 11.43750000000000000 ) ) ;
#9398 = ORIENTED_EDGE ( 'NONE', *, *, #16018, .T. ) ;
#9399 = CARTESIAN_POINT ( 'NONE',  ( 9.295050272127046043, 37.27929687608394005, -9.295050272127046043 ) ) ;
#9400 = CARTESIAN_POINT ( 'NONE',  ( 200.6228728715778686, 34.99726562716787726, 13.57481594606304576 ) ) ;
#9401 = AXIS2_PLACEMENT_3D ( 'NONE', #16073, #18511, #855 ) ;
#9402 = CARTESIAN_POINT ( 'NONE',  ( 9.295050272127047819, 32.11992187608393579, 9.295050272127046043 ) ) ;
#9403 = CARTESIAN_POINT ( 'NONE',  ( 104.9999999999999716, 1.449011120738813565E-14, 11.50000000000000000 ) ) ;
#9404 = CARTESIAN_POINT ( 'NONE',  ( 130.0000000000000000, 52.00000000000000711, -1.503427012513233026E-14 ) ) ;
#9405 = CARTESIAN_POINT ( 'NONE',  ( -13.14518615778179189, 36.03906250108394005, 5.444914386472304635 ) ) ;
#9406 = CARTESIAN_POINT ( 'NONE',  ( 106.9999999999999858, 107.7255621263696241, -49.60000000546236976 ) ) ;
#9407 = CARTESIAN_POINT ( 'NONE',  ( 99.99999999999998579, 92.06249999863440792, 4.458734124999981674 ) ) ;
#9408 = FACE_OUTER_BOUND ( 'NONE', #14008, .T. ) ;
#9409 = VECTOR ( 'NONE', #27035, 1000.000000000000000 ) ;
#9410 = DIRECTION ( 'NONE',  ( 0.000000000000000000, 0.000000000000000000, 1.000000000000000000 ) ) ;
#9411 = CARTESIAN_POINT ( 'NONE',  ( -13.57481594606304576, 33.06249999999999289, 0.000000000000000000 ) ) ;
#9412 = CARTESIAN_POINT ( 'NONE',  ( 96.84719886470459471, -3.152801135295355994, 8.812500001365592084 ) ) ;
#9413 = DIRECTION ( 'NONE',  ( -0.000000000000000000, -1.000000000000000000, -0.000000000000000000 ) ) ;
#9414 = CARTESIAN_POINT ( 'NONE',  ( 104.4587341249999639, 1.442382525525748735E-14, 10.93750000136559208 ) ) ;
#9415 = CARTESIAN_POINT ( 'NONE',  ( 91.91746824999999887, 110.0000000000000000, -47.12500000273119838 ) ) ;
#9416 = CARTESIAN_POINT ( 'NONE',  ( 96.84719886470463734, 92.18749999863440792, 3.152801135295351997 ) ) ;
#9417 = CARTESIAN_POINT ( 'NONE',  ( 103.5355339059327093, 83.75000000273119838, -3.535533905932755072 ) ) ;
#9418 = CARTESIAN_POINT ( 'NONE',  ( 95.00472066334981491, 103.1245878333314465, -55.32499999726882578 ) ) ;
#9419 = CARTESIAN_POINT ( 'NONE',  ( -5.444914386472299306, 33.75703125108393721, 13.14518615778179722 ) ) ;
#9420 = ORIENTED_EDGE ( 'NONE', *, *, #27379, .T. ) ;
#9421 = CARTESIAN_POINT ( 'NONE',  ( 94.99999999999995737, 1.387778780781445676E-14, 13.12500000273118417 ) ) ;
#9422 = FACE_OUTER_BOUND ( 'NONE', #25140, .T. ) ;
#9423 = CARTESIAN_POINT ( 'NONE',  ( -5.622872871577920151, 36.38632812499999858, 13.57481594606300135 ) ) ;
#9424 = CARTESIAN_POINT ( 'NONE',  ( 204.2950502721270425, 35.29492187608393294, 9.295050272127046043 ) ) ;
#9425 = VERTEX_POINT ( 'NONE', #23618 ) ;
#9426 = CARTESIAN_POINT ( 'NONE',  ( 107.0000000000000000, 112.2744378736303190, -49.39999999453763735 ) ) ;
#9427 = CARTESIAN_POINT ( 'NONE',  ( 101.8468681455906903, -4.458734124999987891, 12.00000000136559208 ) ) ;
#9428 = PRODUCT_DEFINITION ( 'UNKNOWN', '', #27259, #20902 ) ;
#9429 = EDGE_CURVE ( 'NONE', #16918, #23612, #24961, .T. ) ;
#9430 = VERTEX_POINT ( 'NONE', #17187 ) ;
#9431 = CARTESIAN_POINT ( 'NONE',  ( 105.6631189606246295, 105.8855032339526758, -47.20000000000000284 ) ) ;
#9432 = CARTESIAN_POINT ( 'NONE',  ( -9.295050272127044266, 37.47773437608393010, 9.295050272127047819 ) ) ;
#9433 = CARTESIAN_POINT ( 'NONE',  ( 102.0669872999999939, 122.8000000010924708, -0.8561741729129507261 ) ) ;
#9434 = CARTESIAN_POINT ( 'NONE',  ( 94.33688103937534208, 114.1144967660473242, -53.20000000000000995 ) ) ;
#9435 = CARTESIAN_POINT ( 'NONE',  ( 120.7049497278729575, 36.68398437608392726, 9.295050272127047819 ) ) ;
#9436 = CARTESIAN_POINT ( 'NONE',  ( 2.414731522848535132E-15, 39.36289062608393152, 13.14518615778179544 ) ) ;
#9437 = CARTESIAN_POINT ( 'NONE',  ( 13.14518615778179900, 35.34453125108392868, 5.444914386472293977 ) ) ;
#9438 = CARTESIAN_POINT ( 'NONE',  ( 95.54126587499999346, 94.12499999863439371, 1.846868145590722543 ) ) ;
#9439 = AXIS2_PLACEMENT_3D ( 'NONE', #21406, #6283, #22208 ) ;
#9440 = CARTESIAN_POINT ( 'NONE',  ( 55.81982418635199394, 50.00000000000000000, -9.999999999999985789 ) ) ;
#9441 = CARTESIAN_POINT ( 'NONE',  ( 91.91746824999998466, 112.6261737610028320, -49.47500000273119269 ) ) ;
#9442 = CARTESIAN_POINT ( 'NONE',  ( 185.7049497278729575, 31.92148437608393508, -9.295050272127046043 ) ) ;
#9443 = ORIENTED_EDGE ( 'NONE', *, *, #21801, .F. ) ;
#9444 = CARTESIAN_POINT ( 'NONE',  ( 71.35193222877107644, 36.00000000000000711, 11.61660627739524365 ) ) ;
#9445 = CARTESIAN_POINT ( 'NONE',  ( 9.295050272127046043, 37.27929687608394005, -9.295050272127046043 ) ) ;
#9446 = CARTESIAN_POINT ( 'NONE',  ( 95.54126587499996504, 1.387778780781445676E-14, 7.687500001365592084 ) ) ;
#9447 = CARTESIAN_POINT ( 'NONE',  ( 74.29505027212704249, 37.87460937608393152, -9.295050272127046043 ) ) ;
#9448 = PRODUCT_DEFINITION_SHAPE ( 'NONE', 'NONE',  #28206 ) ;
#9449 = LINE ( 'NONE', #3188, #3787 ) ;
#9450 = CARTESIAN_POINT ( 'NONE',  ( 195.0000000000000000, 36.78320312608393294, 13.14518615778179544 ) ) ;
#9451 = CARTESIAN_POINT ( 'NONE',  ( 5.444914386472297529, 34.94765625108394147, -13.14518615778179722 ) ) ;
#9452 = CARTESIAN_POINT ( 'NONE',  ( 99.14382582708707048, 123.1000000010924822, 2.066987299999979211 ) ) ;
#9453 = CARTESIAN_POINT ( 'NONE',  ( 96.84719886470463734, 92.18749999863440792, 3.152801135295351997 ) ) ;
#9454 = CARTESIAN_POINT ( 'NONE',  ( 204.2950502721270425, 37.87460937608393863, 9.295050272127046043 ) ) ;
#9455 = CARTESIAN_POINT ( 'NONE',  ( 95.00472066334982912, 103.1245878333314323, -51.57499999726880446 ) ) ;
#9456 = EDGE_LOOP ( 'NONE', ( #9109, #20168, #25538, #10951 ) ) ;
#9457 = CARTESIAN_POINT ( 'NONE',  ( 13.57481594606304576, 33.45937499999999432, -1.662435489736055892E-15 ) ) ;
#9458 = CARTESIAN_POINT ( 'NONE',  ( -13.14518615778179900, 33.36015625108393579, -5.444914386472297529 ) ) ;
#9459 = VERTEX_POINT ( 'NONE', #381 ) ;
#9460 = CARTESIAN_POINT ( 'NONE',  ( 130.0000000000000000, 32.21914062608393436, 13.14518615778179544 ) ) ;
#9461 = CARTESIAN_POINT ( 'NONE',  ( 55.70494972787295751, 31.92148437608393508, 9.295050272127047819 ) ) ;
#9462 = CARTESIAN_POINT ( 'NONE',  ( 208.1451861577817795, 35.64218750108393152, -5.444914386472297529 ) ) ;
#9463 = ORIENTED_EDGE ( 'NONE', *, *, #8241, .F. ) ;
#9464 = CARTESIAN_POINT ( 'NONE',  ( 98.53841926354351699, 123.6500000010924794, -1.461580736456474794 ) ) ;
#9465 = CARTESIAN_POINT ( 'NONE',  ( 5.365496568045275971, 54.48174559707876341, -15.00000000000000000 ) ) ;
#9466 =( BOUNDED_SURFACE ( )  B_SPLINE_SURFACE ( 3, 2, ( 
 ( #20598, #1224, #26880 ),
 ( #16446, #14016, #5066 ),
 ( #3346, #18460, #2919 ),
 ( #22740, #27166, #22452 ),
 ( #7619, #5490, #9465 ),
 ( #7325, #15874, #5207 ),
 ( #11449, #12016, #18598 ),
 ( #14159, #20170, #20739 ),
 ( #27302, #7760, #25142 ),
 ( #5633, #652, #9325 ),
 ( #18021, #13871, #21149 ),
 ( #27572, #12711, #4048 ),
 ( #5912, #25839, #23015 ),
 ( #3903, #21017, #6179 ),
 ( #16589, #8307, #8032 ),
 ( #10439, #1496, #12151 ),
 ( #27431, #1633, #19146 ),
 ( #10152, #6314, #16730 ),
 ( #18863, #14847, #1915 ),
 ( #10580, #8174, #25697 ) ),
 .UNSPECIFIED., .F., .F., .F. ) 
 B_SPLINE_SURFACE_WITH_KNOTS ( ( 4, 2, 2, 2, 2, 2, 2, 2, 2, 4 ),
 ( 3, 3 ),
 ( 0.009073803551359463371, 0.01139250602759181788, 0.01371120850382417065, 0.01602991098005652343, 0.01834861345628887794, 0.01950796469440505693, 0.02066731593252123245, 0.02298601840875358349, 0.02530472088498593800, 0.02762342336121829250 ),
 ( 0.000000000000000000, 1.000000000000000000 ),
 .UNSPECIFIED. ) 
 GEOMETRIC_REPRESENTATION_ITEM ( )  RATIONAL_B_SPLINE_SURFACE ( (
 ( 1.000000000000000000, 0.7071067811865473507, 1.000000000000000000),
 ( 1.000000000000000000, 0.7344871497829210671, 1.000000000000000000),
 ( 1.000000000000000000, 0.7612510203318444413, 1.000000000000000000),
 ( 1.000000000000000000, 0.8116663633844437564, 1.000000000000000000),
 ( 1.000000000000000000, 0.8353358059750773945, 1.000000000000000000),
 ( 1.000000000000000000, 0.8764699612587100175, 1.000000000000000000),
 ( 1.000000000000000000, 0.8939017358719162365, 1.000000000000000000),
 ( 1.000000000000000000, 0.9185314935647118650, 1.000000000000000000),
 ( 1.000000000000000000, 0.9256439951239471275, 1.000000000000000000),
 ( 1.000000000000000000, 0.9261623622476505835, 1.000000000000000000),
 ( 1.000000000000000000, 0.9246301385978624721, 1.000000000000000000),
 ( 1.000000000000000000, 0.9183304321348235710, 1.000000000000000000),
 ( 1.000000000000000000, 0.9135987334168408358, 1.000000000000000000),
 ( 1.000000000000000000, 0.8954110486039673633, 1.000000000000000000),
 ( 1.000000000000000000, 0.8779877431163967128, 1.000000000000000000),
 ( 1.000000000000000000, 0.8366182664709538308, 1.000000000000000000),
 ( 1.000000000000000000, 0.8126941604019177756, 1.000000000000000000),
 ( 1.000000000000000000, 0.7617527316302064033, 1.000000000000000000),
 ( 1.000000000000000000, 0.7347103785794923958, 1.000000000000000000),
 ( 1.000000000000000000, 0.7071067811865462405, 1.000000000000000000) ) ) 
 REPRESENTATION_ITEM ( '' )  SURFACE ( )  );
#9467 = ADVANCED_FACE ( 'NONE', ( #23893 ), #26027, .F. ) ;
#9468 = CARTESIAN_POINT ( 'NONE',  ( 143.5748159460630404, 37.47773437716787726, 5.622872871577869525 ) ) ;
#9469 = CARTESIAN_POINT ( 'NONE',  ( 91.91746824999998466, 112.6261737610028320, -45.22500000273119980 ) ) ;
#9470 = ADVANCED_FACE ( 'NONE', ( #17467 ), #10904, .T. ) ;
#9471 = DIRECTION ( 'NONE',  ( -0.000000000000000000, -1.000000000000000000, -0.000000000000000000 ) ) ;
#9472 = CARTESIAN_POINT ( 'NONE',  ( 99.99999999999995737, 1.387778780781445676E-14, 34.79898987322334136 ) ) ;
#9473 = CARTESIAN_POINT ( 'NONE',  ( 208.1451861577817795, 40.40468750108393436, -5.444914386472297529 ) ) ;
#9474 = VERTEX_POINT ( 'NONE', #8644 ) ;
#9475 = CARTESIAN_POINT ( 'NONE',  ( 104.4587341249999781, 1.846868145590750299, 4.000000001365592084 ) ) ;
#9476 = ORIENTED_EDGE ( 'NONE', *, *, #16974, .T. ) ;
#9477 = CARTESIAN_POINT ( 'NONE',  ( -4.972887739508807137, 36.00000000000002842, -12.48139679469879582 ) ) ;
#9478 = CARTESIAN_POINT ( 'NONE',  ( 96.84719886470459471, 3.152801135295383084, 6.312500001365592084 ) ) ;
#9479 = CARTESIAN_POINT ( 'NONE',  ( 208.5748159460630688, 38.22187499999999716, -1.662435489736055892E-15 ) ) ;
#9480 = ADVANCED_FACE ( 'NONE', ( #6778 ), #234, .F. ) ;
#9481 = CARTESIAN_POINT ( 'NONE',  ( -9.295050272127044266, 35.89023437608393152, 9.295050272127047819 ) ) ;
#9482 = CARTESIAN_POINT ( 'NONE',  ( -11.26481880218186227, 36.00000000000000000, 6.828991891054477570 ) ) ;
#9483 = CARTESIAN_POINT ( 'NONE',  ( 99.99999999999998579, 95.62499999726881583, 4.999999999999984013 ) ) ;
#9484 = CARTESIAN_POINT ( 'NONE',  ( 95.00472066334982912, 116.8754121666685393, -47.42500000273118843 ) ) ;
#9485 = CARTESIAN_POINT ( 'NONE',  ( -9.598844408820458085, 39.41250000216787441, -9.598844408820458085 ) ) ;
#9486 = AXIS2_PLACEMENT_3D ( 'NONE', #11823, #9410, #20687 ) ;
#9487 = CARTESIAN_POINT ( 'NONE',  ( 204.1801758136479918, 55.00000000000000000, -15.00000000000000000 ) ) ;
#9488 = CARTESIAN_POINT ( 'NONE',  ( -2.169956583105884018, 49.99999999883904422, 13.43548448457833366 ) ) ;
#9489 = CARTESIAN_POINT ( 'NONE',  ( 103.5355339059327235, 91.74999999726880162, 3.535533905932724874 ) ) ;
#9490 = CARTESIAN_POINT ( 'NONE',  ( 139.5988444088204687, 34.94765624999999432, 9.598844408820456309 ) ) ;
#9491 = ORIENTED_EDGE ( 'NONE', *, *, #17393, .F. ) ;
#9492 = ORIENTED_EDGE ( 'NONE', *, *, #14367, .T. ) ;
#9493 = CARTESIAN_POINT ( 'NONE',  ( -20.00000000000000355, 55.00000000000000000, -14.99999999999999822 ) ) ;
#9494 = CARTESIAN_POINT ( 'NONE',  ( -8.049105076161786076E-16, 32.61601562608393579, -13.14518615778179544 ) ) ;
#9495 = CARTESIAN_POINT ( 'NONE',  ( 5.622872871577878406, 33.40976562716787157, 13.57481594606304576 ) ) ;
#9496 = CARTESIAN_POINT ( 'NONE',  ( 97.92893218813451028, 5.000000000000018652, 7.937500002731185056 ) ) ;
#9497 = CARTESIAN_POINT ( 'NONE',  ( 120.7049497278729575, 34.10429687608393579, -9.295050272127046043 ) ) ;
#9498 = CARTESIAN_POINT ( 'NONE',  ( 68.87838541077974241, 31.34156310770110565, -13.57481594606304931 ) ) ;
#9499 = ADVANCED_FACE ( 'NONE', ( #13028 ), #13316, .F. ) ;
#9500 = DIRECTION ( 'NONE',  ( 5.782411586589357392E-17, -0.000000000000000000, 1.000000000000000000 ) ) ;
#9501 = CARTESIAN_POINT ( 'NONE',  ( -8.049105076161786076E-16, 39.56132812608393579, -13.14518615778179544 ) ) ;
#9502 = AXIS2_PLACEMENT_3D ( 'NONE', #3731, #19527, #2150 ) ;
#9503 = LINE ( 'NONE', #18204, #4340 ) ;
#9504 = CARTESIAN_POINT ( 'NONE',  ( 96.46446609406721961, -3.535533905932727539, 1.124999999999999334 ) ) ;
#9505 = CARTESIAN_POINT ( 'NONE',  ( 102.4976396683250783, 117.6869444889999841, -50.47499999726882436 ) ) ;
#9506 = DIRECTION ( 'NONE',  ( 5.782411586589357392E-17, 0.000000000000000000, 1.000000000000000000 ) ) ;
#9507 = VECTOR ( 'NONE', #6805, 1000.000000000000000 ) ;
#9508 = FACE_OUTER_BOUND ( 'NONE', #23259, .T. ) ;
#9509 = DIRECTION ( 'NONE',  ( 0.000000000000000000, 0.000000000000000000, -1.000000000000000000 ) ) ;
#9510 = CARTESIAN_POINT ( 'NONE',  ( 98.23223304703363112, 124.3069999999781459, 1.767766952966351557 ) ) ;
#9511 = EDGE_CURVE ( 'NONE', #5570, #10432, #12889, .T. ) ;
#9512 = CARTESIAN_POINT ( 'NONE',  ( 97.93301269999999192, 124.5000000010924879, -0.8561741729129505041 ) ) ;
#9514 = ORIENTED_EDGE ( 'NONE', *, *, #22631, .T. ) ;
#9513 = CYLINDRICAL_SURFACE ( 'NONE', #20999, 5.000000000000000888 ) ;
#9515 =( BOUNDED_CURVE ( )  B_SPLINE_CURVE ( 2, ( #24514, #2296, #292, #15229, #23947, #15373, #15521, #13081, #26374 ),
 .UNSPECIFIED., .F., .T. ) 
 B_SPLINE_CURVE_WITH_KNOTS ( ( 3, 2, 2, 2, 3 ),
 ( 0.1041666666666664909, 0.1145833333333332732, 0.1250000000000000833, 0.1354166666666668517, 0.1458333333333336757 ),
 .UNSPECIFIED. ) 
 CURVE ( )  GEOMETRIC_REPRESENTATION_ITEM ( )  RATIONAL_B_SPLINE_CURVE ( ( 1.000000000000001332, 0.9238795325112854062, 1.000000000000000000, 0.9238795325112867385, 1.000000000000000000, 0.9238795325112867385, 1.000000000000000000, 0.9238795325112842960, 1.000000000000002442 ) ) 
 REPRESENTATION_ITEM ( '' )  );
#9516 = DIRECTION ( 'NONE',  ( 1.000000000000000000, 0.000000000000000000, 0.000000000000000000 ) ) ;
#9517 = CARTESIAN_POINT ( 'NONE',  ( 204.5988444088204687, 39.01562500216787299, 9.598844408820456309 ) ) ;
#9518 = CARTESIAN_POINT ( 'NONE',  ( 9.598844408820459861, 32.56640625000000000, 9.598844408820456309 ) ) ;
#9519 = CARTESIAN_POINT ( 'NONE',  ( -3.420220812170877700, 35.99999999999999289, -13.02105590829194348 ) ) ;
#9520 = CARTESIAN_POINT ( 'NONE',  ( 9.295050272127047819, 33.90585937608393863, 9.295050272127046043 ) ) ;
#9521 = CARTESIAN_POINT ( 'NONE',  ( 2.414731522848535132E-15, 34.40195312608393152, 13.14518615778179544 ) ) ;
#9522 = CARTESIAN_POINT ( 'NONE',  ( -9.295050272127046043, 34.89804687608393152, -9.295050272127046043 ) ) ;
#9523 = CARTESIAN_POINT ( 'NONE',  ( -5.622872871577873077, 34.60039062716786873, -13.57481594606304753 ) ) ;
#9524 = DIRECTION ( 'NONE',  ( 0.000000000000000000, -1.000000000000000000, 0.000000000000000000 ) ) ;
#9525 = CARTESIAN_POINT ( 'NONE',  ( -5.622872871577782483, 35.29492187499999289, -13.57481594606313990 ) ) ;
#9526 = CARTESIAN_POINT ( 'NONE',  ( 70.44491438647230552, 32.07031250108393294, 13.14518615778179189 ) ) ;
#9527 = CARTESIAN_POINT ( 'NONE',  ( 99.99999999999998579, 90.75000000000000000, 4.999999999999984013 ) ) ;
#9528 = CARTESIAN_POINT ( 'NONE',  ( 97.50120075755764049, 123.0000000000000000, 0.1653216690150871027 ) ) ;
#9529 = VERTEX_POINT ( 'NONE', #6364 ) ;
#9530 = CARTESIAN_POINT ( 'NONE',  ( 98.09035273295538104, 123.0000000000000142, 0.7910017786517971050 ) ) ;
#9531 = CARTESIAN_POINT ( 'NONE',  ( -13.57481594606304576, 33.85624999999999574, 0.000000000000000000 ) ) ;
#9532 = CARTESIAN_POINT ( 'NONE',  ( 130.0000000000000000, 34.99726562608393721, -13.14518615778179544 ) ) ;
#9533 = ORIENTED_EDGE ( 'NONE', *, *, #7781, .F. ) ;
#9534 = CARTESIAN_POINT ( 'NONE',  ( 94.99999999999995737, 82.06250000000001421, 2.071067811865466624 ) ) ;
#9535 =( GEOMETRIC_REPRESENTATION_CONTEXT ( 3 ) GLOBAL_UNCERTAINTY_ASSIGNED_CONTEXT ( ( #4715 ) ) GLOBAL_UNIT_ASSIGNED_CONTEXT ( ( #4934, #22461, #661 ) ) REPRESENTATION_CONTEXT ( 'NONE', 'WORKASPACE' ) );
#9536 = CARTESIAN_POINT ( 'NONE',  ( 102.1631189606246153, 116.6573956140660897, -47.60000000000000853 ) ) ;
#9537 = CARTESIAN_POINT ( 'NONE',  ( 96.84719886470459471, 82.56250000136559208, 3.152801135295355994 ) ) ;
#9538 = CARTESIAN_POINT ( 'NONE',  ( 104.9999999999999716, 90.93749999999998579, 2.071067811865467956 ) ) ;
#9539 = CARTESIAN_POINT ( 'NONE',  ( 65.00000000000000000, 38.91640625216786731, 13.57481594606304576 ) ) ;
#9540 = CARTESIAN_POINT ( 'NONE',  ( 107.0000000000000000, 107.7255621263696668, -54.10000000000000853 ) ) ;
#9541 = CARTESIAN_POINT ( 'NONE',  ( 78.57481594606304043, 40.65273437499998721, -5.622872871577873077 ) ) ;
#9542 = CARTESIAN_POINT ( 'NONE',  ( 9.598844408820456309, 37.62656250216787157, -9.598844408820458085 ) ) ;
#9543 = VERTEX_POINT ( 'NONE', #6498 ) ;
#9544 = CYLINDRICAL_SURFACE ( 'NONE', #18156, 5.000000000000004441 ) ;
#9545 = CARTESIAN_POINT ( 'NONE',  ( 96.46446609406721961, -3.535533905932727539, 13.12500000000000000 ) ) ;
#9546 = ORIENTED_EDGE ( 'NONE', *, *, #6239, .T. ) ;
#9547 = CARTESIAN_POINT ( 'NONE',  ( -5.444914386472297529, 37.42812500108394147, -13.14518615778179900 ) ) ;
#9548 = CARTESIAN_POINT ( 'NONE',  ( 181.4251840539369596, 31.62382812716787228, 5.622872871577880183 ) ) ;
#9549 = CARTESIAN_POINT ( 'NONE',  ( -9.295050272127044266, 32.71523437608393436, 9.295050272127047819 ) ) ;
#9550 = EDGE_CURVE ( 'NONE', #15121, #7547, #19493, .T. ) ;
#9551 = CARTESIAN_POINT ( 'NONE',  ( 99.99999999999995737, 5.000000000000018652, 13.87500000273118594 ) ) ;
#9552 = CARTESIAN_POINT ( 'NONE',  ( 204.5988444088204687, 38.22187500216787015, 9.598844408820456309 ) ) ;
#9553 = CARTESIAN_POINT ( 'NONE',  ( -13.14518615778179900, 34.35234375108393579, -5.444914386472297529 ) ) ;
#9554 = CARTESIAN_POINT ( 'NONE',  ( 130.0000000000000000, 32.02070312608393010, 13.14518615778179544 ) ) ;
#9555 = CARTESIAN_POINT ( 'NONE',  ( 51.42518405393695957, 33.01289062500000426, -5.622872871577873077 ) ) ;
#9556 = FACE_OUTER_BOUND ( 'NONE', #23488, .T. ) ;
#9557 = CARTESIAN_POINT ( 'NONE',  ( 130.0000000000000000, 0.000000000000000000, 0.000000000000000000 ) ) ;
#9558 = CARTESIAN_POINT ( 'NONE',  ( 99.99999999999995737, -4.458734124999988779, 5.937500001365592084 ) ) ;
#9559 = CARTESIAN_POINT ( 'NONE',  ( 99.99999999999998579, 90.00000000000000000, 2.999999999999982681 ) ) ;
#9560 = CARTESIAN_POINT ( 'NONE',  ( 104.4587341249999639, 1.442382525525748735E-14, 8.937500001365592084 ) ) ;
#9561 = CARTESIAN_POINT ( 'NONE',  ( 102.4976396683250925, 117.6869444889999841, -45.72500000273119269 ) ) ;
#9562 = CARTESIAN_POINT ( 'NONE',  ( 99.99999999999998579, 91.81249999863440792, -4.458734124999994997 ) ) ;
#9563 = DIRECTION ( 'NONE',  ( -0.000000000000000000, -0.000000000000000000, -1.000000000000000000 ) ) ;
#9564 = DIRECTION ( 'NONE',  ( -0.000000000000000000, -1.000000000000000000, -0.000000000000000000 ) ) ;
#9565 = CARTESIAN_POINT ( 'NONE',  ( 13.14518615778179544, 34.00507812608393721, -1.609821015232357215E-15 ) ) ;
#9566 = ORIENTED_EDGE ( 'NONE', *, *, #11740, .T. ) ;
#9567 = CARTESIAN_POINT ( 'NONE',  ( 0.000000000000000000, -7.395377635281828788, 0.000000000000000000 ) ) ;
#9568 = CARTESIAN_POINT ( 'NONE',  ( 92.99999999999998579, 110.0000000000000000, -45.74999999726882294 ) ) ;
#9569 = CARTESIAN_POINT ( 'NONE',  ( 104.9999999999999858, 95.43749999863440792, -6.938893903907228378E-15 ) ) ;
#9570 = CARTESIAN_POINT ( 'NONE',  ( 185.7049497278729575, 35.69179687608393436, -9.295050272127046043 ) ) ;
#9571 = VERTEX_POINT ( 'NONE', #19332 ) ;
#9572 = CARTESIAN_POINT ( 'NONE',  ( 2.493653234604083739E-15, 37.22968749999999716, 13.57481594606304576 ) ) ;
#9573 = CARTESIAN_POINT ( 'NONE',  ( 103.1528011352953342, 3.152801135295383084, 10.31250000136559208 ) ) ;
#9574 = VECTOR ( 'NONE', #16646, 1000.000000000000227 ) ;
#9575 = EDGE_LOOP ( 'NONE', ( #4212, #7319, #13144, #15480 ) ) ;
#9576 = CARTESIAN_POINT ( 'NONE',  ( 104.3262379212492590, 104.0454443415356991, -45.29999999999999716 ) ) ;
#9577 = CARTESIAN_POINT ( 'NONE',  ( -9.295050272127046043, 36.48554687608393721, -9.295050272127046043 ) ) ;
#9578 = CARTESIAN_POINT ( 'NONE',  ( 97.50000000000000000, 124.1499999999999915, -1.035533905932742416 ) ) ;
#9579 = LINE ( 'NONE', #5319, #11202 ) ;
#9580 = CARTESIAN_POINT ( 'NONE',  ( 143.1451861577818079, 37.72578125108393721, 5.444914386472293977 ) ) ;
#9581 = CARTESIAN_POINT ( 'NONE',  ( -5.444914386472297529, 39.01562500108394005, -13.14518615778179722 ) ) ;
#9582 = CARTESIAN_POINT ( 'NONE',  ( 9.295050272127047819, 34.50117187608393010, 9.295050272127046043 ) ) ;
#9583 = CARTESIAN_POINT ( 'NONE',  ( 95.54126587499999346, 92.12499999863437949, 1.846868145590722543 ) ) ;
#9584 = CARTESIAN_POINT ( 'NONE',  ( 68.71653411378430576, 51.46663580899353008, -14.99999999999931966 ) ) ;
#9585 = CARTESIAN_POINT ( 'NONE',  ( 108.0825317500000153, 110.0000000000000000, -48.37500000273119838 ) ) ;
#9586 = ORIENTED_EDGE ( 'NONE', *, *, #17805, .F. ) ;
#9587 = CARTESIAN_POINT ( 'NONE',  ( 102.1631189606246295, 103.3426043859339103, -50.40000000000001279 ) ) ;
#9588 = CARTESIAN_POINT ( 'NONE',  ( -13.14518615778179189, 36.83281250108393579, 5.444914386472304635 ) ) ;
#9589 = CARTESIAN_POINT ( 'NONE',  ( 98.15313185440923860, 4.458734125000016313, 7.500000001365592084 ) ) ;
#9590 = CARTESIAN_POINT ( 'NONE',  ( 51.85481384221820633, 37.37851562608393863, 0.000000000000000000 ) ) ;
#9591 = CARTESIAN_POINT ( 'NONE',  ( 99.99999999999998579, 124.3999999999999915, 2.499999999999978684 ) ) ;
#9592 = CARTESIAN_POINT ( 'NONE',  ( 96.46446609406721961, -3.535533905932727539, 2.124999999999998224 ) ) ;
#9593 = EDGE_LOOP ( 'NONE', ( #5358, #23086, #5501, #7741 ) ) ;
#9594 = CARTESIAN_POINT ( 'NONE',  ( 5.444914386472302859, 34.65000000108393863, 13.14518615778179189 ) ) ;
#9595 = EDGE_CURVE ( 'NONE', #2581, #23665, #23753, .T. ) ;
#9596 = CARTESIAN_POINT ( 'NONE',  ( 101.4615807364564546, 122.6500000010924794, -1.461580736456474794 ) ) ;
#9597 = LINE ( 'NONE', #9177, #27158 ) ;
#9598 = CARTESIAN_POINT ( 'NONE',  ( 208.1451861577818079, 38.71796875108393721, 5.444914386472293977 ) ) ;
#9599 = CARTESIAN_POINT ( 'NONE',  ( 104.9952793366501709, 116.8754121666685393, -50.57499999726882578 ) ) ;
#9600 = EDGE_LOOP ( 'NONE', ( #27164, #22842, #16874, #3912, #14373 ) ) ;
#9601 = AXIS2_PLACEMENT_3D ( 'NONE', #2339, #25987, #15129 ) ;
#9602 = CARTESIAN_POINT ( 'NONE',  ( -5.622872871577873077, 34.50117187499999005, -13.57481594606304753 ) ) ;
#9603 = CARTESIAN_POINT ( 'NONE',  ( 13.14518615778179900, 33.85625000108393579, -5.444914386472297529 ) ) ;
#9604 = ORIENTED_EDGE ( 'NONE', *, *, #5841, .F. ) ;
#9605 = CARTESIAN_POINT ( 'NONE',  ( 116.8548138422182205, 32.81445312608393294, 0.000000000000000000 ) ) ;
#9606 = CARTESIAN_POINT ( 'NONE',  ( 65.00000000000000000, 32.02070312608393010, 13.14518615778179544 ) ) ;
#9607 = CARTESIAN_POINT ( 'NONE',  ( 195.0000000000000000, 34.60039062608393579, 13.14518615778179544 ) ) ;
#9608 = ORIENTED_EDGE ( 'NONE', *, *, #13839, .F. ) ;
#9609 = CARTESIAN_POINT ( 'NONE',  ( 104.7293670624999748, 95.15624999931721106, -6.938893903907228378E-15 ) ) ;
#9610 = CARTESIAN_POINT ( 'NONE',  ( 97.92893218813451028, 5.000000000000018652, 8.937500002731184168 ) ) ;
#9611 = CARTESIAN_POINT ( 'NONE',  ( 97.92893218813451028, -4.999999999999989342, 1.312500002731184612 ) ) ;
#9612 = CARTESIAN_POINT ( 'NONE',  ( 143.5748159460630688, 37.52734375216787299, -1.662435489736055892E-15 ) ) ;
#9613 = CARTESIAN_POINT ( 'NONE',  ( 93.46109445667491400, 114.7507929638356785, -47.32500000273119412 ) ) ;
#9614 = CARTESIAN_POINT ( 'NONE',  ( 65.00000000000000000, 50.00000000000000000, 13.57481594606303688 ) ) ;
#9615 = CARTESIAN_POINT ( 'NONE',  ( 99.99999999999995737, 1.387778780781445676E-14, 34.79898987322334136 ) ) ;
#9616 = CARTESIAN_POINT ( 'NONE',  ( 69.85849929045953388, 49.99999999891532099, 12.70434618649044189 ) ) ;
#9617 = ORIENTED_EDGE ( 'NONE', *, *, #23297, .T. ) ;
#9618 =( NAMED_UNIT ( * ) PLANE_ANGLE_UNIT ( ) SI_UNIT ( $, .RADIAN. ) );
#9619 = CARTESIAN_POINT ( 'NONE',  ( 104.4587341249999781, -1.846868145590721655, 4.875000001365592084 ) ) ;
#9620 = ORIENTED_EDGE ( 'NONE', *, *, #15372, .T. ) ;
#9621 = CARTESIAN_POINT ( 'NONE',  ( -6.470563696665745823, 36.00000000000002132, -11.78199955157067080 ) ) ;
#9622 = CARTESIAN_POINT ( 'NONE',  ( 96.84719886470459471, -3.152801135295355994, 7.562500001365592084 ) ) ;
#9623 = CARTESIAN_POINT ( 'NONE',  ( 0.000000000000000000, 40.99999999999999289, 0.000000000000000000 ) ) ;
#9624 = CARTESIAN_POINT ( 'NONE',  ( 104.7293670624999748, 90.15624999931721106, -6.938893903907228378E-15 ) ) ;
#9625 = CARTESIAN_POINT ( 'NONE',  ( 71.94442639331153089, 31.75150625057403175, -11.16113171639042356 ) ) ;
#9626 = CARTESIAN_POINT ( 'NONE',  ( -3.061616997868383831E-15, 0.000000000000000000, -25.00000000000000711 ) ) ;
#9627 = CARTESIAN_POINT ( 'NONE',  ( 93.46109445667491400, 105.2492070361643215, -44.92500000273119554 ) ) ;
#9628 = CARTESIAN_POINT ( 'NONE',  ( 195.0000000000000000, 38.02343749999999289, 13.57481594606304576 ) ) ;
#9629 = CARTESIAN_POINT ( 'NONE',  ( 9.598844408820459861, 35.04687500216787299, 9.598844408820456309 ) ) ;
#9630 = CARTESIAN_POINT ( 'NONE',  ( 4.858499290463564435, 49.99999999891551994, 12.70434618648897818 ) ) ;
#9631 = LINE ( 'NONE', #26757, #27917 ) ;
#9632 = CARTESIAN_POINT ( 'NONE',  ( 130.0000000000000000, 33.26093749999999716, 13.57481594606304576 ) ) ;
#9633 = VERTEX_POINT ( 'NONE', #12758 ) ;
#9634 = CARTESIAN_POINT ( 'NONE',  ( 95.67376207875072680, 115.9545556584642867, -51.30000000000000426 ) ) ;
#9635 = ADVANCED_FACE ( 'NONE', ( #21619, #8921 ), #15320, .T. ) ;
#9636 = CARTESIAN_POINT ( 'NONE',  ( 9.295050272127046043, 34.10429687608393579, -9.295050272127046043 ) ) ;
#9637 = CARTESIAN_POINT ( 'NONE',  ( -13.57481594606304753, 34.69960937716787441, -5.622872871577873077 ) ) ;
#9638 =( BOUNDED_CURVE ( )  B_SPLINE_CURVE ( 2, ( #5087, #26613, #15757, #11328, #7060, #24463, #4946, #26755, #14179, #8049, #27321 ),
 .UNSPECIFIED., .F., .F. ) 
 B_SPLINE_CURVE_WITH_KNOTS ( ( 3, 2, 2, 2, 2, 3 ),
 ( 0.3999999999999996891, 0.4199999999999996514, 0.4399999999999996692, 0.4599999999999996869, 0.4799999999999996492, 0.4999999999999996669 ),
 .UNSPECIFIED. ) 
 CURVE ( )  GEOMETRIC_REPRESENTATION_ITEM ( )  RATIONAL_B_SPLINE_CURVE ( ( 1.000000000000000888, 0.9510565162951527540, 1.000000000000000000, 0.9510565162951535312, 1.000000000000000000, 0.9510565162951535312, 1.000000000000000000, 0.9510565162951535312, 1.000000000000000000, 0.9510565162951543083, 0.9999999999999992228 ) ) 
 REPRESENTATION_ITEM ( '' )  );
#9639 = CARTESIAN_POINT ( 'NONE',  ( 99.99999999999995737, 5.000000000000018652, 7.875000002731185056 ) ) ;
#9640 = CARTESIAN_POINT ( 'NONE',  ( 116.8548138422182205, 33.40976562608393863, 0.000000000000000000 ) ) ;
#9641 = CARTESIAN_POINT ( 'NONE',  ( 74.29505027212704249, 40.05742187608392868, 9.295050272127046043 ) ) ;
#9642 = CARTESIAN_POINT ( 'NONE',  ( 99.99999999999995737, 5.000000000000018652, 14.75000000000000000 ) ) ;
#9643 = CARTESIAN_POINT ( 'NONE',  ( -8.049105076161786076E-16, 38.76757812608393294, -13.14518615778179544 ) ) ;
#9644 = CARTESIAN_POINT ( 'NONE',  ( 5.444914386472302859, 33.06250000108393294, 13.14518615778179189 ) ) ;
#9645 = CARTESIAN_POINT ( 'NONE',  ( 181.9416181435491637, 36.00000000000000711, 1.569311539113946274 ) ) ;
#9646 = CARTESIAN_POINT ( 'NONE',  ( 106.5389055433250860, 114.7507929638356785, -52.67499999726882010 ) ) ;
#9647 = FACE_BOUND ( 'NONE', #22999, .T. ) ;
#9648 = CARTESIAN_POINT ( 'NONE',  ( 185.7049497278729575, 32.51679687608393721, -9.295050272127046043 ) ) ;
#9649 = LINE ( 'NONE', #4826, #24289 ) ;
#9650 = CARTESIAN_POINT ( 'NONE',  ( 99.99999999999998579, 123.3000000021849587, -2.499999999999997780 ) ) ;
#9651 = CARTESIAN_POINT ( 'NONE',  ( 97.93301269999999192, 123.8000000010924850, 0.8561741729129329626 ) ) ;
#9652 = CARTESIAN_POINT ( 'NONE',  ( 92.99999999999997158, 112.2744378736302906, -50.59999999453763309 ) ) ;
#9653 = EDGE_CURVE ( 'NONE', #3976, #1420, #25612, .T. ) ;
#9654 = CARTESIAN_POINT ( 'NONE',  ( -13.57481594606304753, 35.39414062499999147, -5.622872871577872189 ) ) ;
#9655 = DIRECTION ( 'NONE',  ( -0.000000000000000000, 1.000000000000000000, -0.000000000000000000 ) ) ;
#9656 = CARTESIAN_POINT ( 'NONE',  ( 2.493653234604083739E-15, 35.64218749999999147, 13.57481594606304576 ) ) ;
#9657 = CARTESIAN_POINT ( 'NONE',  ( -13.57481594606304753, 33.01289062499999716, -5.622872871577872189 ) ) ;
#9658 = CARTESIAN_POINT ( 'NONE',  ( -9.295050272127044266, 34.50117187608393721, 9.295050272127047819 ) ) ;
#9659 = CARTESIAN_POINT ( 'NONE',  ( 2.414731522848535132E-15, 32.02070312608393010, 13.14518615778179544 ) ) ;
#9660 = CARTESIAN_POINT ( 'NONE',  ( -13.14518615778179722, 34.94765625108394147, -5.444914386472297529 ) ) ;
#9661 = CARTESIAN_POINT ( 'NONE',  ( 13.57481594606304576, 36.73359375216787015, -1.662435489736055892E-15 ) ) ;
#9662 = DIRECTION ( 'NONE',  ( -5.782411586589357392E-17, 0.000000000000000000, -1.000000000000000000 ) ) ;
#9663 = CARTESIAN_POINT ( 'NONE',  ( 96.84719886470459471, 83.31250000136560629, -3.152801135295383084 ) ) ;
#9664 = CARTESIAN_POINT ( 'NONE',  ( 74.29505027212704249, 33.90585937608393152, -9.295050272127046043 ) ) ;
#9665 = CARTESIAN_POINT ( 'NONE',  ( 97.50236033167492167, 117.6869444889999841, -53.77500000273119696 ) ) ;
#9666 = DIRECTION ( 'NONE',  ( -1.000000000000000000, 0.000000000000000000, 7.228014483236696740E-18 ) ) ;
#9667 = EDGE_CURVE ( 'NONE', #24795, #14317, #17790, .T. ) ;
#9668 = CARTESIAN_POINT ( 'NONE',  ( 124.3771271284220319, 37.77539062716787299, -13.57481594606295339 ) ) ;
#9669 = CARTESIAN_POINT ( 'NONE',  ( 13.57481594606304753, 34.30273437500000000, -5.622872871577873077 ) ) ;
#9670 = CARTESIAN_POINT ( 'NONE',  ( 91.91746824999997045, 112.6261737610028320, -53.97499999726881725 ) ) ;
#9671 = CARTESIAN_POINT ( 'NONE',  ( 135.4449143864723055, 33.06250000108393294, 13.14518615778179189 ) ) ;
#9672 = ORIENTED_EDGE ( 'NONE', *, *, #17170, .F. ) ;
#9673 = CARTESIAN_POINT ( 'NONE',  ( 104.9999999999999574, 81.56250000000002842, -2.071067811865491937 ) ) ;
#9674 = EDGE_CURVE ( 'NONE', #8206, #3171, #3453, .T. ) ;
#9675 = CARTESIAN_POINT ( 'NONE',  ( 78.57481594606305464, 38.27148437716787299, 5.622872871577868636 ) ) ;
#9676 = CARTESIAN_POINT ( 'NONE',  ( 104.4587341249999781, 83.00000000136559208, -1.846868145590750299 ) ) ;
#9677 = CARTESIAN_POINT ( 'NONE',  ( 102.0710678118654613, 94.18749999999998579, -4.999999999999997335 ) ) ;
#9678 = CARTESIAN_POINT ( 'NONE',  ( 208.5748159460630688, 37.37851562499999858, 5.622872871577868636 ) ) ;
#9679 = ADVANCED_FACE ( 'NONE', ( #5470, #7599 ), #14139, .F. ) ;
#9680 = CARTESIAN_POINT ( 'NONE',  ( 104.9952793366501709, 116.8754121666685393, -48.32499999726881867 ) ) ;
#9681 = CARTESIAN_POINT ( 'NONE',  ( 208.1451861577818079, 39.56132812608393579, -1.609821015232357215E-15 ) ) ;
#9682 = CARTESIAN_POINT ( 'NONE',  ( -8.312177448680279460E-16, 37.72578125216787726, -13.57481594606304576 ) ) ;
#9683 = ORIENTED_EDGE ( 'NONE', *, *, #10318, .T. ) ;
#9684 = CARTESIAN_POINT ( 'NONE',  ( 183.0647576233092195, 35.99999999999999289, -5.809862729997679054 ) ) ;
#9685 = AXIS2_PLACEMENT_3D ( 'NONE', #23647, #4122, #7840 ) ;
#9686 = CARTESIAN_POINT ( 'NONE',  ( 96.46446609406721961, -3.535533905932727539, 14.12499999999999822 ) ) ;
#9687 = EDGE_CURVE ( 'NONE', #2214, #144, #14422, .T. ) ;
#9688 = ORIENTED_EDGE ( 'NONE', *, *, #10913, .T. ) ;
#9689 =( BOUNDED_CURVE ( )  B_SPLINE_CURVE ( 2, ( #3873, #21120, #23540, #21263, #19392, #19117, #18974, #2017, #3739, #1886, #25808, #20987, #8001, #12818, #1745, #21541, #23266, #1468, #25952, #27824, #14960, #25400, #6284, #8278, #16969, #8414, #14816, #23680, #3603, #21407, #19258, #10124, #28097, #27682, #4016, #14550, #12682, #25668, #18837, #17104, #10550, #16702, #6150, #8145, #4157, #10685, #8560, #17251, #14412, #5881, #12262, #27544, #12399, #16839, #25536, #6016, #14679, #23400, #13234, #11105, #15382, #19966, #6839, #4437, #9266, #26384, #17962, #11247, #15676, #6426, #12951, #19675, #19819, #302, #22250, #23957, #9127, #443, #10964, #8988, #15095, #4865, #19536, #6980, #24237, #21685, #4720, #18, #13089, #2160, #17820, #26525, #24097, #4573, #21829, #23815, #17394 ),
 .UNSPECIFIED., .F., .F. ) 
 B_SPLINE_CURVE_WITH_KNOTS ( ( 3, 2, 2, 2, 2, 2, 2, 2, 2, 2, 2, 2, 2, 2, 2, 2, 2, 2, 2, 2, 2, 2, 2, 2, 2, 2, 2, 2, 2, 2, 2, 2, 2, 2, 2, 2, 2, 2, 2, 2, 2, 2, 2, 2, 2, 2, 2, 2, 3 ),
 ( 0.000000000000000000, 0.01041666666666666609, 0.02083333333333333218, 0.03125000000000000000, 0.04166666666666666435, 0.05208333333333333565, 0.06250000000000000000, 0.07291666666666667129, 0.08333333333333332871, 0.09374999999999998612, 0.1041666666666666713, 0.1145833333333333287, 0.1250000000000000000, 0.1354166666666666574, 0.1458333333333333426, 0.1562500000000000000, 0.1666666666666666574, 0.1770833333333333426, 0.1874999999999999722, 0.1979166666666666574, 0.2083333333333333426, 0.2187500000000000000, 0.2291666666666666574, 0.2395833333333333426, 0.2500000000000000000, 0.2604166666666666852, 0.2708333333333333148, 0.2812500000000000000, 0.2916666666666666852, 0.3020833333333333148, 0.3125000000000000000, 0.3229166666666666852, 0.3333333333333333148, 0.3437500000000000000, 0.3541666666666666852, 0.3645833333333333148, 0.3749999999999999445, 0.3854166666666666852, 0.3958333333333333148, 0.4062500000000000000, 0.4166666666666666852, 0.4270833333333333148, 0.4375000000000000000, 0.4479166666666666852, 0.4583333333333333148, 0.4687500000000000000, 0.4791666666666666852, 0.4895833333333333148, 0.4988304892921909817 ),
 .UNSPECIFIED. ) 
 CURVE ( )  GEOMETRIC_REPRESENTATION_ITEM ( )  RATIONAL_B_SPLINE_CURVE ( ( 1.000000000000000000, 0.9238795325112867385, 1.000000000000000000, 0.9238795325112867385, 1.000000000000000000, 0.9238795325112867385, 1.000000000000000000, 0.9238795325112867385, 1.000000000000000000, 0.9238795325112867385, 1.000000000000000000, 0.9238795325112867385, 1.000000000000000000, 0.9238795325112867385, 1.000000000000000000, 0.9238795325112867385, 1.000000000000000000, 0.9238795325112867385, 1.000000000000000000, 0.9238795325112867385, 1.000000000000000000, 0.9238795325112867385, 1.000000000000000000, 0.9238795325112867385, 1.000000000000000000, 0.9238795325112867385, 1.000000000000000000, 0.9238795325112867385, 1.000000000000000000, 0.9238795325112867385, 1.000000000000000000, 0.9238795325112867385, 1.000000000000000000, 0.9238795325112867385, 1.000000000000000000, 0.9238795325112867385, 1.000000000000000000, 0.9238795325112867385, 1.000000000000000000, 0.9238795325112867385, 1.000000000000000000, 0.9238795325112867385, 1.000000000000000000, 0.9238795325112867385, 1.000000000000000000, 0.9238795325112867385, 1.000000000000000000, 0.9238795325112867385, 1.000000000000000000, 0.9238795325112867385, 1.000000000000000000, 0.9238795325112867385, 1.000000000000000000, 0.9238795325112867385, 1.000000000000000000, 0.9238795325112867385, 1.000000000000000000, 0.9238795325112867385, 1.000000000000000000, 0.9238795325112867385, 1.000000000000000000, 0.9238795325112867385, 1.000000000000000000, 0.9238795325112867385, 1.000000000000000000, 0.9238795325112867385, 1.000000000000000000, 0.9238795325112867385, 1.000000000000000000, 0.9238795325112867385, 1.000000000000000000, 0.9238795325112867385, 1.000000000000000000, 0.9238795325112867385, 1.000000000000000000, 0.9238795325112867385, 1.000000000000000000, 0.9238795325112867385, 1.000000000000000000, 0.9238795325112867385, 1.000000000000000000, 0.9238795325112867385, 1.000000000000000000, 0.9238795325112867385, 1.000000000000000000, 0.9238795325112867385, 1.000000000000000000, 0.9238795325112867385, 1.000000000000000000, 0.9238795325112867385, 1.000000000000000000, 0.9238795325112867385, 1.000000000000000000, 0.9238795325112867385, 1.000000000000000000, 0.9324258078851886955, 0.9848264816800353927 ) ) 
 REPRESENTATION_ITEM ( '' )  );
#9690 = CARTESIAN_POINT ( 'NONE',  ( 5.444914386472302859, 37.82500000108392868, 13.14518615778179189 ) ) ;
#9691 = CARTESIAN_POINT ( 'NONE',  ( 208.5748159460630688, 31.97109375216787441, -1.662435489736055892E-15 ) ) ;
#9692 = CARTESIAN_POINT ( 'NONE',  ( 13.14518615778179722, 32.26875000108393721, -5.444914386472297529 ) ) ;
#9693 = CARTESIAN_POINT ( 'NONE',  ( 103.5355339059327093, -3.535533905932726206, 13.50000000273118417 ) ) ;
#9694 = CARTESIAN_POINT ( 'NONE',  ( 99.99999999999998579, 129.0000000000000000, -5.204170427930421283E-15 ) ) ;
#9695 = CARTESIAN_POINT ( 'NONE',  ( -9.295050272127044266, 32.11992187608393579, 9.295050272127047819 ) ) ;
#9696 = CARTESIAN_POINT ( 'NONE',  ( 124.5550856135277087, 31.67343750108393863, -13.14518615778179900 ) ) ;
#9697 = CARTESIAN_POINT ( 'NONE',  ( 96.84719886470463734, 92.68749999863440792, -3.152801135295366208 ) ) ;
#9698 = CARTESIAN_POINT ( 'NONE',  ( 101.7677669529663547, 124.5000000000000000, 1.767766952966350891 ) ) ;
#9699 = CARTESIAN_POINT ( 'NONE',  ( 65.00000000000000000, 0.000000000000000000, 0.000000000000000000 ) ) ;
#9700 = CARTESIAN_POINT ( 'NONE',  ( -8.312177448680279460E-16, 32.86406249999999574, -13.57481594606304576 ) ) ;
#9701 = CARTESIAN_POINT ( 'NONE',  ( 99.99999999999995737, 4.458734125000016313, 7.437500001365592084 ) ) ;
#9702 = CARTESIAN_POINT ( 'NONE',  ( 70.44491438647230552, 40.30546875108393579, -13.14518615778179900 ) ) ;
#9703 = CARTESIAN_POINT ( 'NONE',  ( 101.8468681455907046, -4.458734124999987891, 11.75000000136559208 ) ) ;
#9704 = CARTESIAN_POINT ( 'NONE',  ( 107.0000000000000142, 110.0000000000000000, -47.50000000546238255 ) ) ;
#9705 = CARTESIAN_POINT ( 'NONE',  ( 97.50000000000000000, 124.2500000021849900, -1.035533905932742416 ) ) ;
#9706 = CARTESIAN_POINT ( 'NONE',  ( 13.57481594606304576, 39.80937499999999574, -1.662435489736055892E-15 ) ) ;
#9707 = DIRECTION ( 'NONE',  ( 0.000000000000000000, 0.000000000000000000, -1.000000000000000000 ) ) ;
#9708 = CARTESIAN_POINT ( 'NONE',  ( 5.444914386472302859, 33.06250000108393294, 13.14518615778179189 ) ) ;
#9709 = AXIS2_PLACEMENT_3D ( 'NONE', #23167, #3356, #12028 ) ;
#9710 = ORIENTED_EDGE ( 'NONE', *, *, #19439, .T. ) ;
#9711 = DIRECTION ( 'NONE',  ( -0.000000000000000000, -1.000000000000000000, -0.000000000000000000 ) ) ;
#9712 = CARTESIAN_POINT ( 'NONE',  ( 97.92893218813451028, 91.31249999999998579, -4.999999999999984013 ) ) ;
#9713 = CARTESIAN_POINT ( 'NONE',  ( -9.598844408820458085, 36.13828124999999147, -9.598844408820458085 ) ) ;
#9714 = EDGE_CURVE ( 'NONE', #9261, #7715, #6187, .T. ) ;
#9715 = CARTESIAN_POINT ( 'NONE',  ( 204.2950502721270425, 34.69960937608393436, -9.295050272127046043 ) ) ;
#9716 = ORIENTED_EDGE ( 'NONE', *, *, #11787, .F. ) ;
#9717 = CARTESIAN_POINT ( 'NONE',  ( 101.8468681455906903, 4.458734125000016313, 12.37500000136559208 ) ) ;
#9718 = EDGE_LOOP ( 'NONE', ( #27607, #14326 ) ) ;
#9719 = CARTESIAN_POINT ( 'NONE',  ( 99.99999999999998579, 118.4984768113314004, -49.87500000273118417 ) ) ;
#9720 = CARTESIAN_POINT ( 'NONE',  ( -8.049105076161786076E-16, 37.18007812608393436, -13.14518615778179544 ) ) ;
#9721 = CARTESIAN_POINT ( 'NONE',  ( 195.0000000000000000, 39.71015625216787015, 13.57481594606304576 ) ) ;
#9722 = CARTESIAN_POINT ( 'NONE',  ( 98.23223304703363112, 123.2999999999999972, -1.767766952966370209 ) ) ;
#9723 = CARTESIAN_POINT ( 'NONE',  ( 143.1451861577818079, 38.56914062608393579, -1.609821015232357215E-15 ) ) ;
#9724 = CARTESIAN_POINT ( 'NONE',  ( 9.295050272127047819, 38.66835937608393436, 9.295050272127046043 ) ) ;
#9725 = CARTESIAN_POINT ( 'NONE',  ( -9.295050272127046043, 40.65273437608393436, -9.295050272127046043 ) ) ;
#9726 = CARTESIAN_POINT ( 'NONE',  ( 98.15313185440925281, 93.24999999863439371, 4.458734124999979898 ) ) ;
#9727 = CARTESIAN_POINT ( 'NONE',  ( -8.312177448680279460E-16, 36.13828125216787157, -13.57481594606304576 ) ) ;
#9728 = CARTESIAN_POINT ( 'NONE',  ( 95.00472066334981491, 103.1245878333314465, -51.07500000273119412 ) ) ;
#9729 = DIRECTION ( 'NONE',  ( 0.000000000000000000, -1.000000000000000000, 0.000000000000000000 ) ) ;
#9730 = CARTESIAN_POINT ( 'NONE',  ( -9.295050272127044266, 35.29492187608393294, 9.295050272127047819 ) ) ;
#9731 = CARTESIAN_POINT ( 'NONE',  ( 103.1528011352953342, 3.152801135295383084, 5.312500001365592972 ) ) ;
#9732 = CARTESIAN_POINT ( 'NONE',  ( 78.14518615778180788, 36.13828125108393152, 5.444914386472293977 ) ) ;
#9733 = CARTESIAN_POINT ( 'NONE',  ( 13.57481594606304931, 32.61601562499999574, 5.622872871577868636 ) ) ;
#9734 = DIRECTION ( 'NONE',  ( 5.782411586589357392E-17, -0.000000000000000000, 1.000000000000000000 ) ) ;
#9735 = CARTESIAN_POINT ( 'NONE',  ( 195.0000000000000000, -7.395377635281828788, 13.57481594606302266 ) ) ;
#9736 = CARTESIAN_POINT ( 'NONE',  ( -9.295050272127046043, 33.50898437608393010, -9.295050272127046043 ) ) ;
#9737 = CARTESIAN_POINT ( 'NONE',  ( 97.93301269999999192, 123.7000000010924765, -0.8561741729129505041 ) ) ;
#9738 = CARTESIAN_POINT ( 'NONE',  ( -5.622872871577920151, 36.08867187500000284, -13.57481594606300135 ) ) ;
#9739 = CARTESIAN_POINT ( 'NONE',  ( 195.0000000000000000, 38.96601562608393721, -13.14518615778179544 ) ) ;
#9740 = CARTESIAN_POINT ( 'NONE',  ( 104.9952793366501709, 116.8754121666685393, -48.57499999726881867 ) ) ;
#9741 = CARTESIAN_POINT ( 'NONE',  ( 13.57481594606304931, 34.99726562500000426, 5.622872871577869525 ) ) ;
#9742 = CARTESIAN_POINT ( 'NONE',  ( 13.14518615778179544, 34.60039062608392868, -1.609821015232357215E-15 ) ) ;
#9743 = ORIENTED_EDGE ( 'NONE', *, *, #5433, .F. ) ;
#9744 = CARTESIAN_POINT ( 'NONE',  ( 91.91746824999998466, 110.0000000000000000, -55.74999999726882294 ) ) ;
#9745 = CARTESIAN_POINT ( 'NONE',  ( 104.9999999999999716, 1.449011120738813565E-14, 0.6250000027311856110 ) ) ;
#9746 = CYLINDRICAL_SURFACE ( 'NONE', #1877, 5.000000000000004441 ) ;
#9747 = CARTESIAN_POINT ( 'NONE',  ( 200.4449143864723055, 34.65000000108393863, 13.14518615778179189 ) ) ;
#9748 = ORIENTED_EDGE ( 'NONE', *, *, #7968, .F. ) ;
#9749 = CARTESIAN_POINT ( 'NONE',  ( 100.8561741729129295, 124.3000000010924850, -2.066987299999998751 ) ) ;
#9750 = CARTESIAN_POINT ( 'NONE',  ( 99.99999999999998579, 110.0000000000000000, -145.0000000000000284 ) ) ;
#9751 = CARTESIAN_POINT ( 'NONE',  ( 187.3760580380745466, 55.00000000000000711, 14.99999999999995559 ) ) ;
#9752 = CARTESIAN_POINT ( 'NONE',  ( 143.5748159460630404, 38.37070312716786447, -5.622872871577873077 ) ) ;
#9753 = CARTESIAN_POINT ( 'NONE',  ( 99.99999999999995737, -4.999999999999990230, 7.249999999999999112 ) ) ;
#9754 = DIRECTION ( 'NONE',  ( -0.000000000000000000, 1.000000000000000000, -0.000000000000000000 ) ) ;
#9755 = CARTESIAN_POINT ( 'NONE',  ( 71.11984362770094492, 51.28708186914658995, 14.99999999999719513 ) ) ;
#9756 = ORIENTED_EDGE ( 'NONE', *, *, #18381, .T. ) ;
#9757 = ORIENTED_EDGE ( 'NONE', *, *, #8291, .F. ) ;
#9758 = SHAPE_REPRESENTATION_RELATIONSHIP ( 'NONE' , 'NONE' ,  #10045, #24660 ) ;
#9759 = CARTESIAN_POINT ( 'NONE',  ( 99.99999999999995737, -4.458734124999988779, 4.687500001365592084 ) ) ;
#9760 = CARTESIAN_POINT ( 'NONE',  ( 103.5355339059327093, 3.535533905932755072, 12.75000000273118594 ) ) ;
#9761 = CARTESIAN_POINT ( 'NONE',  ( 96.84719886470459471, 3.152801135295383084, 3.312500001365592972 ) ) ;
#9762 = CARTESIAN_POINT ( 'NONE',  ( 136.4128666762518662, 50.00000000108477849, 11.99502265407748780 ) ) ;
#9763 = CARTESIAN_POINT ( 'NONE',  ( -5.569058551903145471, 35.99999999999999289, 11.91493531101255599 ) ) ;
#9764 = CARTESIAN_POINT ( 'NONE',  ( 55.70494972787295751, 32.91367187608393152, 9.295050272127047819 ) ) ;
#9765 = CARTESIAN_POINT ( 'NONE',  ( 94.99999999999995737, 1.387778780781445676E-14, 4.999999999999999112 ) ) ;
#9766 = CARTESIAN_POINT ( 'NONE',  ( 108.0825317500000011, 107.3738262389971538, -44.22500000273118559 ) ) ;
#9767 = CARTESIAN_POINT ( 'NONE',  ( 13.14518615778179722, 36.13828125108393152, 5.444914386472293977 ) ) ;
#9768 = VECTOR ( 'NONE', #9223, 1000.000000000000000 ) ;
#9769 = CARTESIAN_POINT ( 'NONE',  ( 5.622872871578015186, 34.99726562716787015, 13.57481594606290543 ) ) ;
#9770 = CARTESIAN_POINT ( 'NONE',  ( -0.8389268692817103412, 53.50081894914648473, 14.99999999999999645 ) ) ;
#9771 = CARTESIAN_POINT ( 'NONE',  ( 103.5355339059327235, 90.99999999726880162, -3.535533905932738197 ) ) ;
#9772 = CARTESIAN_POINT ( 'NONE',  ( 124.3771271284221314, 34.79882812499998579, 13.57481594606304753 ) ) ;
#9773 = ORIENTED_EDGE ( 'NONE', *, *, #19217, .T. ) ;
#9774 = ORIENTED_EDGE ( 'NONE', *, *, #3693, .T. ) ;
#9775 = PLANE ( 'NONE',  #19019 ) ;
#9776 = CARTESIAN_POINT ( 'NONE',  ( -9.295050272127044266, 32.91367187608393152, 9.295050272127047819 ) ) ;
#9777 = CARTESIAN_POINT ( 'NONE',  ( -13.57481594606304576, 35.54296875216788010, 0.000000000000000000 ) ) ;
#9778 = CARTESIAN_POINT ( 'NONE',  ( 104.9999999999999574, 2.071067811865491937, 6.687500002731185056 ) ) ;
#9779 = CARTESIAN_POINT ( 'NONE',  ( 135.4449143864723055, 40.20625000108394431, 13.14518615778179189 ) ) ;
#9780 = CARTESIAN_POINT ( 'NONE',  ( 70.62287287157788285, 31.82226562716787654, 13.57481594606304576 ) ) ;
#9781 = VERTEX_POINT ( 'NONE', #12272 ) ;
#9782 = CARTESIAN_POINT ( 'NONE',  ( 5.622872871577786924, 37.37851562716787157, 13.57481594606313813 ) ) ;
#9783 = CARTESIAN_POINT ( 'NONE',  ( 2.414731522848535132E-15, 37.57695312608392868, 13.14518615778179544 ) ) ;
#9784 = CARTESIAN_POINT ( 'NONE',  ( -9.295050272127046043, 33.50898437608393010, -9.295050272127046043 ) ) ;
#9785 = CARTESIAN_POINT ( 'NONE',  ( 51.42518405393695957, 37.77539062499998579, -5.622872871577872189 ) ) ;
#9786 = CARTESIAN_POINT ( 'NONE',  ( 104.9952793366501567, 116.8754121666685393, -54.57499999726882578 ) ) ;
#9787 = EDGE_CURVE ( 'NONE', #8172, #15313, #7659, .T. ) ;
#9788 = VECTOR ( 'NONE', #16310, 1000.000000000000000 ) ;
#9789 = CARTESIAN_POINT ( 'NONE',  ( 208.5748159460630688, 40.60312499999999858, -1.662435489736055892E-15 ) ) ;
#9790 = CARTESIAN_POINT ( 'NONE',  ( 214.9999999999999716, 50.00000000000000000, -10.00000000000000000 ) ) ;
#9791 = LINE ( 'NONE', #1673, #18382 ) ;
#9792 = CARTESIAN_POINT ( 'NONE',  ( 105.6631189606246295, 105.8855032339526758, -52.20000000000000995 ) ) ;
#9793 = SURFACE_SIDE_STYLE ('',( #11919 ) ) ;
#9794 = DIRECTION ( 'NONE',  ( 1.000000000000000000, 0.000000000000000000, -7.228014483236696740E-18 ) ) ;
#9795 = CARTESIAN_POINT ( 'NONE',  ( 99.99999999999998579, 102.6397644303321215, -47.50000000000000711 ) ) ;
#9796 = CARTESIAN_POINT ( 'NONE',  ( 130.0000000000000000, 38.42031249999999432, -13.57481594606304576 ) ) ;
#9797 = CARTESIAN_POINT ( 'NONE',  ( -9.598844408820454532, 34.74921874999999716, 9.598844408820459861 ) ) ;
#9798 = CARTESIAN_POINT ( 'NONE',  ( -8.312177448680279460E-16, 32.86406249999999574, -13.57481594606304576 ) ) ;
#9799 = CARTESIAN_POINT ( 'NONE',  ( 5.444914386472302859, 34.65000000108393863, 13.14518615778179189 ) ) ;
#9800 = CARTESIAN_POINT ( 'NONE',  ( 13.14518615778179900, 33.75703125108393010, 5.444914386472293977 ) ) ;
#9801 = CARTESIAN_POINT ( 'NONE',  ( 181.4251840539369596, 32.31835937499999289, 5.622872871577880183 ) ) ;
#9802 = CARTESIAN_POINT ( 'NONE',  ( 13.57481594606304576, 35.93984375216787441, -1.662435489736055892E-15 ) ) ;
#9803 = DIRECTION ( 'NONE',  ( -0.000000000000000000, 1.000000000000000000, -0.000000000000000000 ) ) ;
#9804 = CARTESIAN_POINT ( 'NONE',  ( 99.99999999999995737, 84.18750000136560629, -4.458734125000016313 ) ) ;
#9805 = CARTESIAN_POINT ( 'NONE',  ( 59.55508561352770158, 32.46718750108393436, -13.14518615778179900 ) ) ;
#9806 = CARTESIAN_POINT ( 'NONE',  ( 91.91746824999998466, 112.6261737610028320, -53.47500000273119980 ) ) ;
#9807 = DIRECTION ( 'NONE',  ( 0.000000000000000000, 0.000000000000000000, 1.000000000000000000 ) ) ;
#9808 =( BOUNDED_CURVE ( )  B_SPLINE_CURVE ( 2, ( #24856, #496, #11719, #11437, #18009 ),
 .UNSPECIFIED., .F., .T. ) 
 B_SPLINE_CURVE_WITH_KNOTS ( ( 3, 2, 3 ),
 ( 0.000000000000000000, 0.04166666666666694885, 0.08333333333333389770 ),
 .UNSPECIFIED. ) 
 CURVE ( )  GEOMETRIC_REPRESENTATION_ITEM ( )  RATIONAL_B_SPLINE_CURVE ( ( 1.000000000000000000, 0.9238795325112867385, 1.000000000000000000, 0.9238795325112857393, 1.000000000000001110 ) ) 
 REPRESENTATION_ITEM ( '' )  );
#9809 = CARTESIAN_POINT ( 'NONE',  ( 120.4011555911795455, 37.82500000216787583, -9.598844408820458085 ) ) ;
#9810 = CARTESIAN_POINT ( 'NONE',  ( -9.598844408820458085, 32.96328124999999432, -9.598844408820458085 ) ) ;
#9811 = CARTESIAN_POINT ( 'NONE',  ( 106.5389055433250860, 114.7507929638356785, -52.67499999726882010 ) ) ;
#9812 = CARTESIAN_POINT ( 'NONE',  ( 116.8548138422182063, 34.45156250108394147, 5.444914386472304635 ) ) ;
#9813 = ORIENTED_EDGE ( 'NONE', *, *, #14399, .F. ) ;
#9814 = CARTESIAN_POINT ( 'NONE',  ( 104.9999999999999574, 81.43750000000001421, 2.071067811865462627 ) ) ;
#9815 = CARTESIAN_POINT ( 'NONE',  ( 99.99999999999998579, 94.25000000000000000, -4.999999999999997335 ) ) ;
#9816 = CARTESIAN_POINT ( 'NONE',  ( 101.8468681455906903, 82.12500000136560629, -4.458734125000016313 ) ) ;
#9817 = CARTESIAN_POINT ( 'NONE',  ( 95.00000000000000000, 92.50000000000000000, -7.551217303480904118E-15 ) ) ;
#9818 = EDGE_CURVE ( 'NONE', #22175, #18860, #23151, .T. ) ;
#9819 = CARTESIAN_POINT ( 'NONE',  ( 104.9952793366501709, 103.1245878333314323, -46.92499999726882010 ) ) ;
#9820 = CARTESIAN_POINT ( 'NONE',  ( 200.4449143864723055, 39.71015625108393010, -13.14518615778179900 ) ) ;
#9821 = CARTESIAN_POINT ( 'NONE',  ( -13.57481594606304576, 40.30546875216787583, 0.000000000000000000 ) ) ;
#9822 = ORIENTED_EDGE ( 'NONE', *, *, #12253, .T. ) ;
#9823 = CARTESIAN_POINT ( 'NONE',  ( 104.9999999999999716, 1.449011120738813565E-14, 7.500000000000000000 ) ) ;
#9824 = ORIENTED_EDGE ( 'NONE', *, *, #8760, .T. ) ;
#9825 = CARTESIAN_POINT ( 'NONE',  ( -13.14518615778179544, 32.02070312608393010, 0.000000000000000000 ) ) ;
#9826 = CARTESIAN_POINT ( 'NONE',  ( 204.5988444088204403, 32.07031250216787299, -9.598844408820458085 ) ) ;
#9827 = ADVANCED_FACE ( 'NONE', ( #26463, #22859 ), #16428, .F. ) ;
#9828 = CARTESIAN_POINT ( 'NONE',  ( 5.622872871577870413, 36.88242187716787157, -13.57481594606304753 ) ) ;
#9829 = CARTESIAN_POINT ( 'NONE',  ( 104.9999999999999716, 1.449011120738813565E-14, 0.6250000027311856110 ) ) ;
#9830 = CARTESIAN_POINT ( 'NONE',  ( 104.9999999999999716, 1.449011120738813565E-14, 3.499999999999999556 ) ) ;
#9831 = EDGE_CURVE ( 'NONE', #25528, #3896, #9052, .T. ) ;
#9832 = CARTESIAN_POINT ( 'NONE',  ( 102.0710678118654329, 5.000000000000018652, 11.81250000273118950 ) ) ;
#9833 = CARTESIAN_POINT ( 'NONE',  ( 55.40115559117954547, 32.96328124999999432, -9.598844408820458085 ) ) ;
#9834 = CARTESIAN_POINT ( 'NONE',  ( 98.23223304703363112, 123.5000000000000000, 1.767766952966351557 ) ) ;
#9835 =( NAMED_UNIT ( * ) PLANE_ANGLE_UNIT ( ) SI_UNIT ( $, .RADIAN. ) );
#9836 = CARTESIAN_POINT ( 'NONE',  ( 65.00000000000000000, 36.53515625216787299, 13.57481594606304576 ) ) ;
#9837 = CARTESIAN_POINT ( 'NONE',  ( 104.4587341249999781, -1.846868145590721655, 6.125000001365591196 ) ) ;
#9838 = CARTESIAN_POINT ( 'NONE',  ( 97.50000000000000000, 123.4500000000000028, 1.035533905932725096 ) ) ;
#9839 = CARTESIAN_POINT ( 'NONE',  ( 103.1528011352953342, 3.152801135295383084, 11.06250000136559208 ) ) ;
#9840 = CARTESIAN_POINT ( 'NONE',  ( 99.99999999999998579, 117.3602355696678501, -47.00000000546238255 ) ) ;
#9841 = CARTESIAN_POINT ( 'NONE',  ( 101.8468681455907330, 93.74999999863439371, -4.458734124999994997 ) ) ;
#9842 = AXIS2_PLACEMENT_3D ( 'NONE', #22049, #26468, #6369 ) ;
#9843 = CARTESIAN_POINT ( 'NONE',  ( 195.0000000000000000, 39.61093749999999147, 13.57481594606304576 ) ) ;
#9844 = DIRECTION ( 'NONE',  ( 0.000000000000000000, -1.000000000000000000, 0.000000000000000000 ) ) ;
#9845 = CARTESIAN_POINT ( 'NONE',  ( -9.295050272127044266, 32.11992187608393579, 9.295050272127047819 ) ) ;
#9846 = EDGE_CURVE ( 'NONE', #9895, #439, #4043, .T. ) ;
#9847 = ORIENTED_EDGE ( 'NONE', *, *, #6036, .T. ) ;
#9848 =( LENGTH_UNIT ( ) NAMED_UNIT ( * ) SI_UNIT ( .MILLI., .METRE. ) );
#9849 = CARTESIAN_POINT ( 'NONE',  ( -9.598844408820454532, 37.92421874999999432, 9.598844408820459861 ) ) ;
#9850 =( BOUNDED_SURFACE ( )  B_SPLINE_SURFACE ( 3, 2, ( 
 ( #4596, #24546, #13256 ),
 ( #11412, #2465, #611 ),
 ( #9287, #26692, #20416 ),
 ( #27264, #9987, #22843 ),
 ( #25245, #20979, #18418 ),
 ( #1459, #20564, #27124 ),
 ( #5735, #7720, #25108 ),
 ( #18561, #18828, #23119 ),
 ( #16412, #5872, #902 ),
 ( #7428, #3593, #12115 ),
 ( #20841, #16122, #11840 ),
 ( #16270, #24828, #16554 ),
 ( #14120, #12251, #5312 ),
 ( #18696, #7575, #22701 ),
 ( #25391, #20705, #1044 ),
 ( #14262, #22557, #10116 ),
 ( #24968, #3024, #14402 ),
 ( #5596, #3310, #22982 ),
 ( #27536, #7993, #3449 ),
 ( #5452, #16691, #18277 ) ),
 .UNSPECIFIED., .F., .F., .T. ) 
 B_SPLINE_SURFACE_WITH_KNOTS ( ( 4, 2, 2, 2, 2, 2, 2, 2, 2, 4 ),
 ( 3, 3 ),
 ( 0.009073803551359449493, 0.01139250602759181094, 0.01371120850382417239, 0.01602991098005653384, 0.01834861345628889528, 0.01950796469440507774, 0.02066731593252125673, 0.02298601840875361818, 0.02530472088498597616, 0.02762342336121833761 ),
 ( 0.000000000000000000, 1.000000000000000000 ),
 .UNSPECIFIED. ) 
 GEOMETRIC_REPRESENTATION_ITEM ( )  RATIONAL_B_SPLINE_SURFACE ( (
 ( 1.000000000000000000, 0.7071067811865470176, 1.000000000000000000),
 ( 1.000000000000000000, 0.7344871497831121365, 1.000000000000000000),
 ( 1.000000000000000000, 0.7612510203315883128, 1.000000000000000000),
 ( 1.000000000000000000, 0.8116663633847007731, 1.000000000000000000),
 ( 1.000000000000000000, 0.8353358059750350950, 1.000000000000000000),
 ( 1.000000000000000000, 0.8764699612587538713, 1.000000000000000000),
 ( 1.000000000000000000, 0.8939017358718743811, 1.000000000000000000),
 ( 1.000000000000000000, 0.9185314935647557189, 1.000000000000000000),
 ( 1.000000000000000000, 0.9256439951239916475, 1.000000000000000000),
 ( 1.000000000000000000, 0.9261623622476302664, 1.000000000000000000),
 ( 1.000000000000000000, 0.9246301385979071030, 1.000000000000000000),
 ( 1.000000000000000000, 0.9183304321347808274, 1.000000000000000000),
 ( 1.000000000000000000, 0.9135987334169072271, 1.000000000000000000),
 ( 1.000000000000000000, 0.8954110486038381334, 1.000000000000000000),
 ( 1.000000000000000000, 0.8779877431164831991, 1.000000000000000000),
 ( 1.000000000000000000, 0.8366182664708661232, 1.000000000000000000),
 ( 1.000000000000000000, 0.8126941604018734777, 1.000000000000000000),
 ( 1.000000000000000000, 0.7617527316302484808, 1.000000000000000000),
 ( 1.000000000000000000, 0.7347103785794607544, 1.000000000000000000),
 ( 1.000000000000000000, 0.7071067811865446862, 1.000000000000000000) ) ) 
 REPRESENTATION_ITEM ( '' )  SURFACE ( )  );
#9851 = CARTESIAN_POINT ( 'NONE',  ( 181.8548138422182205, 33.40976562608393863, 0.000000000000000000 ) ) ;
#9852 = VERTEX_POINT ( 'NONE', #20580 ) ;
#9853 = AXIS2_PLACEMENT_3D ( 'NONE', #16032, #13890, #13608 ) ;
#9854 = CARTESIAN_POINT ( 'NONE',  ( -13.57481594606304576, 37.03124999999999289, 0.000000000000000000 ) ) ;
#9855 = CARTESIAN_POINT ( 'NONE',  ( 98.15313185440925281, -4.458734124999987891, 7.875000001365591196 ) ) ;
#9856 = EDGE_CURVE ( 'NONE', #23574, #26438, #11956, .T. ) ;
#9857 = VERTEX_POINT ( 'NONE', #8013 ) ;
#9858 = CARTESIAN_POINT ( 'NONE',  ( 91.91746824999998466, 112.6261737610028320, -47.47500000273119269 ) ) ;
#9859 = CARTESIAN_POINT ( 'NONE',  ( -5.444914386472297529, 35.64218750108392442, -13.14518615778179900 ) ) ;
#9860 = VECTOR ( 'NONE', #8203, 1000.000000000000000 ) ;
#9861 = CARTESIAN_POINT ( 'NONE',  ( 185.4011555911795597, 38.81718750216787583, 9.598844408820459861 ) ) ;
#9862 = DIRECTION ( 'NONE',  ( 0.000000000000000000, 0.000000000000000000, 1.000000000000000000 ) ) ;
#9863 = CARTESIAN_POINT ( 'NONE',  ( 5.444914386472297529, 38.91640625108393436, -13.14518615778179722 ) ) ;
#9864 = CARTESIAN_POINT ( 'NONE',  ( -13.14518615778179900, 33.36015625108393579, -5.444914386472297529 ) ) ;
#9865 = CARTESIAN_POINT ( 'NONE',  ( 98.15313185440925281, 91.24999999863439371, 4.458734124999979898 ) ) ;
#9866 = DIRECTION ( 'NONE',  ( 0.000000000000000000, 0.000000000000000000, 1.000000000000000000 ) ) ;
#9867 = ADVANCED_FACE ( 'NONE', ( #16714 ), #26543, .T. ) ;
#9868 = CARTESIAN_POINT ( 'NONE',  ( 105.0000000000000000, 110.0000000000000000, -145.0000000000000284 ) ) ;
#9869 = CARTESIAN_POINT ( 'NONE',  ( 5.444914386472302859, 33.85625000108393579, 13.14518615778179189 ) ) ;
#9870 = CARTESIAN_POINT ( 'NONE',  ( 95.54126587499996504, -1.846868145590724986, 7.750000001365592084 ) ) ;
#9871 = CARTESIAN_POINT ( 'NONE',  ( 103.1528011352953342, 84.31250000136560629, -3.152801135295383084 ) ) ;
#9872 = CARTESIAN_POINT ( 'NONE',  ( 214.9999999999999716, 75.00000000000000000, 9.999999999999946709 ) ) ;
#9873 = CARTESIAN_POINT ( 'NONE',  ( 5.622872871577796694, 39.26367187716788010, -13.57481594606312036 ) ) ;
#9874 = ORIENTED_EDGE ( 'NONE', *, *, #19965, .F. ) ;
#9875 = CARTESIAN_POINT ( 'NONE',  ( -9.295050272127044266, 35.29492187608393294, 9.295050272127047819 ) ) ;
#9876 = CARTESIAN_POINT ( 'NONE',  ( 101.4615807364564546, 124.2500000010924879, -1.461580736456474794 ) ) ;
#9877 = CARTESIAN_POINT ( 'NONE',  ( 96.84719886470463734, 94.18749999863440792, 3.152801135295351997 ) ) ;
#9878 = LINE ( 'NONE', #14569, #9999 ) ;
#9879 = CARTESIAN_POINT ( 'NONE',  ( 104.9952793366501709, 103.1245878333314323, -47.17499999726881299 ) ) ;
#9880 = CARTESIAN_POINT ( 'NONE',  ( -9.598844408820454532, 33.16171874999999858, 9.598844408820459861 ) ) ;
#9881 = ORIENTED_EDGE ( 'NONE', *, *, #17078, .T. ) ;
#9882 = CARTESIAN_POINT ( 'NONE',  ( 208.5748159460630688, 37.57695312716787583, -5.622872871577873966 ) ) ;
#9883 = CARTESIAN_POINT ( 'NONE',  ( 78.14518615778180788, 37.13046875108393863, 5.444914386472293977 ) ) ;
#9884 = DIRECTION ( 'NONE',  ( -1.000000000000000000, 0.000000000000000000, 0.000000000000000000 ) ) ;
#9885 = CARTESIAN_POINT ( 'NONE',  ( -5.622872871577816234, 39.26367187500000000, -13.57481594606310260 ) ) ;
#9886 = ORIENTED_EDGE ( 'NONE', *, *, #14686, .F. ) ;
#9887 = CARTESIAN_POINT ( 'NONE',  ( 99.99999999999998579, 92.75000000000000000, 4.999999999999984013 ) ) ;
#9888 = CARTESIAN_POINT ( 'NONE',  ( 94.99999999999995737, 1.387778780781445676E-14, 9.125000002731184168 ) ) ;
#9889 = CARTESIAN_POINT ( 'NONE',  ( -8.312177448680279460E-16, 33.65781249999999147, -13.57481594606304576 ) ) ;
#9890 = ADVANCED_FACE ( 'NONE', ( #24925 ), #20227, .T. ) ;
#9891 = CARTESIAN_POINT ( 'NONE',  ( 116.4251840539369596, 38.76757812716787299, 5.622872871577880183 ) ) ;
#9892 = CARTESIAN_POINT ( 'NONE',  ( 59.37712712842223794, 40.15664062716787441, -13.57481594606315412 ) ) ;
#9893 = CARTESIAN_POINT ( 'NONE',  ( 94.99999999999998579, 110.0000000000000000, -43.00000000000000000 ) ) ;
#9894 = CARTESIAN_POINT ( 'NONE',  ( 189.5550856135277229, 38.51953125108393294, 13.14518615778179722 ) ) ;
#9895 = VERTEX_POINT ( 'NONE', #5411 ) ;
#9896 = CARTESIAN_POINT ( 'NONE',  ( 95.54126587499995082, 1.846868145590750077, 2.375000001365592084 ) ) ;
#9897 = CARTESIAN_POINT ( 'NONE',  ( -13.09590655363597733, 36.00000000000000000, 1.137167824541468031 ) ) ;
#9898 = CARTESIAN_POINT ( 'NONE',  ( 120.8198241863519939, 50.00000000000000000, 9.999999999999968026 ) ) ;
#9899 = CARTESIAN_POINT ( 'NONE',  ( 95.54126587499996504, 84.37500000136563472, -1.846868145590750077 ) ) ;
#9900 = CARTESIAN_POINT ( 'NONE',  ( 130.0000000000000000, 36.00000000000000000, -11.57481594606305997 ) ) ;
#9901 = CARTESIAN_POINT ( 'NONE',  ( 13.14518615778179900, 40.40468750108393436, -5.444914386472297529 ) ) ;
#9902 = DIRECTION ( 'NONE',  ( 1.224646799147353454E-16, 0.000000000000000000, -1.000000000000000000 ) ) ;
#9903 = CARTESIAN_POINT ( 'NONE',  ( 9.432006169633215364, 36.00000000000001421, 9.391769196591040370 ) ) ;
#9904 = CYLINDRICAL_SURFACE ( 'NONE', #6750, 4.999999999999989342 ) ;
#9905 = CARTESIAN_POINT ( 'NONE',  ( 120.4011555911795455, 34.55078124999999289, -9.598844408820458085 ) ) ;
#9906 = ORIENTED_EDGE ( 'NONE', *, *, #16925, .T. ) ;
#9907 = CARTESIAN_POINT ( 'NONE',  ( 104.9999999999999716, 84.56250000000002842, -2.071067811865491937 ) ) ;
#9908 = CARTESIAN_POINT ( 'NONE',  ( 5.444914386472302859, 33.06250000108393294, 13.14518615778179189 ) ) ;
#9909 = CARTESIAN_POINT ( 'NONE',  ( -13.57481594606304576, 33.16171875216787868, 0.000000000000000000 ) ) ;
#9910 = CARTESIAN_POINT ( 'NONE',  ( 104.9999999999999716, 1.449011120738813565E-14, 7.625000002731185056 ) ) ;
#9911 = CARTESIAN_POINT ( 'NONE',  ( 135.4449143864723055, 38.12265625108393152, -13.14518615778179900 ) ) ;
#9912 = CARTESIAN_POINT ( 'NONE',  ( 51.85481384221820633, 39.75976562608393294, 0.000000000000000000 ) ) ;
#9913 = CARTESIAN_POINT ( 'NONE',  ( 58.66170920764977126, 36.00000000000000000, 11.53992004314981656 ) ) ;
#9914 = CARTESIAN_POINT ( 'NONE',  ( 13.14518615778179544, 38.56914062608393579, -1.609821015232357215E-15 ) ) ;
#9915 = CARTESIAN_POINT ( 'NONE',  ( 9.295050272127047819, 32.31835937608393294, 9.295050272127046043 ) ) ;
#9916 = DIRECTION ( 'NONE',  ( 0.000000000000000000, 0.000000000000000000, 1.000000000000000000 ) ) ;
#9917 = CARTESIAN_POINT ( 'NONE',  ( 95.00472066334981491, 103.1245878333314465, -53.57499999726881157 ) ) ;
#9918 = CARTESIAN_POINT ( 'NONE',  ( 195.0000000000000000, 32.02070312608393010, 13.14518615778179544 ) ) ;
#9919 = CARTESIAN_POINT ( 'NONE',  ( 98.96446609406726225, 124.3500000000000085, 2.499999999999981348 ) ) ;
#9920 = CARTESIAN_POINT ( 'NONE',  ( 97.50000000000000000, 123.4569999999781373, 1.035533905932725096 ) ) ;
#9921 = VECTOR ( 'NONE', #10499, 1000.000000000000000 ) ;
#9922 = CARTESIAN_POINT ( 'NONE',  ( 99.99999999999998579, 122.7500000010924879, -2.066987299999998751 ) ) ;
#9923 = CARTESIAN_POINT ( 'NONE',  ( 116.8508260188483234, 36.00000000000000000, -1.058935892997001416 ) ) ;
#9924 = CARTESIAN_POINT ( 'NONE',  ( 195.0000000000000000, 36.00000000000000000, -2.255140518769849538E-14 ) ) ;
#9925 = AXIS2_PLACEMENT_3D ( 'NONE', #885, #18400, #17573 ) ;
#9926 = CARTESIAN_POINT ( 'NONE',  ( 95.54126587499995082, 1.846868145590750077, 11.37500000136559208 ) ) ;
#9927 = CARTESIAN_POINT ( 'NONE',  ( -9.598844408820458085, 35.34453124999998863, -9.598844408820458085 ) ) ;
#9928 = VERTEX_POINT ( 'NONE', #859 ) ;
#9929 = CARTESIAN_POINT ( 'NONE',  ( 99.99999999999998579, 90.00000000000000000, -4.999999999999996447 ) ) ;
#9930 = CARTESIAN_POINT ( 'NONE',  ( 2.414731522848535132E-15, 32.21914062608393436, 13.14518615778179544 ) ) ;
#9931 = CARTESIAN_POINT ( 'NONE',  ( -9.295050272127046043, 34.10429687608393579, -9.295050272127046043 ) ) ;
#9932 = CARTESIAN_POINT ( 'NONE',  ( 202.1713912169989555, 31.99955315621561525, -11.52591757658528948 ) ) ;
#9933 = CARTESIAN_POINT ( 'NONE',  ( -5.622872871577873077, 33.80664062716786589, -13.57481594606304753 ) ) ;
#9934 = CARTESIAN_POINT ( 'NONE',  ( 99.99999999999998579, 110.0000000000000000, -45.00000000000000711 ) ) ;
#9935 = CARTESIAN_POINT ( 'NONE',  ( 96.84719886470459471, 82.56250000136559208, 3.152801135295355994 ) ) ;
#9936 = CARTESIAN_POINT ( 'NONE',  ( 51.85481384221820633, 31.87187500108393223, 5.444914386472304635 ) ) ;
#9937 = CARTESIAN_POINT ( 'NONE',  ( 106.5389055433251002, 105.2492070361643215, -48.57500000273119412 ) ) ;
#9938 = FACE_OUTER_BOUND ( 'NONE', #10150, .T. ) ;
#9939 = ORIENTED_EDGE ( 'NONE', *, *, #10358, .F. ) ;
#9940 = CARTESIAN_POINT ( 'NONE',  ( 97.93301269999999192, 123.2000000010924765, 0.8561741729129329626 ) ) ;
#9941 = CARTESIAN_POINT ( 'NONE',  ( -13.57481594606304576, 40.99999999999999289, 0.000000000000000000 ) ) ;
#9942 = CARTESIAN_POINT ( 'NONE',  ( 94.33688103937534208, 114.1144967660473242, -46.69999999453764161 ) ) ;
#9943 = CARTESIAN_POINT ( 'NONE',  ( 143.1451861577818079, 35.64218750108393152, -5.444914386472297529 ) ) ;
#9944 = ORIENTED_EDGE ( 'NONE', *, *, #24476, .F. ) ;
#9945 = CARTESIAN_POINT ( 'NONE',  ( 96.46446609406721961, 3.535533905932755072, 7.875000000000000000 ) ) ;
#9946 = ADVANCED_FACE ( 'NONE', ( #25754 ), #12352, .F. ) ;
#9947 = CARTESIAN_POINT ( 'NONE',  ( 65.00000000000000000, 38.51953125216787299, -13.57481594606304576 ) ) ;
#9948 = CARTESIAN_POINT ( 'NONE',  ( 95.54126587499995082, 83.37500000136563472, -1.846868145590750077 ) ) ;
#9949 = CARTESIAN_POINT ( 'NONE',  ( 124.5550856135277087, 39.11484375108394573, 13.14518615778179722 ) ) ;
#9950 = CARTESIAN_POINT ( 'NONE',  ( 195.0000000000000000, 37.22968749999999716, 13.57481594606304576 ) ) ;
#9951 = CIRCLE ( 'NONE', #19971, 5.000000000000000000 ) ;
#9952 = AXIS2_PLACEMENT_3D ( 'NONE', #25224, #5846, #7553 ) ;
#9953 = CARTESIAN_POINT ( 'NONE',  ( 108.0825317500000011, 110.0000000000000000, -48.62499999726882294 ) ) ;
#9954 = AXIS2_PLACEMENT_3D ( 'NONE', #13954, #24525, #20247 ) ;
#9955 = CARTESIAN_POINT ( 'NONE',  ( 9.598844408820456309, 39.21406250216787015, -9.598844408820458085 ) ) ;
#9956 = ORIENTED_EDGE ( 'NONE', *, *, #476, .T. ) ;
#9957 = CARTESIAN_POINT ( 'NONE',  ( 94.99999999999995737, 1.387778780781445676E-14, 11.00000000000000000 ) ) ;
#9958 = ORIENTED_EDGE ( 'NONE', *, *, #24151, .F. ) ;
#9959 = CARTESIAN_POINT ( 'NONE',  ( 13.14518615778179900, 32.46718750108393436, -5.444914386472297529 ) ) ;
#9960 = CARTESIAN_POINT ( 'NONE',  ( 195.0000000000000000, 39.56132812608393579, -13.14518615778179544 ) ) ;
#9961 =( BOUNDED_CURVE ( )  B_SPLINE_CURVE ( 2, ( #16065, #11638, #20924, #1129, #5679, #5254, #23061, #22646, #7518 ),
 .UNSPECIFIED., .F., .F. ) 
 B_SPLINE_CURVE_WITH_KNOTS ( ( 3, 2, 2, 2, 3 ),
 ( 0.02083333333333358892, 0.03125000000000020123, 0.04166666666666681007, 0.05208333333333342585, 0.06250000000000004163 ),
 .UNSPECIFIED. ) 
 CURVE ( )  GEOMETRIC_REPRESENTATION_ITEM ( )  RATIONAL_B_SPLINE_CURVE ( ( 0.9999999999999981126, 0.9238795325112886259, 1.000000000000000000, 0.9238795325112867385, 1.000000000000000000, 0.9238795325112867385, 1.000000000000000000, 0.9238795325112864054, 1.000000000000000222 ) ) 
 REPRESENTATION_ITEM ( '' )  );
#9962 = LINE ( 'NONE', #12498, #17444 ) ;
#9963 = CARTESIAN_POINT ( 'NONE',  ( 94.99999999999997158, 2.071067811865471953, 1.062500002731186832 ) ) ;
#9964 = FACE_OUTER_BOUND ( 'NONE', #1731, .T. ) ;
#9965 = CARTESIAN_POINT ( 'NONE',  ( 2.414731522848535132E-15, 33.01289062608393721, 13.14518615778179544 ) ) ;
#9966 = DIRECTION ( 'NONE',  ( 0.000000000000000000, 0.000000000000000000, -1.000000000000000000 ) ) ;
#9967 = CARTESIAN_POINT ( 'NONE',  ( 102.4999999999999858, 123.7999999999999972, -9.847140817659276890E-15 ) ) ;
#9968 = CARTESIAN_POINT ( 'NONE',  ( 204.2950502721270425, 32.31835937608393294, 9.295050272127046043 ) ) ;
#9969 = CONTEXT_DEPENDENT_SHAPE_REPRESENTATION ( #17523, #16228 ) ;
#9970 = CARTESIAN_POINT ( 'NONE',  ( 104.9999999999999716, 1.449011120738813565E-14, 9.500000000000000000 ) ) ;
#9971 = CARTESIAN_POINT ( 'NONE',  ( 103.1528011352953342, 3.152801135295383084, 6.312500001365592084 ) ) ;
#9972 = CARTESIAN_POINT ( 'NONE',  ( 107.0000000000000142, 112.2744378736303190, -53.40000000546236691 ) ) ;
#9973 = CARTESIAN_POINT ( 'NONE',  ( 95.54126587499996504, 1.387778780781445676E-14, 9.437500001365593860 ) ) ;
#9974 = CARTESIAN_POINT ( 'NONE',  ( 99.99999999999998579, 102.6397644303321215, -48.00000000546237544 ) ) ;
#9975 =( GEOMETRIC_REPRESENTATION_CONTEXT ( 3 ) GLOBAL_UNCERTAINTY_ASSIGNED_CONTEXT ( ( #15526 ) ) GLOBAL_UNIT_ASSIGNED_CONTEXT ( ( #1949, #26309, #8913 ) ) REPRESENTATION_CONTEXT ( 'NONE', 'WORKASPACE' ) );
#9976 = CARTESIAN_POINT ( 'NONE',  ( 104.4587341249999923, 94.62499999863439371, -1.846868145590737198 ) ) ;
#9977 = DIRECTION ( 'NONE',  ( 0.000000000000000000, 0.000000000000000000, -1.000000000000000000 ) ) ;
#9978 = COLOUR_RGB ( '', 0.31764706, 0.68627451, 0.89019608) ;
#9979 = CARTESIAN_POINT ( 'NONE',  ( 114.9999999999999858, 100.0000000000000000, -15.00000000000000711 ) ) ;
#9980 = CARTESIAN_POINT ( 'NONE',  ( -5.444914386472299306, 32.16953125108393152, 13.14518615778179722 ) ) ;
#9981 = ORIENTED_EDGE ( 'NONE', *, *, #21320, .T. ) ;
#9982 = CARTESIAN_POINT ( 'NONE',  ( 98.15313185440925281, 82.50000000136560629, -4.458734125000016313 ) ) ;
#9983 = CARTESIAN_POINT ( 'NONE',  ( 99.99999999999998579, 123.3000000021849587, -2.499999999999997780 ) ) ;
#9984 = ADVANCED_FACE ( 'NONE', ( #14496 ), #27495, .T. ) ;
#9985 = CARTESIAN_POINT ( 'NONE',  ( 195.0000000000000000, 34.00507812608393721, -13.14518615778179544 ) ) ;
#9986 = ORIENTED_EDGE ( 'NONE', *, *, #3286, .F. ) ;
#9987 = CARTESIAN_POINT ( 'NONE',  ( 201.9023785737630590, 51.13402819307176372, -15.00000000000129852 ) ) ;
#9988 = CARTESIAN_POINT ( 'NONE',  ( 101.8468681455906903, 4.458734125000016313, 5.375000001365592972 ) ) ;
#9989 = EDGE_LOOP ( 'NONE', ( #22899, #11457 ) ) ;
#9990 = CARTESIAN_POINT ( 'NONE',  ( 93.46109445667491400, 114.7507929638356785, -47.57500000273119412 ) ) ;
#9991 = CARTESIAN_POINT ( 'NONE',  ( -8.049105076161786076E-16, 34.79882812608393294, -13.14518615778179544 ) ) ;
#9992 = CARTESIAN_POINT ( 'NONE',  ( -8.312177448680279460E-16, 36.13828125216787157, -13.57481594606304576 ) ) ;
#9993 = CIRCLE ( 'NONE', #10434, 4.999999999999997335 ) ;
#9994 = B_SPLINE_CURVE_WITH_KNOTS ( 'NONE', 3,
 ( #21144, #1631, #25560, #6041, #23704, #15264, #17559, #21854, #12842, #10986, #21569, #25836, #23841, #13403, #10577, #2044, #10848, #8446 ),
 .UNSPECIFIED., .F., .F.,
 ( 4, 2, 2, 2, 2, 2, 2, 2, 4 ),
 ( 0.000000000000000000, 0.004618502246277155811, 0.006927753369415732415, 0.009237004492554308152, 0.01039163005412361424, 0.01154625561569292379, 0.01385550673883149432, 0.01616475786197006659, 0.01847400898510864059 ),
 .UNSPECIFIED. ) ;
#9995 = CARTESIAN_POINT ( 'NONE',  ( -13.14518615778179722, 37.52734375108393294, -5.444914386472297529 ) ) ;
#9996 = CARTESIAN_POINT ( 'NONE',  ( -9.295050272127044266, 31.92148437608393508, 9.295050272127047819 ) ) ;
#9997 = CARTESIAN_POINT ( 'NONE',  ( 103.1528011352953484, 93.43749999863440792, 3.152801135295352886 ) ) ;
#9998 = DIRECTION ( 'NONE',  ( -0.000000000000000000, 1.000000000000000000, -0.000000000000000000 ) ) ;
#9999 = VECTOR ( 'NONE', #24998, 1000.000000000000000 ) ;
#10000 = CARTESIAN_POINT ( 'NONE',  ( 99.99999999999998579, 110.0000000000000000, -145.0000000000000284 ) ) ;
#10001 = CARTESIAN_POINT ( 'NONE',  ( -13.14518615778179900, 34.35234375108393579, -5.444914386472297529 ) ) ;
#10002 = CARTESIAN_POINT ( 'NONE',  ( 104.4587341249999781, 1.846868145590750521, 2.250000001365592084 ) ) ;
#10003 = CARTESIAN_POINT ( 'NONE',  ( 95.54126587499996504, 84.68750000136560629, -1.387778780781445676E-14 ) ) ;
#10004 = CARTESIAN_POINT ( 'NONE',  ( -13.14518615778179189, 37.42812500108393436, 5.444914386472304635 ) ) ;
#10005 = CARTESIAN_POINT ( 'NONE',  ( 84.99999999999998579, 95.00000000000000000, 14.99999999999999467 ) ) ;
#10006 = CARTESIAN_POINT ( 'NONE',  ( 93.00000000000000000, 110.0000000000000000, -55.00000000000000711 ) ) ;
#10007 = VERTEX_POINT ( 'NONE', #10211 ) ;
#10008 = CARTESIAN_POINT ( 'NONE',  ( 6.944426393311537993, 31.75150625057403175, -11.16113171639042356 ) ) ;
#10009 =( BOUNDED_CURVE ( )  B_SPLINE_CURVE ( 2, ( #18140, #26853, #7301, #24702, #5182, #13845, #25119, #16282, #9727 ),
 .UNSPECIFIED., .F., .F. ) 
 B_SPLINE_CURVE_WITH_KNOTS ( ( 3, 2, 2, 2, 3 ),
 ( 0.3958333333333331483, 0.4062499999999999445, 0.4166666666666667407, 0.4270833333333335369, 0.4375000000000003331 ),
 .UNSPECIFIED. ) 
 CURVE ( )  GEOMETRIC_REPRESENTATION_ITEM ( )  RATIONAL_B_SPLINE_CURVE ( ( 1.000000000000001110, 0.9238795325112855172, 1.000000000000000000, 0.9238795325112867385, 1.000000000000000000, 0.9238795325112867385, 1.000000000000000000, 0.9238795325112842960, 1.000000000000002442 ) ) 
 REPRESENTATION_ITEM ( '' )  );
#10011 = EDGE_CURVE ( 'NONE', #7715, #5951, #1247, .T. ) ;
#10010 = CARTESIAN_POINT ( 'NONE',  ( 102.0669872999999939, 124.1000000010924964, 0.8561741729129311862 ) ) ;
#10012 = CARTESIAN_POINT ( 'NONE',  ( 98.15313185440923860, 92.87499999863439371, -4.458734124999994997 ) ) ;
#10013 = CARTESIAN_POINT ( 'NONE',  ( 104.9999999999999716, 1.449011120738813565E-14, 34.79898987322334136 ) ) ;
#10014 = CARTESIAN_POINT ( 'NONE',  ( 93.46109445667489979, 105.2492070361643215, -53.67499999726882720 ) ) ;
#10015 = AXIS2_PLACEMENT_3D ( 'NONE', #3266, #11933, #9807 ) ;
#10016 = CARTESIAN_POINT ( 'NONE',  ( 116.4251840539369596, 39.46210937716787726, -5.622872871577872189 ) ) ;
#10017 = ORIENTED_EDGE ( 'NONE', *, *, #17241, .F. ) ;
#10018 = CARTESIAN_POINT ( 'NONE',  ( 55.70494972787295751, 38.27148437608393294, -9.295050272127046043 ) ) ;
#10019 = EDGE_CURVE ( 'NONE', #10042, #7430, #8932, .T. ) ;
#10020 = FACE_OUTER_BOUND ( 'NONE', #27839, .T. ) ;
#10021 = CYLINDRICAL_SURFACE ( 'NONE', #8939, 13.57481594606304398 ) ;
#10022 = ORIENTED_EDGE ( 'NONE', *, *, #19598, .T. ) ;
#10023 = CARTESIAN_POINT ( 'NONE',  ( 0.000000000000000000, 10.00000000000000000, 0.000000000000000000 ) ) ;
#10024 = FACE_OUTER_BOUND ( 'NONE', #13804, .T. ) ;
#10025 = EDGE_CURVE ( 'NONE', #26363, #13933, #9951, .T. ) ;
#10026 = CARTESIAN_POINT ( 'NONE',  ( 120.4011555911795455, 38.02343750216788010, 9.598844408820459861 ) ) ;
#10027 = CARTESIAN_POINT ( 'NONE',  ( 181.8548138422182205, 40.65273437608393436, 0.000000000000000000 ) ) ;
#10028 = DIRECTION ( 'NONE',  ( -0.000000000000000000, -1.000000000000000000, -0.000000000000000000 ) ) ;
#10029 = CARTESIAN_POINT ( 'NONE',  ( 185.7049497278729575, 39.26367187608393294, 9.295050272127047819 ) ) ;
#10030 = EDGE_LOOP ( 'NONE', ( #27398, #21276, #17893, #1381 ) ) ;
#10031 = CARTESIAN_POINT ( 'NONE',  ( 95.54126587499995082, -1.846868145590724986, 1.500000001365591418 ) ) ;
#10032 = CARTESIAN_POINT ( 'NONE',  ( 95.54126587499996504, 1.846868145590750077, 14.62500000136559208 ) ) ;
#10033 = CARTESIAN_POINT ( 'NONE',  ( 2.493653234604083739E-15, 40.40468749999999432, 13.57481594606304576 ) ) ;
#10034 = CYLINDRICAL_SURFACE ( 'NONE', #17423, 13.57481594606304398 ) ;
#10035 = CARTESIAN_POINT ( 'NONE',  ( 92.99999999999998579, 110.0000000000000000, -47.00000000000001421 ) ) ;
#10036 = SURFACE_SIDE_STYLE ('',( #23031 ) ) ;
#10037 = CARTESIAN_POINT ( 'NONE',  ( 5.444914386472302859, 39.41250000108393436, 13.14518615778179189 ) ) ;
#10038 = CARTESIAN_POINT ( 'NONE',  ( 97.92893218813445344, 81.18750000000001421, 4.999999999999948486 ) ) ;
#10039 = CARTESIAN_POINT ( 'NONE',  ( 12.66784425494550703, 36.00000000000000711, 4.396229039744191880 ) ) ;
#10040 = FACE_OUTER_BOUND ( 'NONE', #2457, .T. ) ;
#10041 = CARTESIAN_POINT ( 'NONE',  ( 108.0825317500000011, 110.0000000000000000, -48.62499999726882294 ) ) ;
#10042 = VERTEX_POINT ( 'NONE', #25483 ) ;
#10043 = ORIENTED_EDGE ( 'NONE', *, *, #11067, .T. ) ;
#10044 = PRODUCT_DEFINITION_CONTEXT ( 'detailed design', #24064, 'design' ) ;
#10045 = SHAPE_REPRESENTATION ( 'Integrated Vacuum Pressure Gauge', ( #26844 ), #7245 ) ;
#10046 = CARTESIAN_POINT ( 'NONE',  ( 5.622872871577871301, 39.16445312499999432, -13.57481594606304753 ) ) ;
#10047 = CARTESIAN_POINT ( 'NONE',  ( -8.049105076161786076E-16, 39.56132812608393579, -13.14518615778179544 ) ) ;
#10048 = CARTESIAN_POINT ( 'NONE',  ( 94.99999999999995737, 2.071067811865491048, 7.062500002731185944 ) ) ;
#10049 = CARTESIAN_POINT ( 'NONE',  ( 139.2950502721270425, 40.45429687608393721, -9.295050272127046043 ) ) ;
#10050 = CARTESIAN_POINT ( 'NONE',  ( 70.44491438647230552, 36.03906250108394005, 13.14518615778179189 ) ) ;
#10051 = EDGE_CURVE ( 'NONE', #20981, #23148, #3444, .T. ) ;
#10052 = LINE ( 'NONE', #22910, #27988 ) ;
#10053 = CARTESIAN_POINT ( 'NONE',  ( 9.295050272127046043, 37.87460937608393152, -9.295050272127046043 ) ) ;
#10054 = CARTESIAN_POINT ( 'NONE',  ( 97.50000000000000000, 124.2500000021849758, -1.035533905932742416 ) ) ;
#10055 = CARTESIAN_POINT ( 'NONE',  ( 99.99999999999998579, 128.0000000000000000, -5.204170427930421283E-15 ) ) ;
#10056 = CARTESIAN_POINT ( 'NONE',  ( 97.92893218813446765, 82.18750000000001421, 4.999999999999962697 ) ) ;
#10057 = CARTESIAN_POINT ( 'NONE',  ( 208.1451861577817795, 32.16953125108393152, 5.444914386472293977 ) ) ;
#10058 = CARTESIAN_POINT ( 'NONE',  ( 142.3201169669889339, 36.00000000000002132, -5.704949255836478272 ) ) ;
#10059 = CARTESIAN_POINT ( 'NONE',  ( 101.0355339059327378, 123.6569999999781544, 2.499999999999977796 ) ) ;
#10060 = CARTESIAN_POINT ( 'NONE',  ( 99.99999999999998579, 123.3500000010924680, 2.066987299999980099 ) ) ;
#10061 = FACE_OUTER_BOUND ( 'NONE', #2055, .T. ) ;
#10062 = CARTESIAN_POINT ( 'NONE',  ( 214.9999999999999716, 75.00000000000000000, 14.99999999999994493 ) ) ;
#10063 = CARTESIAN_POINT ( 'NONE',  ( 96.84719886470459471, -3.152801135295355994, 12.56250000136559208 ) ) ;
#10064 = CARTESIAN_POINT ( 'NONE',  ( 94.99999999999995737, 1.387778780781445676E-14, 13.12500000273118417 ) ) ;
#10065 = ORIENTED_EDGE ( 'NONE', *, *, #12967, .T. ) ;
#10066 = FACE_OUTER_BOUND ( 'NONE', #23838, .T. ) ;
#10067 = CARTESIAN_POINT ( 'NONE',  ( 13.57481594606304753, 40.65273437499998721, -5.622872871577873077 ) ) ;
#10068 = CARTESIAN_POINT ( 'NONE',  ( -13.57481594606304576, 40.99999999999999289, 0.000000000000000000 ) ) ;
#10069 = CARTESIAN_POINT ( 'NONE',  ( -13.57481594606304576, 31.62382812716787228, 5.622872871577880183 ) ) ;
#10070 = CARTESIAN_POINT ( 'NONE',  ( 96.46446609406721961, 80.12500000000000000, 3.535533905932727539 ) ) ;
#10071 = CARTESIAN_POINT ( 'NONE',  ( 103.1528011352953342, 81.06250000136559208, -3.152801135295383084 ) ) ;
#10072 = CARTESIAN_POINT ( 'NONE',  ( 59.55508561352770158, 37.72578125108395142, 13.14518615778179722 ) ) ;
#10073 = CARTESIAN_POINT ( 'NONE',  ( 91.91746824999998466, 112.6261737610028320, -47.47500000273119269 ) ) ;
#10074 = DIRECTION ( 'NONE',  ( 0.000000000000000000, 0.000000000000000000, 1.000000000000000000 ) ) ;
#10075 = CARTESIAN_POINT ( 'NONE',  ( 98.53841926354351699, 123.8500000010924680, -1.461580736456474794 ) ) ;
#10076 = CARTESIAN_POINT ( 'NONE',  ( 13.57481594606304931, 33.40976562499999858, 5.622872871577868636 ) ) ;
#10077 = CARTESIAN_POINT ( 'NONE',  ( 97.83688103937535629, 116.6573956140660897, -50.89999999453764445 ) ) ;
#10078 = CARTESIAN_POINT ( 'NONE',  ( 120.7049497278729575, 33.50898437608393010, -9.295050272127046043 ) ) ;
#10079 = VERTEX_POINT ( 'NONE', #21208 ) ;
#10080 = CARTESIAN_POINT ( 'NONE',  ( 107.0000000000000142, 107.7255621263696952, -51.59999999453763309 ) ) ;
#10081 = CARTESIAN_POINT ( 'NONE',  ( 99.99999999999998579, 90.00000000000000000, -6.938893903907228378E-15 ) ) ;
#10082 = CARTESIAN_POINT ( 'NONE',  ( -8.312177448680279460E-16, 39.31328125216787583, -13.57481594606304576 ) ) ;
#10083 = CARTESIAN_POINT ( 'NONE',  ( 143.1451861577818079, 38.56914062608393579, -1.609821015232357215E-15 ) ) ;
#10084 = CARTESIAN_POINT ( 'NONE',  ( 59.37712712842213136, 37.27929687716787299, 13.57481594606304753 ) ) ;
#10085 = CARTESIAN_POINT ( 'NONE',  ( -20.00000000000000000, 55.00000000000000000, 10.00000000000000000 ) ) ;
#10086 = CARTESIAN_POINT ( 'NONE',  ( -9.598844408820458085, 40.20625000216787726, -9.598844408820458085 ) ) ;
#10087 = ORIENTED_EDGE ( 'NONE', *, *, #25360, .F. ) ;
#10088 = CARTESIAN_POINT ( 'NONE',  ( 104.9999999999999574, 2.071067811865491937, 7.562499999999999112 ) ) ;
#10089 = VERTEX_POINT ( 'NONE', #18656 ) ;
#10090 = CARTESIAN_POINT ( 'NONE',  ( -5.444914386472297529, 34.25312500108393010, -13.14518615778179900 ) ) ;
#10091 = CARTESIAN_POINT ( 'NONE',  ( 185.4011555911795597, 32.46718750216787441, 9.598844408820459861 ) ) ;
#10092 = CARTESIAN_POINT ( 'NONE',  ( 0.000000000000000000, 40.99999999999999289, -13.57481594606304576 ) ) ;
#10093 = CARTESIAN_POINT ( 'NONE',  ( 97.92893218813451028, 5.000000000000018652, 13.93750000273118772 ) ) ;
#10094 = CARTESIAN_POINT ( 'NONE',  ( 116.8548138422182205, 37.32890625108393579, -5.444914386472297529 ) ) ;
#10095 = CARTESIAN_POINT ( 'NONE',  ( 6.944426393311538881, 31.75150625057403175, -11.16113171639042356 ) ) ;
#10096 = EDGE_CURVE ( 'NONE', #23999, #20385, #17050, .T. ) ;
#10097 = CYLINDRICAL_SURFACE ( 'NONE', #15413, 12.50000000000001599 ) ;
#10098 = CARTESIAN_POINT ( 'NONE',  ( 101.8468681455907330, 93.12499999863439371, 4.458734124999980786 ) ) ;
#10099 = CARTESIAN_POINT ( 'NONE',  ( 98.53841926354351699, 123.0500000010924850, -1.461580736456474794 ) ) ;
#10100 = CARTESIAN_POINT ( 'NONE',  ( 208.5748159460630120, 38.27148437500000711, -5.622872871577873077 ) ) ;
#10101 = SHAPE_DEFINITION_REPRESENTATION ( #13995, #9145 ) ;
#10102 = DIRECTION ( 'NONE',  ( 0.000000000000000000, -1.000000000000000000, -0.000000000000000000 ) ) ;
#10103 = CARTESIAN_POINT ( 'NONE',  ( 96.84719886470459471, -3.152801135295355994, 4.812500001365592084 ) ) ;
#10104 = CARTESIAN_POINT ( 'NONE',  ( 103.1528011352953342, 3.152801135295383084, 7.062500001365592084 ) ) ;
#10105 = CARTESIAN_POINT ( 'NONE',  ( 102.1631189606246295, 103.3426043859339103, -45.90000000546237402 ) ) ;
#10106 = CARTESIAN_POINT ( 'NONE',  ( 99.99999999999998579, 92.81249999863440792, -4.458734124999994997 ) ) ;
#10107 = CARTESIAN_POINT ( 'NONE',  ( -12.73839015785546813, 35.99999999999998579, 3.273369733618573196 ) ) ;
#10108 = CARTESIAN_POINT ( 'NONE',  ( 13.57481594606304576, 39.80937499999999574, -1.662435489736055892E-15 ) ) ;
#10109 = ORIENTED_EDGE ( 'NONE', *, *, #6660, .T. ) ;
#10110 = CARTESIAN_POINT ( 'NONE',  ( 99.99999999999995737, 81.43750000136559208, -4.458734125000016313 ) ) ;
#10111 = CARTESIAN_POINT ( 'NONE',  ( 99.99999999999998579, 124.1000000021849416, -2.499999999999997780 ) ) ;
#10112 = ORIENTED_EDGE ( 'NONE', *, *, #5547, .T. ) ;
#10113 = VECTOR ( 'NONE', #9655, 1000.000000000000000 ) ;
#10114 =( BOUNDED_CURVE ( )  B_SPLINE_CURVE ( 2, ( #9483, #18184, #16178, #22757, #9342 ),
 .UNSPECIFIED., .F., .T. ) 
 B_SPLINE_CURVE_WITH_KNOTS ( ( 3, 2, 3 ),
 ( 0.9500000000000009548, 0.9750000000000005329, 1.000000000000000000 ),
 .UNSPECIFIED. ) 
 CURVE ( )  GEOMETRIC_REPRESENTATION_ITEM ( )  RATIONAL_B_SPLINE_CURVE ( ( 0.9999999999999970024, 0.9238795325112897361, 1.000000000000000000, 0.9238795325112867385, 1.000000000000000000 ) ) 
 REPRESENTATION_ITEM ( '' )  );
#10115 = ORIENTED_EDGE ( 'NONE', *, *, #1016, .F. ) ;
#10116 = CARTESIAN_POINT ( 'NONE',  ( 189.6762090360452646, 54.47170356488337006, -15.00000000000000000 ) ) ;
#10117 = CARTESIAN_POINT ( 'NONE',  ( 95.54126587499995082, -1.846868145590724986, 5.750000001365591196 ) ) ;
#10118 = ORIENTED_EDGE ( 'NONE', *, *, #6887, .T. ) ;
#10119 = CARTESIAN_POINT ( 'NONE',  ( 95.00472066334982912, 103.1245878333314323, -49.07500000273118701 ) ) ;
#10120 = CARTESIAN_POINT ( 'NONE',  ( -9.295050272127046043, 34.89804687608393152, -9.295050272127046043 ) ) ;
#10121 = CARTESIAN_POINT ( 'NONE',  ( 208.5748159460630120, 39.85898437716787157, 5.622872871577869525 ) ) ;
#10122 = CARTESIAN_POINT ( 'NONE',  ( 9.295050272127047819, 39.26367187608393294, 9.295050272127046043 ) ) ;
#10123 = CARTESIAN_POINT ( 'NONE',  ( 108.0825317500000011, 112.6261737610028320, -46.02500000273120406 ) ) ;
#10124 = CARTESIAN_POINT ( 'NONE',  ( 116.8548138422182205, 39.21406250108392300, 5.444914386472304635 ) ) ;
#10125 = CARTESIAN_POINT ( 'NONE',  ( 5.444914386472302859, 40.20625000108394431, 13.14518615778179189 ) ) ;
#10126 = EDGE_CURVE ( 'NONE', #20676, #4003, #27515, .T. ) ;
#10127 = ORIENTED_EDGE ( 'NONE', *, *, #9511, .F. ) ;
#10128 = CARTESIAN_POINT ( 'NONE',  ( 78.57481594606305464, 39.01562500000000000, -1.662435489736055892E-15 ) ) ;
#10129 = CARTESIAN_POINT ( 'NONE',  ( 55.40115559117954547, 39.61093750216787868, 9.598844408820459861 ) ) ;
#10130 = FACE_OUTER_BOUND ( 'NONE', #4177, .T. ) ;
#10131 = CARTESIAN_POINT ( 'NONE',  ( 5.444914386472302859, 32.26875000108393721, 13.14518615778179189 ) ) ;
#10132 = CARTESIAN_POINT ( 'NONE',  ( 101.8468681455907046, -4.458734124999987891, 3.000000001365592528 ) ) ;
#10133 = CARTESIAN_POINT ( 'NONE',  ( 95.54126587499996504, 82.68750000136560629, -1.387778780781445676E-14 ) ) ;
#10134 = CARTESIAN_POINT ( 'NONE',  ( -9.295050272127044266, 34.30273437608393294, 9.295050272127047819 ) ) ;
#10135 = CARTESIAN_POINT ( 'NONE',  ( 13.14518615778179900, 40.40468750108393436, -5.444914386472297529 ) ) ;
#10136 = CARTESIAN_POINT ( 'NONE',  ( 9.598844408820459861, 39.01562500216787299, 9.598844408820456309 ) ) ;
#10137 = ORIENTED_EDGE ( 'NONE', *, *, #16294, .T. ) ;
#10138 =( NAMED_UNIT ( * ) SI_UNIT ( $, .STERADIAN. ) SOLID_ANGLE_UNIT ( ) );
#10139 = CARTESIAN_POINT ( 'NONE',  ( 97.83688103937537051, 103.3426043859339103, -54.09999999453764019 ) ) ;
#10140 = CARTESIAN_POINT ( 'NONE',  ( 103.1528011352953484, 95.43749999863440792, 3.152801135295352886 ) ) ;
#10141 = CARTESIAN_POINT ( 'NONE',  ( 95.27063293749995410, 1.387778780781445676E-14, 0.8437500006827957089 ) ) ;
#10142 = DIRECTION ( 'NONE',  ( -1.000000000000000000, -0.000000000000000000, 2.385244779468110248E-16 ) ) ;
#10143 = DIRECTION ( 'NONE',  ( -0.000000000000000000, -0.000000000000000000, -1.000000000000000000 ) ) ;
#10144 = ORIENTED_EDGE ( 'NONE', *, *, #13111, .F. ) ;
#10145 = CARTESIAN_POINT ( 'NONE',  ( 74.29505027212704249, 37.27929687608394005, -9.295050272127046043 ) ) ;
#10146 = CARTESIAN_POINT ( 'NONE',  ( 97.93301270000000613, 123.1000000010924822, -0.8561741729129506151 ) ) ;
#10147 = CARTESIAN_POINT ( 'NONE',  ( 181.8548138422181921, 32.07031250108393294, 5.444914386472304635 ) ) ;
#10148 = CIRCLE ( 'NONE', #23386, 12.50000000000001599 ) ;
#10149 = ADVANCED_FACE ( 'NONE', ( #6098 ), #8365, .T. ) ;
#10150 = EDGE_LOOP ( 'NONE', ( #21701, #18151, #27372, #16438 ) ) ;
#10151 = CARTESIAN_POINT ( 'NONE',  ( 84.99999999999998579, 102.0000000000000142, -15.00000000000000711 ) ) ;
#10152 = CARTESIAN_POINT ( 'NONE',  ( -8.259611528891891652, 50.00000000056336802, -10.79618466885709083 ) ) ;
#10153 = CARTESIAN_POINT ( 'NONE',  ( 204.1801758136480203, 55.00000000000000000, 14.99999999999994671 ) ) ;
#10154 = CARTESIAN_POINT ( 'NONE',  ( 120.4011555911795455, 33.26093750216787726, 9.598844408820459861 ) ) ;
#10155 = CARTESIAN_POINT ( 'NONE',  ( 103.5355339059327235, 90.12500000000000000, -3.535533905932738197 ) ) ;
#10156 = EDGE_CURVE ( 'NONE', #58, #18296, #5870, .T. ) ;
#10157 = FACE_OUTER_BOUND ( 'NONE', #25274, .T. ) ;
#10158 = CARTESIAN_POINT ( 'NONE',  ( 208.1451861577817795, 36.43593750108392726, -5.444914386472297529 ) ) ;
#10159 = VERTEX_POINT ( 'NONE', #19481 ) ;
#10160 = EDGE_CURVE ( 'NONE', #8859, #12194, #21627, .T. ) ;
#10161 =( BOUNDED_CURVE ( )  B_SPLINE_CURVE ( 2, ( #10795, #19935, #8815, #4692, #13061, #11077, #19509, #8534, #15209 ),
 .UNSPECIFIED., .F., .F. ) 
 B_SPLINE_CURVE_WITH_KNOTS ( ( 3, 2, 2, 2, 3 ),
 ( 0.06250000000000004163, 0.07291666666666665741, 0.08333333333333325932, 0.09374999999999987510, 0.1041666666666664909 ),
 .UNSPECIFIED. ) 
 CURVE ( )  GEOMETRIC_REPRESENTATION_ITEM ( )  RATIONAL_B_SPLINE_CURVE ( ( 0.9999999999999996669, 0.9238795325112870716, 1.000000000000000000, 0.9238795325112867385, 1.000000000000000000, 0.9238795325112867385, 1.000000000000000000, 0.9238795325112880708, 0.9999999999999986677 ) ) 
 REPRESENTATION_ITEM ( '' )  );
#10162 =( LENGTH_UNIT ( ) NAMED_UNIT ( * ) SI_UNIT ( .MILLI., .METRE. ) );
#10163 = PLANE ( 'NONE',  #4817 ) ;
#10164 = CARTESIAN_POINT ( 'NONE',  ( 95.00000000000000000, 92.43749999726880162, 2.071067811865463959 ) ) ;
#10165 = EDGE_CURVE ( 'NONE', #9633, #25436, #17685, .T. ) ;
#10166 = CARTESIAN_POINT ( 'NONE',  ( 181.8548138422182205, 40.55351562608393579, 0.000000000000000000 ) ) ;
#10167 = CARTESIAN_POINT ( 'NONE',  ( -5.444914386472297529, 39.80937500108393579, -13.14518615778179722 ) ) ;
#10168 = CARTESIAN_POINT ( 'NONE',  ( 102.0669872999999797, 122.7500000010924737, -9.794112055954760458E-15 ) ) ;
#10169 = CARTESIAN_POINT ( 'NONE',  ( 87.00000000000000000, 118.0000000000000000, -43.00000000000000000 ) ) ;
#10170 = DIRECTION ( 'NONE',  ( 0.000000000000000000, 0.000000000000000000, 1.000000000000000000 ) ) ;
#10171 = CARTESIAN_POINT ( 'NONE',  ( 99.99999999999997158, 101.5015231886685854, -47.12499999726882294 ) ) ;
#10172 = EDGE_CURVE ( 'NONE', #10042, #637, #5420, .T. ) ;
#10173 = VERTEX_POINT ( 'NONE', #28179 ) ;
#10174 = CARTESIAN_POINT ( 'NONE',  ( 13.57481594606304753, 38.27148437500000711, -5.622872871577873077 ) ) ;
#10175 = CARTESIAN_POINT ( 'NONE',  ( -5.622872871577873077, 31.72304687716787441, 13.57481594606304753 ) ) ;
#10176 = ORIENTED_EDGE ( 'NONE', *, *, #12095, .T. ) ;
#10177 = CARTESIAN_POINT ( 'NONE',  ( 104.9999999999999716, 1.449011120738813565E-14, 6.625000002731185944 ) ) ;
#10178 = CARTESIAN_POINT ( 'NONE',  ( 124.5550856135277087, 38.51953125108393294, 13.14518615778179722 ) ) ;
#10179 = CARTESIAN_POINT ( 'NONE',  ( 51.85481384221819923, 37.32890625108393579, -5.444914386472297529 ) ) ;
#10180 = LINE ( 'NONE', #23459, #12491 ) ;
#10181 = CARTESIAN_POINT ( 'NONE',  ( -13.14518615778179544, 34.99726562608393721, 0.000000000000000000 ) ) ;
#10182 = CARTESIAN_POINT ( 'NONE',  ( 194.0044387749465784, 36.00000000000000000, -13.45766439703020367 ) ) ;
#10183 = LINE ( 'NONE', #1392, #6171 ) ;
#10184 = CARTESIAN_POINT ( 'NONE',  ( 217.9999999999999716, 52.00000000000000711, 12.99999999999994316 ) ) ;
#10185 = EDGE_CURVE ( 'NONE', #23121, #2928, #2524, .T. ) ;
#10186 = DIRECTION ( 'NONE',  ( -1.000000000000000000, -0.000000000000000000, 2.385244779468110248E-16 ) ) ;
#10187 = CYLINDRICAL_SURFACE ( 'NONE', #16636, 5.000000000000004441 ) ;
#10188 = CARTESIAN_POINT ( 'NONE',  ( 13.14518615778179900, 39.31328125108392868, 5.444914386472293977 ) ) ;
#10189 = CARTESIAN_POINT ( 'NONE',  ( 99.99999999999995737, 85.00000000000000000, -5.000000000000018652 ) ) ;
#10190 = CARTESIAN_POINT ( 'NONE',  ( 101.7677669529663547, 124.7000000000000028, -1.767766952966370209 ) ) ;
#10191 = CARTESIAN_POINT ( 'NONE',  ( 98.53841926354351699, 123.2500000010924737, 1.461580736456455920 ) ) ;
#10192 = CARTESIAN_POINT ( 'NONE',  ( 97.93301270000000613, 124.0000000010924879, 0.8561741729129328515 ) ) ;
#10193 = AXIS2_PLACEMENT_3D ( 'NONE', #27944, #23389, #17236 ) ;
#10194 = EDGE_CURVE ( 'NONE', #18726, #17053, #22602, .T. ) ;
#10195 = CARTESIAN_POINT ( 'NONE',  ( 195.0000000000000000, -7.395377635281828788, -13.57481594606306707 ) ) ;
#10196 = CARTESIAN_POINT ( 'NONE',  ( 99.99999999999995737, -4.458734124999988779, 13.68750000136559208 ) ) ;
#10197 = CARTESIAN_POINT ( 'NONE',  ( -13.57481594606304576, 32.31835937499999289, 5.622872871577880183 ) ) ;
#10198 = VERTEX_POINT ( 'NONE', #11186 ) ;
#10199 = DIRECTION ( 'NONE',  ( -1.000000000000000000, 0.000000000000000000, 0.000000000000000000 ) ) ;
#10200 =( BOUNDED_CURVE ( )  B_SPLINE_CURVE ( 2, ( #19559, #2464, #14985, #13255, #2042, #10711, #21986, #6580, #21710 ),
 .UNSPECIFIED., .F., .F. ) 
 B_SPLINE_CURVE_WITH_KNOTS ( ( 3, 2, 2, 2, 3 ),
 ( 0.4642857142857142461, 0.4732142857142856429, 0.4821428571428570953, 0.4910714285714285476, 0.5000000000000000000 ),
 .UNSPECIFIED. ) 
 CURVE ( )  GEOMETRIC_REPRESENTATION_ITEM ( )  RATIONAL_B_SPLINE_CURVE ( ( 1.000000000000000444, 0.9238795325112862944, 1.000000000000000000, 0.9238795325112867385, 1.000000000000000000, 0.9238795325112867385, 1.000000000000000000, 0.9238795325112867385, 1.000000000000000000 ) ) 
 REPRESENTATION_ITEM ( '' )  );
#10201 = CARTESIAN_POINT ( 'NONE',  ( 13.57481594606304753, 39.06523437499998863, -5.622872871577873077 ) ) ;
#10202 = CARTESIAN_POINT ( 'NONE',  ( 2.414731522848535132E-15, 33.60820312608392868, 13.14518615778179544 ) ) ;
#10203 = EDGE_CURVE ( 'NONE', #21009, #9571, #388, .T. ) ;
#10204 = CARTESIAN_POINT ( 'NONE',  ( -8.312177448680279460E-16, 32.16953125216787157, -13.57481594606304576 ) ) ;
#10205 = CARTESIAN_POINT ( 'NONE',  ( 93.00000000000000000, 110.0000000000000000, -52.00000000000000711 ) ) ;
#10206 = CARTESIAN_POINT ( 'NONE',  ( 103.1528011352953342, 83.31250000136560629, -3.152801135295383084 ) ) ;
#10207 = CARTESIAN_POINT ( 'NONE',  ( 70.44491438647230552, 37.32890625108393579, -13.14518615778179900 ) ) ;
#10208 = CARTESIAN_POINT ( 'NONE',  ( 97.50236033167492167, 102.3130555110000159, -50.97500000273119980 ) ) ;
#10209 = CARTESIAN_POINT ( 'NONE',  ( 102.0710678118653902, 94.18749999999998579, -5.000000000000047073 ) ) ;
#10210 = CARTESIAN_POINT ( 'NONE',  ( 102.0669872999999939, 122.6000000010924964, -0.8561741729129507261 ) ) ;
#10211 = CARTESIAN_POINT ( 'NONE',  ( 130.0000000000000000, 36.83281249999999574, -13.57481594606304576 ) ) ;
#10212 = CARTESIAN_POINT ( 'NONE',  ( 94.33688103937534208, 114.1144967660473242, -54.69999999453764161 ) ) ;
#10213 = CARTESIAN_POINT ( 'NONE',  ( 120.7049497278729575, 32.71523437608393436, -9.295050272127046043 ) ) ;
#10214 = ORIENTED_EDGE ( 'NONE', *, *, #19041, .F. ) ;
#10215 = CARTESIAN_POINT ( 'NONE',  ( 130.0000000000000000, 37.72578125216787726, -13.57481594606304576 ) ) ;
#10216 = DIRECTION ( 'NONE',  ( 0.000000000000000000, 1.000000000000000000, 0.000000000000000000 ) ) ;
#10217 = CARTESIAN_POINT ( 'NONE',  ( 95.54126587499996504, 79.43750000136559208, -1.387778780781445676E-14 ) ) ;
#10218 = CARTESIAN_POINT ( 'NONE',  ( -13.57481594606304576, 40.65273437608393436, 0.000000000000000000 ) ) ;
#10219 = CARTESIAN_POINT ( 'NONE',  ( 65.00000000000000000, 38.12265625216787157, 13.57481594606304576 ) ) ;
#10220 = AXIS2_PLACEMENT_3D ( 'NONE', #24759, #5239, #27051 ) ;
#10221 = CARTESIAN_POINT ( 'NONE',  ( 99.99999999999997158, 101.5015231886685854, -51.12499999726882294 ) ) ;
#10222 = CARTESIAN_POINT ( 'NONE',  ( -13.57481594606304576, 36.38632812716788578, 5.622872871577880183 ) ) ;
#10223 = VERTEX_POINT ( 'NONE', #2102 ) ;
#10224 = CARTESIAN_POINT ( 'NONE',  ( 94.99999999999995737, 2.071067811865491048, 10.93749999999999822 ) ) ;
#10225 = ORIENTED_EDGE ( 'NONE', *, *, #2205, .T. ) ;
#10226 = CARTESIAN_POINT ( 'NONE',  ( 6.944426393311538881, 31.75150625057403175, -11.16113171639042356 ) ) ;
#10227 = CARTESIAN_POINT ( 'NONE',  ( 208.1451861577818079, 36.98164062608393010, -1.609821015232357215E-15 ) ) ;
#10228 = CARTESIAN_POINT ( 'NONE',  ( 13.57481594606304931, 36.68398437716787441, 5.622872871577868636 ) ) ;
#10229 = EDGE_CURVE ( 'NONE', #6540, #18933, #23760, .T. ) ;
#10230 = CARTESIAN_POINT ( 'NONE',  ( 139.2950502721270425, 36.88242187608393152, 9.295050272127046043 ) ) ;
#10231 = CARTESIAN_POINT ( 'NONE',  ( 96.46446609406721961, 80.25000000273119838, 3.535533905932727539 ) ) ;
#10232 = CARTESIAN_POINT ( 'NONE',  ( 0.000000000000000000, 31.00000000000000000, 0.000000000000000000 ) ) ;
#10233 = CARTESIAN_POINT ( 'NONE',  ( 130.0000000000000000, -7.395377635281828788, 11.57481594606302799 ) ) ;
#10234 = CARTESIAN_POINT ( 'NONE',  ( 130.0000000000000000, -7.395377635281828788, 13.57481594606302799 ) ) ;
#10235 = CARTESIAN_POINT ( 'NONE',  ( 101.0355339059327378, 124.7500000000000142, -2.499999999999997780 ) ) ;
#10236 = CARTESIAN_POINT ( 'NONE',  ( 189.3771271284221314, 38.76757812500000000, 13.57481594606304753 ) ) ;
#10237 = ITEM_DEFINED_TRANSFORMATION ( 'NONE', 'NONE', #19023,  #26844 ) ;
#10238 = FACE_OUTER_BOUND ( 'NONE', #23359, .T. ) ;
#10239 = CARTESIAN_POINT ( 'NONE',  ( 99.99999999999995737, 4.458734125000016313, 1.437500001365592972 ) ) ;
#10240 = CARTESIAN_POINT ( 'NONE',  ( 59.55508561352770158, 37.22968750108393721, -13.14518615778179900 ) ) ;
#10241 = AXIS2_PLACEMENT_3D ( 'NONE', #23336, #25744, #23474 ) ;
#10242 = CARTESIAN_POINT ( 'NONE',  ( 95.54126587499996504, 1.846868145590750077, 4.375000001365592084 ) ) ;
#10243 = CARTESIAN_POINT ( 'NONE',  ( 93.00000000000000000, 110.0000000000000000, -50.50000000546237544 ) ) ;
#10244 = CARTESIAN_POINT ( 'NONE',  ( 101.8468681455907330, 94.74999999863440792, -4.458734124999994997 ) ) ;
#10245 = FACE_OUTER_BOUND ( 'NONE', #14370, .T. ) ;
#10246 = CARTESIAN_POINT ( 'NONE',  ( 9.598844408820459861, 38.91640624999999432, 9.598844408820456309 ) ) ;
#10247 = FACE_OUTER_BOUND ( 'NONE', #726, .T. ) ;
#10248 = EDGE_LOOP ( 'NONE', ( #9617, #8824, #1243, #15179, #1963, #650 ) ) ;
#10249 = DIRECTION ( 'NONE',  ( 0.000000000000000000, 1.000000000000000000, 0.000000000000000000 ) ) ;
#10250 = AXIS2_PLACEMENT_3D ( 'NONE', #15263, #21431, #12560 ) ;
#10251 = AXIS2_PLACEMENT_3D ( 'NONE', #1308, #9564, #16113 ) ;
#10252 = DIRECTION ( 'NONE',  ( 0.000000000000000000, 0.000000000000000000, -1.000000000000000000 ) ) ;
#10253 = VERTEX_POINT ( 'NONE', #25900 ) ;
#10254 = ORIENTED_EDGE ( 'NONE', *, *, #6847, .F. ) ;
#10255 = CARTESIAN_POINT ( 'NONE',  ( 9.598844408820456309, 32.76484374999999716, -9.598844408820458085 ) ) ;
#10256 = CARTESIAN_POINT ( 'NONE',  ( 95.54126587499995082, -1.846868145590724986, 6.750000001365592972 ) ) ;
#10257 = ORIENTED_EDGE ( 'NONE', *, *, #10, .F. ) ;
#10258 = CARTESIAN_POINT ( 'NONE',  ( 104.9952793366501851, 116.8754121666685393, -50.07500000273120122 ) ) ;
#10259 = CARTESIAN_POINT ( 'NONE',  ( 5.444914386472302859, 33.65781250108393152, 13.14518615778179189 ) ) ;
#10260 = DIRECTION ( 'NONE',  ( 0.000000000000000000, 0.000000000000000000, 1.000000000000000000 ) ) ;
#10261 = CARTESIAN_POINT ( 'NONE',  ( 2.414731522848535132E-15, 39.95820312608393010, 13.14518615778179544 ) ) ;
#10262 = CARTESIAN_POINT ( 'NONE',  ( 102.4976396683250925, 117.6869444889999841, -49.72500000273119269 ) ) ;
#10263 = CARTESIAN_POINT ( 'NONE',  ( 93.00000000000001421, 107.7255621263696668, -51.90000000000000568 ) ) ;
#10264 = CARTESIAN_POINT ( 'NONE',  ( -5.444914386472299306, 36.13828125108393152, 13.14518615778179722 ) ) ;
#10265 = CARTESIAN_POINT ( 'NONE',  ( -13.14518615778179544, 31.82226562608393650, 0.000000000000000000 ) ) ;
#10266 = EDGE_LOOP ( 'NONE', ( #7348, #9533, #16000, #15265 ) ) ;
#10267 = CARTESIAN_POINT ( 'NONE',  ( 59.37712712842213136, 38.76757812500000000, 13.57481594606304753 ) ) ;
#10268 = VECTOR ( 'NONE', #2938, 1000.000000000000000 ) ;
#10269 = FACE_OUTER_BOUND ( 'NONE', #8228, .T. ) ;
#10270 = CARTESIAN_POINT ( 'NONE',  ( 203.1931556449107177, 36.00000000000000000, 10.45682415286345446 ) ) ;
#10271 = CARTESIAN_POINT ( 'NONE',  ( 104.4587341249999639, 1.442382525525748735E-14, 4.937500001365592972 ) ) ;
#10272 = CARTESIAN_POINT ( 'NONE',  ( 13.14518615778179544, 34.00507812608393721, -1.609821015232357215E-15 ) ) ;
#10273 = CARTESIAN_POINT ( 'NONE',  ( 104.4587341249999639, 1.442382525525748735E-14, 2.187500001365592084 ) ) ;
#10274 = CARTESIAN_POINT ( 'NONE',  ( 101.8468681455907046, 83.00000000136562051, 4.458734124999987891 ) ) ;
#10275 = CARTESIAN_POINT ( 'NONE',  ( 13.14518615778179900, 32.16953125108393152, 5.444914386472293977 ) ) ;
#10276 = CARTESIAN_POINT ( 'NONE',  ( 13.14518615778179544, 38.76757812608393294, -1.609821015232357215E-15 ) ) ;
#10277 = DIRECTION ( 'NONE',  ( -1.000000000000000000, 0.000000000000000000, 0.000000000000000000 ) ) ;
#10278 = ORIENTED_EDGE ( 'NONE', *, *, #19932, .T. ) ;
#10279 =( BOUNDED_SURFACE ( )  B_SPLINE_SURFACE ( 1, 2, ( 
 ( #11826, #20549, #14248, #16254, #1031, #9702, #8120, #12509, #21381, #6260, #21098, #25511, #3718, #1993, #21513, #25642, #6125, #23376, #19511, #18949, #27658, #10382, #19367, #23789, #8254, #23514, #10797, #7978, #14791, #21238, #19231, #16814, #12656, #27932, #5991, #17077, #16677, #8391, #1720, #3993, #5856, #25376, #14656, #28070, #25782, #8536, #3849, #14526, #23241, #1860, #10524, #19089, #27797, #17222, #15070, #16941, #25927, #14933, #23654, #1586, #12379, #4129, #12795, #10660, #6401, #4265, #12925, #10240, #21657, #2133, #10937, #11361, #6814, #24214, #22222, #417, #20085, #8677, #6956, #4841, #23930, #26647, #13502, #6533, #19937, #2701, #11220, #11504, #17797, #11079, #13063, #15210, #4409, #8959, #562, #19791, #9102, #19649, #14017, #21943, #21800, #2279, #273, #4693, #7094, #17648, #17506, #26356, #2559, #131, #9243, #2836, #15503, #13354, #15651, #22082, #26499, #24350, #8817, #17936, #15793, #24496, #4981, #13647, #22362, #17368, #26064, #26207, #6670, #15356, #24071, #4547, #13209, #2421, #9664, #18367, #7378, #3545, #2970, #11645, #22653, #3395, #7814, #20514, #7525, #23067, #20221, #27073, #24780, #3264, #854, #24921, #11931, #20369, #1137, #705, #20653, #5261, #16220, #18076, #9379, #26935, #12066, #9805, #20791, #16072, #26790, #7235, #5405, #14075, #18226, #9526, #1272, #27356, #3123, #9936, #22795, #18510, #13783, #15926, #27217, #996, #25065 ),
 ( #13925, #18651, #7671, #16364, #14216, #5551, #16506, #24644, #22934, #25200, #5117, #5686, #14352, #22505, #11790, #17046, #23480, #23755, #1824, #23343, #25336, #18784, #27491, #21204, #4097, #3817, #12620, #23209, #12202, #5957, #5822, #7947, #12477, #8221, #10629, #1687, #1554, #10346, #14760, #12348, #25750, #15038, #19053, #27762, #27900, #16911, #21345, #25609, #14492, #1960, #6093, #14899, #3960, #10489, #19197, #8360, #8504, #12760, #23620, #6232, #20929, #10072, #19334, #21480, #21066, #16779, #28037, #17189, #3684, #10207, #16644, #25896, #6366, #1413, #18917, #27626, #8084, #25479, #14625, #13172, #17762, #26029, #21911, #19753, #8646, #6919, #13458, #6500, #19899, #26465, #15176, #24314, #383, #4515, #15612, #4800, #22184, #2664, #8781, #26609, #4657, #11324, #9067, #8923, #24036, #2097, #20046, #19476, #236, #525, #9206, #2519, #17900, #7055, #15322, #15754, #26319, #2244, #17335, #2386, #23895, #11044, #10765, #17611, #4233, #28175, #13030, #12891, #21621, #4374, #21767, #10906, #6780, #19615, #15465, #100, #17469, #26171, #6638, #24179, #13318, #22044, #11181, #22614, #3222, #954, #16030, #5083, #24742, #25025, #18473, #22469, #669, #7341, #18330, #3084, #1097, #5223, #9764, #13888, #2934, #5365, #11751, #1236, #20477, #815, #12029, #13745, #16326, #27317, #26750, #14175, #27181, #5507, #7773, #11604, #7483, #22892, #4942, #7632, #3357, #20327, #9625 ) ),
 .UNSPECIFIED., .F., .F., .F. ) 
 B_SPLINE_SURFACE_WITH_KNOTS ( ( 2, 2 ),
 ( 3, 2, 2, 2, 2, 2, 2, 2, 2, 2, 2, 2, 2, 2, 2, 2, 2, 2, 2, 2, 2, 2, 2, 2, 2, 2, 2, 2, 2, 2, 2, 2, 2, 2, 2, 2, 2, 2, 2, 2, 2, 2, 2, 2, 2, 2, 2, 2, 2, 2, 2, 2, 2, 2, 2, 2, 2, 2, 2, 2, 2, 2, 2, 2, 2, 2, 2, 2, 2, 2, 2, 2, 2, 2, 2, 2, 2, 2, 2, 2, 2, 2, 2, 2, 2, 2, 2, 2, 2, 2, 2, 3 ),
 ( 0.000000000000000000, 1.000000000000000000 ),
 ( 0.000000000000000000, 0.01041666666666666609, 0.02083333333333333218, 0.03125000000000000000, 0.04166666666666666435, 0.05208333333333333565, 0.06250000000000000000, 0.07291666666666667129, 0.08333333333333332871, 0.09375000000000000000, 0.1041666666666666713, 0.1145833333333333287, 0.1250000000000000000, 0.1354166666666666574, 0.1458333333333333426, 0.1562500000000000000, 0.1666666666666666574, 0.1770833333333333426, 0.1875000000000000000, 0.1979166666666666574, 0.2083333333333333426, 0.2187500000000000000, 0.2291666666666666574, 0.2395833333333333426, 0.2500000000000000000, 0.2604166666666666852, 0.2708333333333333148, 0.2812500000000000000, 0.2916666666666666852, 0.3020833333333333148, 0.3125000000000000000, 0.3229166666666666852, 0.3333333333333333148, 0.3437500000000000000, 0.3541666666666666852, 0.3645833333333333148, 0.3750000000000000000, 0.3854166666666666852, 0.3958333333333333148, 0.4062500000000000000, 0.4166666666666666852, 0.4270833333333333148, 0.4375000000000000000, 0.4479166666666666852, 0.4583333333333333148, 0.4687500000000000000, 0.4791666666666666852, 0.4895833333333333148, 0.5000000000000000000, 0.5104166666666666297, 0.5208333333333333703, 0.5312500000000000000, 0.5416666666666666297, 0.5520833333333333703, 0.5625000000000000000, 0.5729166666666666297, 0.5833333333333333703, 0.5937500000000000000, 0.6041666666666666297, 0.6145833333333333703, 0.6250000000000000000, 0.6354166666666666297, 0.6458333333333333703, 0.6562500000000000000, 0.6666666666666666297, 0.6770833333333333703, 0.6875000000000000000, 0.6979166666666666297, 0.7083333333333333703, 0.7187500000000000000, 0.7291666666666666297, 0.7395833333333333703, 0.7500000000000000000, 0.7604166666666666297, 0.7708333333333333703, 0.7812500000000000000, 0.7916666666666666297, 0.8020833333333333703, 0.8125000000000000000, 0.8229166666666666297, 0.8333333333333333703, 0.8437500000000000000, 0.8541666666666666297, 0.8645833333333333703, 0.8750000000000000000, 0.8854166666666666297, 0.8958333333333333703, 0.9062500000000000000, 0.9166666666666666297, 0.9270833333333333703, 0.9375000000000000000, 0.9448587001587775980 ),
 .UNSPECIFIED. ) 
 GEOMETRIC_REPRESENTATION_ITEM ( )  RATIONAL_B_SPLINE_SURFACE ( (
 ( 1.000000000000000000, 0.9238795325112867385, 1.000000000000000000, 0.9238795325112867385, 1.000000000000000000, 0.9238795325112867385, 1.000000000000000000, 0.9238795325112867385, 1.000000000000000000, 0.9238795325112867385, 1.000000000000000000, 0.9238795325112867385, 1.000000000000000000, 0.9238795325112867385, 1.000000000000000000, 0.9238795325112867385, 1.000000000000000000, 0.9238795325112867385, 1.000000000000000000, 0.9238795325112867385, 1.000000000000000000, 0.9238795325112867385, 1.000000000000000000, 0.9238795325112867385, 1.000000000000000000, 0.9238795325112867385, 1.000000000000000000, 0.9238795325112867385, 1.000000000000000000, 0.9238795325112867385, 1.000000000000000000, 0.9238795325112867385, 1.000000000000000000, 0.9238795325112867385, 1.000000000000000000, 0.9238795325112867385, 1.000000000000000000, 0.9238795325112867385, 1.000000000000000000, 0.9238795325112867385, 1.000000000000000000, 0.9238795325112867385, 1.000000000000000000, 0.9238795325112867385, 1.000000000000000000, 0.9238795325112867385, 1.000000000000000000, 0.9238795325112867385, 1.000000000000000000, 0.9238795325112867385, 1.000000000000000000, 0.9238795325112867385, 1.000000000000000000, 0.9238795325112867385, 1.000000000000000000, 0.9238795325112867385, 1.000000000000000000, 0.9238795325112867385, 1.000000000000000000, 0.9238795325112867385, 1.000000000000000000, 0.9238795325112867385, 1.000000000000000000, 0.9238795325112867385, 1.000000000000000000, 0.9238795325112867385, 1.000000000000000000, 0.9238795325112867385, 1.000000000000000000, 0.9238795325112867385, 1.000000000000000000, 0.9238795325112867385, 1.000000000000000000, 0.9238795325112867385, 1.000000000000000000, 0.9238795325112867385, 1.000000000000000000, 0.9238795325112867385, 1.000000000000000000, 0.9238795325112867385, 1.000000000000000000, 0.9238795325112867385, 1.000000000000000000, 0.9238795325112867385, 1.000000000000000000, 0.9238795325112867385, 1.000000000000000000, 0.9238795325112867385, 1.000000000000000000, 0.9238795325112867385, 1.000000000000000000, 0.9238795325112867385, 1.000000000000000000, 0.9238795325112867385, 1.000000000000000000, 0.9238795325112867385, 1.000000000000000000, 0.9238795325112867385, 1.000000000000000000, 0.9238795325112867385, 1.000000000000000000, 0.9238795325112867385, 1.000000000000000000, 0.9238795325112867385, 1.000000000000000000, 0.9238795325112867385, 1.000000000000000000, 0.9238795325112867385, 1.000000000000000000, 0.9238795325112867385, 1.000000000000000000, 0.9238795325112867385, 1.000000000000000000, 0.9238795325112867385, 1.000000000000000000, 0.9238795325112867385, 1.000000000000000000, 0.9238795325112867385, 1.000000000000000000, 0.9238795325112867385, 1.000000000000000000, 0.9238795325112867385, 1.000000000000000000, 0.9238795325112867385, 1.000000000000000000, 0.9238795325112867385, 1.000000000000000000, 0.9238795325112867385, 1.000000000000000000, 0.9238795325112867385, 1.000000000000000000, 0.9238795325112867385, 1.000000000000000000, 0.9238795325112867385, 1.000000000000000000, 0.9238795325112867385, 1.000000000000000000, 0.9238795325112867385, 1.000000000000000000, 0.9238795325112867385, 1.000000000000000000, 0.9238795325112867385, 1.000000000000000000, 0.9238795325112867385, 1.000000000000000000, 0.9238795325112867385, 1.000000000000000000, 0.9238795325112867385, 1.000000000000000000, 0.9238795325112867385, 1.000000000000000000, 0.9238795325112867385, 1.000000000000000000, 0.9238795325112867385, 1.000000000000000000, 0.9238795325112867385, 1.000000000000000000, 0.9238795325112867385, 1.000000000000000000, 0.9238795325112867385, 1.000000000000000000, 0.9238795325112867385, 1.000000000000000000, 0.9238795325112867385, 1.000000000000000000, 0.9238795325112867385, 1.000000000000000000, 0.9238795325112867385, 1.000000000000000000, 0.9238795325112867385, 1.000000000000000000, 0.9238795325112867385, 1.000000000000000000, 0.9238795325112867385, 1.000000000000000000, 0.9238795325112867385, 1.000000000000000000, 0.9238795325112867385, 1.000000000000000000, 0.9238795325112867385, 1.000000000000000000, 0.9462258211652395667, 0.9684275895297407288),
 ( 1.000000000000000000, 0.9238795325112867385, 1.000000000000000000, 0.9238795325112867385, 1.000000000000000000, 0.9238795325112867385, 1.000000000000000000, 0.9238795325112867385, 1.000000000000000000, 0.9238795325112867385, 1.000000000000000000, 0.9238795325112867385, 1.000000000000000000, 0.9238795325112867385, 1.000000000000000000, 0.9238795325112867385, 1.000000000000000000, 0.9238795325112867385, 1.000000000000000000, 0.9238795325112867385, 1.000000000000000000, 0.9238795325112867385, 1.000000000000000000, 0.9238795325112867385, 1.000000000000000000, 0.9238795325112867385, 1.000000000000000000, 0.9238795325112867385, 1.000000000000000000, 0.9238795325112867385, 1.000000000000000000, 0.9238795325112867385, 1.000000000000000000, 0.9238795325112867385, 1.000000000000000000, 0.9238795325112867385, 1.000000000000000000, 0.9238795325112867385, 1.000000000000000000, 0.9238795325112867385, 1.000000000000000000, 0.9238795325112867385, 1.000000000000000000, 0.9238795325112867385, 1.000000000000000000, 0.9238795325112867385, 1.000000000000000000, 0.9238795325112867385, 1.000000000000000000, 0.9238795325112867385, 1.000000000000000000, 0.9238795325112867385, 1.000000000000000000, 0.9238795325112867385, 1.000000000000000000, 0.9238795325112867385, 1.000000000000000000, 0.9238795325112867385, 1.000000000000000000, 0.9238795325112867385, 1.000000000000000000, 0.9238795325112867385, 1.000000000000000000, 0.9238795325112867385, 1.000000000000000000, 0.9238795325112867385, 1.000000000000000000, 0.9238795325112867385, 1.000000000000000000, 0.9238795325112867385, 1.000000000000000000, 0.9238795325112867385, 1.000000000000000000, 0.9238795325112867385, 1.000000000000000000, 0.9238795325112867385, 1.000000000000000000, 0.9238795325112867385, 1.000000000000000000, 0.9238795325112867385, 1.000000000000000000, 0.9238795325112867385, 1.000000000000000000, 0.9238795325112867385, 1.000000000000000000, 0.9238795325112867385, 1.000000000000000000, 0.9238795325112867385, 1.000000000000000000, 0.9238795325112867385, 1.000000000000000000, 0.9238795325112867385, 1.000000000000000000, 0.9238795325112867385, 1.000000000000000000, 0.9238795325112867385, 1.000000000000000000, 0.9238795325112867385, 1.000000000000000000, 0.9238795325112867385, 1.000000000000000000, 0.9238795325112867385, 1.000000000000000000, 0.9238795325112867385, 1.000000000000000000, 0.9238795325112867385, 1.000000000000000000, 0.9238795325112867385, 1.000000000000000000, 0.9238795325112867385, 1.000000000000000000, 0.9238795325112867385, 1.000000000000000000, 0.9238795325112867385, 1.000000000000000000, 0.9238795325112867385, 1.000000000000000000, 0.9238795325112867385, 1.000000000000000000, 0.9238795325112867385, 1.000000000000000000, 0.9238795325112867385, 1.000000000000000000, 0.9238795325112867385, 1.000000000000000000, 0.9238795325112867385, 1.000000000000000000, 0.9238795325112867385, 1.000000000000000000, 0.9238795325112867385, 1.000000000000000000, 0.9238795325112867385, 1.000000000000000000, 0.9238795325112867385, 1.000000000000000000, 0.9238795325112867385, 1.000000000000000000, 0.9238795325112867385, 1.000000000000000000, 0.9238795325112867385, 1.000000000000000000, 0.9238795325112867385, 1.000000000000000000, 0.9238795325112867385, 1.000000000000000000, 0.9238795325112867385, 1.000000000000000000, 0.9238795325112867385, 1.000000000000000000, 0.9238795325112867385, 1.000000000000000000, 0.9238795325112867385, 1.000000000000000000, 0.9238795325112867385, 1.000000000000000000, 0.9238795325112867385, 1.000000000000000000, 0.9238795325112867385, 1.000000000000000000, 0.9238795325112867385, 1.000000000000000000, 0.9238795325112867385, 1.000000000000000000, 0.9238795325112867385, 1.000000000000000000, 0.9238795325112867385, 1.000000000000000000, 0.9238795325112867385, 1.000000000000000000, 0.9238795325112867385, 1.000000000000000000, 0.9238795325112867385, 1.000000000000000000, 0.9238795325112867385, 1.000000000000000000, 0.9238795325112867385, 1.000000000000000000, 0.9238795325112867385, 1.000000000000000000, 0.9238795325112867385, 1.000000000000000000, 0.9462258211652395667, 0.9684275895297407288) ) ) 
 REPRESENTATION_ITEM ( '' )  SURFACE ( )  );
#10280 = AXIS2_PLACEMENT_3D ( 'NONE', #15567, #4756, #13416 ) ;
#10281 = CARTESIAN_POINT ( 'NONE',  ( 97.93301270000000613, 123.7500000010924879, -9.540979117872439019E-15 ) ) ;
#10282 = CARTESIAN_POINT ( 'NONE',  ( 104.4587341249999923, 93.49999999863440792, 1.846868145590726318 ) ) ;
#10283 = CARTESIAN_POINT ( 'NONE',  ( 99.99999999999995737, -4.999999999999990230, 3.375000002731184612 ) ) ;
#10284 = CARTESIAN_POINT ( 'NONE',  ( 97.50236033167490746, 117.6869444889999841, -54.27499999726882862 ) ) ;
#10285 = EDGE_CURVE ( 'NONE', #3669, #1494, #17193, .T. ) ;
#10286 = CARTESIAN_POINT ( 'NONE',  ( 116.4251840539369596, 39.51171875216787299, 0.000000000000000000 ) ) ;
#10287 = VECTOR ( 'NONE', #3176, 1000.000000000000000 ) ;
#10288 = ORIENTED_EDGE ( 'NONE', *, *, #1313, .T. ) ;
#10289 = CARTESIAN_POINT ( 'NONE',  ( 78.14518615778180788, 38.02343750108395426, -5.444914386472297529 ) ) ;
#10290 = CARTESIAN_POINT ( 'NONE',  ( 94.99999999999995737, 83.12500000273119838, -1.387778780781445676E-14 ) ) ;
#10291 = CARTESIAN_POINT ( 'NONE',  ( 204.2950502721270425, 32.51679687608393721, -9.295050272127046043 ) ) ;
#10292 = ORIENTED_EDGE ( 'NONE', *, *, #24047, .T. ) ;
#10293 = LINE ( 'NONE', #25427, #9788 ) ;
#10294 = FACE_BOUND ( 'NONE', #12628, .T. ) ;
#10295 = CARTESIAN_POINT ( 'NONE',  ( 139.5988444088204403, 36.83281250216787583, -9.598844408820458085 ) ) ;
#10296 = CARTESIAN_POINT ( 'NONE',  ( 116.4251840539369596, 33.95546875216787441, 0.000000000000000000 ) ) ;
#10297 = CIRCLE ( 'NONE', #23091, 12.50000000000001599 ) ;
#10298 = CARTESIAN_POINT ( 'NONE',  ( 78.14518615778179367, 40.40468750108393436, -5.444914386472297529 ) ) ;
#10299 = CARTESIAN_POINT ( 'NONE',  ( 185.7049497278729575, 38.46992187608393721, 9.295050272127047819 ) ) ;
#10300 = ORIENTED_EDGE ( 'NONE', *, *, #15897, .F. ) ;
#10301 = VERTEX_POINT ( 'NONE', #15043 ) ;
#10302 =( LENGTH_UNIT ( ) NAMED_UNIT ( * ) SI_UNIT ( .MILLI., .METRE. ) );
#10303 = CARTESIAN_POINT ( 'NONE',  ( 95.54126587499996504, 1.846868145590750077, 13.62500000136559386 ) ) ;
#10304 = CARTESIAN_POINT ( 'NONE',  ( -9.598844408820454532, 40.30546874999999574, 9.598844408820459861 ) ) ;
#10305 = CARTESIAN_POINT ( 'NONE',  ( 2.493653234604083739E-15, 31.77265625216787370, 13.57481594606304576 ) ) ;
#10306 = DIRECTION ( 'NONE',  ( -1.000000000000000000, 0.000000000000000000, 0.000000000000000000 ) ) ;
#10307 = CARTESIAN_POINT ( 'NONE',  ( -5.444914386472297529, 40.60312500108393863, -13.14518615778179722 ) ) ;
#10308 = CARTESIAN_POINT ( 'NONE',  ( 102.4999999999999858, 123.0000000000000000, -8.724596124144689908E-15 ) ) ;
#10309 = CARTESIAN_POINT ( 'NONE',  ( 12.32011696698886816, 36.00000000000001421, -5.704949255836485378 ) ) ;
#10310 = CARTESIAN_POINT ( 'NONE',  ( 104.9999999999999858, 93.87499999726881583, -6.938893903907228378E-15 ) ) ;
#10311 = CARTESIAN_POINT ( 'NONE',  ( 120.4011555911795455, 32.36796874999999574, 9.598844408820459861 ) ) ;
#10312 = ORIENTED_EDGE ( 'NONE', *, *, #27597, .T. ) ;
#10313 = CARTESIAN_POINT ( 'NONE',  ( 2.493653234604083739E-15, 39.61093749999999147, 13.57481594606304576 ) ) ;
#10314 = CARTESIAN_POINT ( 'NONE',  ( -9.295050272127044266, 39.85898437608393152, 9.295050272127047819 ) ) ;
#10315 = CIRCLE ( 'NONE', #17614, 13.57481594606304398 ) ;
#10316 = CARTESIAN_POINT ( 'NONE',  ( 104.9999999999999716, 1.449011120738813565E-14, 5.625000002731185056 ) ) ;
#10317 = CARTESIAN_POINT ( 'NONE',  ( 116.8548138422182205, 39.16445312608393436, 0.000000000000000000 ) ) ;
#10318 = EDGE_CURVE ( 'NONE', #22337, #9781, #8761, .T. ) ;
#10319 = CARTESIAN_POINT ( 'NONE',  ( 65.00000000000000000, 37.57695312608392868, 13.14518615778179544 ) ) ;
#10320 = CARTESIAN_POINT ( 'NONE',  ( 189.5550856135277229, 39.31328125108394289, 13.14518615778179722 ) ) ;
#10321 = EDGE_CURVE ( 'NONE', #25975, #8262, #2680, .T. ) ;
#10322 = FACE_BOUND ( 'NONE', #24881, .T. ) ;
#10323 = CARTESIAN_POINT ( 'NONE',  ( -9.295050272127046043, 35.69179687608393436, -9.295050272127046043 ) ) ;
#10324 = DIRECTION ( 'NONE',  ( -1.000000000000000000, 0.000000000000000000, 0.000000000000000000 ) ) ;
#10325 = CARTESIAN_POINT ( 'NONE',  ( 195.7050241099688606, 35.99999999999999289, 13.13343125082109175 ) ) ;
#10326 = FACE_OUTER_BOUND ( 'NONE', #21252, .T. ) ;
#10327 = CARTESIAN_POINT ( 'NONE',  ( 95.27063293749995410, 84.84375000068281736, -1.387778780781445676E-14 ) ) ;
#10328 = CARTESIAN_POINT ( 'NONE',  ( 13.14518615778179900, 37.03125000108393294, -5.444914386472297529 ) ) ;
#10329 = CARTESIAN_POINT ( 'NONE',  ( 143.3933367278051207, 36.00000000000001421, -2.034633736484514621 ) ) ;
#10330 = CARTESIAN_POINT ( 'NONE',  ( 98.96446609406727646, 123.2569999999781487, -2.499999999999997780 ) ) ;
#10331 = EDGE_CURVE ( 'NONE', #24831, #24171, #21771, .T. ) ;
#10332 = CARTESIAN_POINT ( 'NONE',  ( 99.99999999999998579, 122.9500000010924765, -2.066987299999998751 ) ) ;
#10333 = CARTESIAN_POINT ( 'NONE',  ( 99.99999999999998579, 123.3500000010924680, 2.066987299999980099 ) ) ;
#10334 = CARTESIAN_POINT ( 'NONE',  ( 116.4251840539369596, 40.25585937716787299, -5.622872871577872189 ) ) ;
#10335 = CARTESIAN_POINT ( 'NONE',  ( 104.4587341249999781, 1.846868145590750299, 13.00000000136559386 ) ) ;
#10336 = CARTESIAN_POINT ( 'NONE',  ( -8.312177448680279460E-16, 32.16953125216787157, -13.57481594606304576 ) ) ;
#10337 = VERTEX_POINT ( 'NONE', #15469 ) ;
#10338 = DIRECTION ( 'NONE',  ( 0.000000000000000000, 0.000000000000000000, 1.000000000000000000 ) ) ;
#10339 = AXIS2_PLACEMENT_3D ( 'NONE', #12875, #6622, #26015 ) ;
#10340 = CARTESIAN_POINT ( 'NONE',  ( -13.14518615778179544, 32.02070312608393010, 0.000000000000000000 ) ) ;
#10341 = AXIS2_PLACEMENT_3D ( 'NONE', #4063, #4339, #23726 ) ;
#10342 = CARTESIAN_POINT ( 'NONE',  ( 5.444914386472302859, 32.86406250108392868, 13.14518615778179189 ) ) ;
#10343 = CARTESIAN_POINT ( 'NONE',  ( 5.622872871577871301, 32.91367187716787157, -13.57481594606304753 ) ) ;
#10344 = CARTESIAN_POINT ( 'NONE',  ( 185.4011555911795313, 36.23750000216787726, -9.598844408820458085 ) ) ;
#10345 = CARTESIAN_POINT ( 'NONE',  ( 104.4587341249999781, 84.12500000136560629, 1.846868145590721655 ) ) ;
#10346 = CARTESIAN_POINT ( 'NONE',  ( 70.44491438647230552, 38.91640625108393436, -13.14518615778179900 ) ) ;
#10347 = CARTESIAN_POINT ( 'NONE',  ( 102.4976396683250925, 102.3130555110000159, -46.77500000273119696 ) ) ;
#10348 = CARTESIAN_POINT ( 'NONE',  ( -9.295050272127046043, 40.45429687608393721, -9.295050272127046043 ) ) ;
#10349 = CARTESIAN_POINT ( 'NONE',  ( 99.14382582708707048, 124.1000000010924964, 2.066987299999979211 ) ) ;
#10350 = CARTESIAN_POINT ( 'NONE',  ( 65.00000000000000000, 38.51953125216787299, -13.57481594606304576 ) ) ;
#10351 = CARTESIAN_POINT ( 'NONE',  ( 105.6631189606246153, 114.1144967660473242, -49.29999999453763593 ) ) ;
#10352 = CARTESIAN_POINT ( 'NONE',  ( 133.7556381558600265, 31.78804748261757140, -13.14518615778179367 ) ) ;
#10353 = EDGE_LOOP ( 'NONE', ( #24402, #16652, #16829, #15544 ) ) ;
#10354 = CARTESIAN_POINT ( 'NONE',  ( -20.00000000000000000, 55.00000000000000000, 10.00000000000000178 ) ) ;
#10355 = CARTESIAN_POINT ( 'NONE',  ( 5.444914386472302859, 39.41250000108393436, 13.14518615778179189 ) ) ;
#10356 = CARTESIAN_POINT ( 'NONE',  ( 104.4587341249999639, 79.93750000136559208, -1.442382525525748735E-14 ) ) ;
#10357 = CARTESIAN_POINT ( 'NONE',  ( 124.5550856135277087, 40.40468750108393436, -13.14518615778179900 ) ) ;
#10358 = EDGE_CURVE ( 'NONE', #24596, #21433, #17670, .T. ) ;
#10359 = CARTESIAN_POINT ( 'NONE',  ( 59.37712712842213136, 36.48554687716787015, 13.57481594606304753 ) ) ;
#10360 = CARTESIAN_POINT ( 'NONE',  ( 91.91746824999997045, 107.3738262389971538, -55.52499999726882862 ) ) ;
#10361 = CARTESIAN_POINT ( 'NONE',  ( -13.57481594606304576, 34.74921875216787726, 0.000000000000000000 ) ) ;
#10362 = ORIENTED_EDGE ( 'NONE', *, *, #22515, .F. ) ;
#10363 = ADVANCED_FACE ( 'NONE', ( #8927 ), #17616, .T. ) ;
#10364 = AXIS2_PLACEMENT_3D ( 'NONE', #17044, #14897, #15463 ) ;
#10365 = CARTESIAN_POINT ( 'NONE',  ( 102.0710678118654329, 5.000000000000018652, 3.687499999999999556 ) ) ;
#10366 = EDGE_LOOP ( 'NONE', ( #24879, #17415, #7465, #2784 ) ) ;
#10367 = AXIS2_PLACEMENT_3D ( 'NONE', #9557, #18109, #26279 ) ;
#10368 = CARTESIAN_POINT ( 'NONE',  ( 181.8548138422181921, 37.32890625108393579, -5.444914386472297529 ) ) ;
#10369 =( BOUNDED_CURVE ( )  B_SPLINE_CURVE ( 2, ( #11050, #15759, #15328, #21628, #17767, #11330, #19906, #4519, #11187, #17475, #8787 ),
 .UNSPECIFIED., .F., .F. ) 
 B_SPLINE_CURVE_WITH_KNOTS ( ( 3, 2, 2, 2, 2, 3 ),
 ( 0.4000000000000003553, 0.4200000000000002065, 0.4400000000000000577, 0.4599999999999999645, 0.4799999999999997602, 0.4999999999999996669 ),
 .UNSPECIFIED. ) 
 CURVE ( )  GEOMETRIC_REPRESENTATION_ITEM ( )  RATIONAL_B_SPLINE_CURVE ( ( 0.9999999999999992228, 0.9510565162951543083, 1.000000000000000000, 0.9510565162951535312, 1.000000000000000000, 0.9510565162951535312, 1.000000000000000000, 0.9510565162951535312, 1.000000000000000000, 0.9510565162951543083, 0.9999999999999992228 ) ) 
 REPRESENTATION_ITEM ( '' )  );
#10370 = CARTESIAN_POINT ( 'NONE',  ( 3.878384841496545388, 31.34156311272377238, -13.57481594606304753 ) ) ;
#10371 = ADVANCED_FACE ( 'NONE', ( #22762 ), #26899, .T. ) ;
#10372 = CARTESIAN_POINT ( 'NONE',  ( 116.8548138422182205, 36.58476562608393579, 0.000000000000000000 ) ) ;
#10373 = CARTESIAN_POINT ( 'NONE',  ( 97.50000000000000000, 122.7500000021849615, 1.035533905932725096 ) ) ;
#10374 = CARTESIAN_POINT ( 'NONE',  ( 135.6228728715778686, 37.57695312499999574, -13.57481594606304753 ) ) ;
#10375 = CARTESIAN_POINT ( 'NONE',  ( 95.54126587500000767, 94.81249999863440792, -7.484931351350258973E-15 ) ) ;
#10376 = CARTESIAN_POINT ( 'NONE',  ( 65.00000000000000000, 38.51953125216787299, -13.57481594606304576 ) ) ;
#10377 = CARTESIAN_POINT ( 'NONE',  ( -13.14518615778179900, 38.91640625108393436, -5.444914386472297529 ) ) ;
#10378 = CARTESIAN_POINT ( 'NONE',  ( 181.4251840539369596, 38.66835937499999432, 5.622872871577880183 ) ) ;
#10379 = ITEM_DEFINED_TRANSFORMATION ( 'NONE', 'NONE', #9486,  #26844 ) ;
#10380 = CARTESIAN_POINT ( 'NONE',  ( 94.99999999999995737, 1.387778780781445676E-14, 8.125000002731185944 ) ) ;
#10381 = CARTESIAN_POINT ( 'NONE',  ( 95.54126587499996504, 1.387778780781445676E-14, 2.687500001365592528 ) ) ;
#10382 = CARTESIAN_POINT ( 'NONE',  ( 70.44491438647230552, 39.51171875108392584, -13.14518615778179900 ) ) ;
#10383 = CARTESIAN_POINT ( 'NONE',  ( 98.15313185440923860, -4.458734124999987891, 4.625000001365592084 ) ) ;
#10384 = CARTESIAN_POINT ( 'NONE',  ( 139.1801758136479918, 55.00000000000000000, 9.999999999999964473 ) ) ;
#10385 = CARTESIAN_POINT ( 'NONE',  ( 98.15313185440925281, 90.62499999863439371, -4.458734124999994997 ) ) ;
#10386 = DIRECTION ( 'NONE',  ( 0.000000000000000000, 0.000000000000000000, -1.000000000000000000 ) ) ;
#10387 = CARTESIAN_POINT ( 'NONE',  ( -13.57481594606304576, 38.61874999999999147, 0.000000000000000000 ) ) ;
#10388 = CARTESIAN_POINT ( 'NONE',  ( 116.8548138422182205, 39.95820312608393010, 0.000000000000000000 ) ) ;
#10389 = AXIS2_PLACEMENT_3D ( 'NONE', #9872, #22721, #11858 ) ;
#10390 = VECTOR ( 'NONE', #15875, 1000.000000000000000 ) ;
#10391 = ORIENTED_EDGE ( 'NONE', *, *, #446, .F. ) ;
#10392 = CARTESIAN_POINT ( 'NONE',  ( 103.1528011352953342, 81.06250000136559208, 3.152801135295355106 ) ) ;
#10393 = VECTOR ( 'NONE', #24442, 1000.000000000000000 ) ;
#10394 = CARTESIAN_POINT ( 'NONE',  ( 99.99999999999998579, 91.56249999863440792, -4.458734124999994997 ) ) ;
#10395 = VERTEX_POINT ( 'NONE', #20190 ) ;
#10396 = CARTESIAN_POINT ( 'NONE',  ( 105.6631189606246295, 105.8855032339526758, -46.20000000000000995 ) ) ;
#10397 = CARTESIAN_POINT ( 'NONE',  ( 78.14518615778179367, 35.64218750108393152, -5.444914386472297529 ) ) ;
#10398 =( REPRESENTATION_RELATIONSHIP ('NONE','NONE', #2411, #19878 ) REPRESENTATION_RELATIONSHIP_WITH_TRANSFORMATION ( #16811 )SHAPE_REPRESENTATION_RELATIONSHIP( ) );
#10399 = VERTEX_POINT ( 'NONE', #27186 ) ;
#10400 = CARTESIAN_POINT ( 'NONE',  ( 124.6826484225240961, 54.47013368152369850, -15.00000000000000000 ) ) ;
#10401 = ADVANCED_FACE ( 'NONE', ( #18189 ), #18762, .T. ) ;
#10402 = CARTESIAN_POINT ( 'NONE',  ( 103.1528011352953342, 3.152801135295383084, 5.312500001365592972 ) ) ;
#10403 = VERTEX_POINT ( 'NONE', #25160 ) ;
#10404 = DIRECTION ( 'NONE',  ( 1.000000000000000000, 0.000000000000000000, -2.385244779468110248E-16 ) ) ;
#10405 = CARTESIAN_POINT ( 'NONE',  ( -5.444914386472297529, 33.26093750108393721, -13.14518615778179900 ) ) ;
#10406 = CARTESIAN_POINT ( 'NONE',  ( 181.4251840539369596, 38.71796875216787726, 0.000000000000000000 ) ) ;
#10407 = CARTESIAN_POINT ( 'NONE',  ( 9.295050272127046043, 40.25585937608393294, -9.295050272127046043 ) ) ;
#10408 = CARTESIAN_POINT ( 'NONE',  ( 77.07727640983618755, 35.99999999999999289, -6.197985357348142266 ) ) ;
#10409 = CARTESIAN_POINT ( 'NONE',  ( 201.1198436276839629, 51.28708186915499567, 14.99999999999995204 ) ) ;
#10410 = CARTESIAN_POINT ( 'NONE',  ( -13.09590655363597733, 35.99999999999999289, 1.137167824541468031 ) ) ;
#10411 = CARTESIAN_POINT ( 'NONE',  ( 9.295050272127047819, 38.66835937608393436, 9.295050272127046043 ) ) ;
#10412 = EDGE_LOOP ( 'NONE', ( #26229, #15584, #11241, #14538 ) ) ;
#10413 = COLOUR_RGB ( '', 0.09019608, 0.27058824, 0.51372549) ;
#10414 = CARTESIAN_POINT ( 'NONE',  ( 65.00000000000000000, 38.02343749999999289, 13.57481594606304576 ) ) ;
#10415 = LINE ( 'NONE', #3879, #5499 ) ;
#10416 = CARTESIAN_POINT ( 'NONE',  ( 130.0000000000000000, 40.10703125216787157, -13.57481594606304576 ) ) ;
#10417 =( BOUNDED_SURFACE ( )  B_SPLINE_SURFACE ( 1, 2, ( 
 ( #12396, #3315, #18567, #1049, #7998, #18423, #18834, #5740, #23124, #10121, #3599, #27541, #9721, #12257, #21117, #7582, #1604, #11986, #20710, #27269, #7725, #23396, #19252, #23811, #17247, #6146, #23952, #13086, #27954, #19532, #4434, #3869, #10406, #27678, #21404, #12531, #21681, #17100, #8411, #8698, #21259, #21826, #4288, #4012, #27820, #12946, #2301, #25803, #25664, #10961, #19388, #8141, #2156, #17389, #16835, #6011, #10817, #12813, #2012, #6280, #23676, #25531, #14, #26088, #28093, #6554, #14675, #6422, #15234, #1740, #19112, #12678, #25947, #8273, #16964, #14811, #14957, #23536, #15091, #1882, #10545, #4153, #21536, #10681, #8556, #15379, #2441, #19672, #13375, #4569, #13669, #9124, #11243, #728, #13230, #5140, #15814, #24234, #19815, #5006, #22529, #17817, #17672, #2996, #11385, #156, #24519, #9400, #8840, #26232, #22383, #4860, #22246, #19961, #15673, #15950, #20243, #2857, #13526, #17531, #6690, #18099, #21962, #26812, #9263, #24094, #17957, #11102, #8983, #298, #11524, #7260, #26521, #6977, #6836, #26380, #15527, #4716, #22105, #24665, #13806, #438, #2583, #24372, #2724, #20107, #585, #26668, #7114, #16385, #7694, #5428, #1161, #18804, #1432, #14097, #18250, #18533, #10091, #25084, #22958, #20390, #23090, #27096, #23229, #877, #9826, #5572, #9691, #11815, #3564, #27510, #22816, #7966, #11669, #9548, #18673, #7549, #16667, #14236, #12223, #20537, #25363 ),
 ( #27238, #3284, #18390, #20811, #3420, #5843, #12088, #16245, #14512, #1020, #27374, #20951, #26958, #5284, #7401, #1291, #16094, #24942, #24802, #13948, #9960, #22675, #3148, #11955, #7833, #20678, #16527, #25219, #5709, #14375, #8663, #10784, #19497, #25631, #8107, #19354, #23364, #19216, #17210, #2117, #25915, #10511, #12782, #25498, #17065, #19077, #6387, #28057, #15058, #23775, #4252, #5978, #21368, #27920, #12911, #25769, #1848, #21643, #1709, #1574, #8380, #6248, #21498, #28195, #14779, #10368, #6520, #23641, #15197, #8523, #17354, #3706, #10227, #26050, #14920, #4116, #23500, #1979, #12367, #21086, #18937, #10648, #27646, #16801, #14645, #3836, #12497, #21224, #27782, #8240, #16930, #6113, #3979, #12642, #9228, #13340, #22069, #11065, #7219, #6655, #15341, #26342, #7079, #11488, #24199, #19635, #9365, #4968, #691, #258, #6941, #4532, #405, #19921, #17631, #2545, #2820, #13629, #6799, #2266, #11206, #22349, #9087, #15637, #4394, #15775, #19775, #23914, #13050, #17783, #117, #15485, #21787, #10926, #24057, #4678, #8801, #26486, #26774, #17492, #13194, #20204, #26190, #21929, #547, #18059, #24338, #2405, #4824, #8943, #13484, #22206, #2686, #11346, #20069, #17921, #26632, #24481, #13910, #1258, #11629, #5246, #9648, #24765, #3529, #11774, #5104, #20353, #27059, #10057, #20774, #16202, #9918, #5389, #22638, #25048, #22779, #20914, #11915, #20498, #12185, #3106, #3378 ) ),
 .UNSPECIFIED., .F., .F., .T. ) 
 B_SPLINE_SURFACE_WITH_KNOTS ( ( 2, 2 ),
 ( 3, 2, 2, 2, 2, 2, 2, 2, 2, 2, 2, 2, 2, 2, 2, 2, 2, 2, 2, 2, 2, 2, 2, 2, 2, 2, 2, 2, 2, 2, 2, 2, 2, 2, 2, 2, 2, 2, 2, 2, 2, 2, 2, 2, 2, 2, 2, 2, 2, 2, 2, 2, 2, 2, 2, 2, 2, 2, 2, 2, 2, 2, 2, 2, 2, 2, 2, 2, 2, 2, 2, 2, 2, 2, 2, 2, 2, 2, 2, 2, 2, 2, 2, 2, 2, 2, 2, 2, 2, 2, 2, 3 ),
 ( 0.000000000000000000, 1.000000000000000000 ),
 ( 0.000000000000000000, 0.01041666666666666609, 0.02083333333333333218, 0.03125000000000000000, 0.04166666666666666435, 0.05208333333333333565, 0.06250000000000000000, 0.07291666666666667129, 0.08333333333333332871, 0.09375000000000000000, 0.1041666666666666713, 0.1145833333333333287, 0.1250000000000000000, 0.1354166666666666574, 0.1458333333333333426, 0.1562500000000000000, 0.1666666666666666574, 0.1770833333333333426, 0.1875000000000000000, 0.1979166666666666574, 0.2083333333333333426, 0.2187500000000000000, 0.2291666666666666574, 0.2395833333333333426, 0.2500000000000000000, 0.2604166666666666852, 0.2708333333333333148, 0.2812500000000000000, 0.2916666666666666852, 0.3020833333333333148, 0.3125000000000000000, 0.3229166666666666852, 0.3333333333333333148, 0.3437500000000000000, 0.3541666666666666852, 0.3645833333333333148, 0.3750000000000000000, 0.3854166666666666852, 0.3958333333333333148, 0.4062500000000000000, 0.4166666666666666852, 0.4270833333333333148, 0.4375000000000000000, 0.4479166666666666852, 0.4583333333333333148, 0.4687500000000000000, 0.4791666666666666852, 0.4895833333333333148, 0.5000000000000000000, 0.5104166666666666297, 0.5208333333333333703, 0.5312500000000000000, 0.5416666666666666297, 0.5520833333333333703, 0.5625000000000000000, 0.5729166666666666297, 0.5833333333333333703, 0.5937500000000000000, 0.6041666666666666297, 0.6145833333333333703, 0.6250000000000000000, 0.6354166666666666297, 0.6458333333333333703, 0.6562500000000000000, 0.6666666666666666297, 0.6770833333333333703, 0.6875000000000000000, 0.6979166666666666297, 0.7083333333333333703, 0.7187500000000000000, 0.7291666666666666297, 0.7395833333333333703, 0.7500000000000000000, 0.7604166666666666297, 0.7708333333333333703, 0.7812500000000000000, 0.7916666666666666297, 0.8020833333333333703, 0.8125000000000000000, 0.8229166666666666297, 0.8333333333333333703, 0.8437500000000000000, 0.8541666666666666297, 0.8645833333333333703, 0.8750000000000000000, 0.8854166666666666297, 0.8958333333333333703, 0.9062500000000000000, 0.9166666666666666297, 0.9270833333333333703, 0.9375000000000000000, 0.9448586970929392370 ),
 .UNSPECIFIED. ) 
 GEOMETRIC_REPRESENTATION_ITEM ( )  RATIONAL_B_SPLINE_SURFACE ( (
 ( 1.000000000000000000, 0.9238795325112867385, 1.000000000000000000, 0.9238795325112867385, 1.000000000000000000, 0.9238795325112867385, 1.000000000000000000, 0.9238795325112867385, 1.000000000000000000, 0.9238795325112867385, 1.000000000000000000, 0.9238795325112867385, 1.000000000000000000, 0.9238795325112867385, 1.000000000000000000, 0.9238795325112867385, 1.000000000000000000, 0.9238795325112867385, 1.000000000000000000, 0.9238795325112867385, 1.000000000000000000, 0.9238795325112867385, 1.000000000000000000, 0.9238795325112867385, 1.000000000000000000, 0.9238795325112867385, 1.000000000000000000, 0.9238795325112867385, 1.000000000000000000, 0.9238795325112867385, 1.000000000000000000, 0.9238795325112867385, 1.000000000000000000, 0.9238795325112867385, 1.000000000000000000, 0.9238795325112867385, 1.000000000000000000, 0.9238795325112867385, 1.000000000000000000, 0.9238795325112867385, 1.000000000000000000, 0.9238795325112867385, 1.000000000000000000, 0.9238795325112867385, 1.000000000000000000, 0.9238795325112867385, 1.000000000000000000, 0.9238795325112867385, 1.000000000000000000, 0.9238795325112867385, 1.000000000000000000, 0.9238795325112867385, 1.000000000000000000, 0.9238795325112867385, 1.000000000000000000, 0.9238795325112867385, 1.000000000000000000, 0.9238795325112867385, 1.000000000000000000, 0.9238795325112867385, 1.000000000000000000, 0.9238795325112867385, 1.000000000000000000, 0.9238795325112867385, 1.000000000000000000, 0.9238795325112867385, 1.000000000000000000, 0.9238795325112867385, 1.000000000000000000, 0.9238795325112867385, 1.000000000000000000, 0.9238795325112867385, 1.000000000000000000, 0.9238795325112867385, 1.000000000000000000, 0.9238795325112867385, 1.000000000000000000, 0.9238795325112867385, 1.000000000000000000, 0.9238795325112867385, 1.000000000000000000, 0.9238795325112867385, 1.000000000000000000, 0.9238795325112867385, 1.000000000000000000, 0.9238795325112867385, 1.000000000000000000, 0.9238795325112867385, 1.000000000000000000, 0.9238795325112867385, 1.000000000000000000, 0.9238795325112867385, 1.000000000000000000, 0.9238795325112867385, 1.000000000000000000, 0.9238795325112867385, 1.000000000000000000, 0.9238795325112867385, 1.000000000000000000, 0.9238795325112867385, 1.000000000000000000, 0.9238795325112867385, 1.000000000000000000, 0.9238795325112867385, 1.000000000000000000, 0.9238795325112867385, 1.000000000000000000, 0.9238795325112867385, 1.000000000000000000, 0.9238795325112867385, 1.000000000000000000, 0.9238795325112867385, 1.000000000000000000, 0.9238795325112867385, 1.000000000000000000, 0.9238795325112867385, 1.000000000000000000, 0.9238795325112867385, 1.000000000000000000, 0.9238795325112867385, 1.000000000000000000, 0.9238795325112867385, 1.000000000000000000, 0.9238795325112867385, 1.000000000000000000, 0.9238795325112867385, 1.000000000000000000, 0.9238795325112867385, 1.000000000000000000, 0.9238795325112867385, 1.000000000000000000, 0.9238795325112867385, 1.000000000000000000, 0.9238795325112867385, 1.000000000000000000, 0.9238795325112867385, 1.000000000000000000, 0.9238795325112867385, 1.000000000000000000, 0.9238795325112867385, 1.000000000000000000, 0.9238795325112867385, 1.000000000000000000, 0.9238795325112867385, 1.000000000000000000, 0.9238795325112867385, 1.000000000000000000, 0.9238795325112867385, 1.000000000000000000, 0.9238795325112867385, 1.000000000000000000, 0.9238795325112867385, 1.000000000000000000, 0.9238795325112867385, 1.000000000000000000, 0.9238795325112867385, 1.000000000000000000, 0.9238795325112867385, 1.000000000000000000, 0.9238795325112867385, 1.000000000000000000, 0.9238795325112867385, 1.000000000000000000, 0.9238795325112867385, 1.000000000000000000, 0.9238795325112867385, 1.000000000000000000, 0.9238795325112867385, 1.000000000000000000, 0.9238795325112867385, 1.000000000000000000, 0.9238795325112867385, 1.000000000000000000, 0.9238795325112867385, 1.000000000000000000, 0.9238795325112867385, 1.000000000000000000, 0.9238795325112867385, 1.000000000000000000, 0.9238795325112867385, 1.000000000000000000, 0.9462258435690522607, 0.9684275710300105366),
 ( 1.000000000000000000, 0.9238795325112867385, 1.000000000000000000, 0.9238795325112867385, 1.000000000000000000, 0.9238795325112867385, 1.000000000000000000, 0.9238795325112867385, 1.000000000000000000, 0.9238795325112867385, 1.000000000000000000, 0.9238795325112867385, 1.000000000000000000, 0.9238795325112867385, 1.000000000000000000, 0.9238795325112867385, 1.000000000000000000, 0.9238795325112867385, 1.000000000000000000, 0.9238795325112867385, 1.000000000000000000, 0.9238795325112867385, 1.000000000000000000, 0.9238795325112867385, 1.000000000000000000, 0.9238795325112867385, 1.000000000000000000, 0.9238795325112867385, 1.000000000000000000, 0.9238795325112867385, 1.000000000000000000, 0.9238795325112867385, 1.000000000000000000, 0.9238795325112867385, 1.000000000000000000, 0.9238795325112867385, 1.000000000000000000, 0.9238795325112867385, 1.000000000000000000, 0.9238795325112867385, 1.000000000000000000, 0.9238795325112867385, 1.000000000000000000, 0.9238795325112867385, 1.000000000000000000, 0.9238795325112867385, 1.000000000000000000, 0.9238795325112867385, 1.000000000000000000, 0.9238795325112867385, 1.000000000000000000, 0.9238795325112867385, 1.000000000000000000, 0.9238795325112867385, 1.000000000000000000, 0.9238795325112867385, 1.000000000000000000, 0.9238795325112867385, 1.000000000000000000, 0.9238795325112867385, 1.000000000000000000, 0.9238795325112867385, 1.000000000000000000, 0.9238795325112867385, 1.000000000000000000, 0.9238795325112867385, 1.000000000000000000, 0.9238795325112867385, 1.000000000000000000, 0.9238795325112867385, 1.000000000000000000, 0.9238795325112867385, 1.000000000000000000, 0.9238795325112867385, 1.000000000000000000, 0.9238795325112867385, 1.000000000000000000, 0.9238795325112867385, 1.000000000000000000, 0.9238795325112867385, 1.000000000000000000, 0.9238795325112867385, 1.000000000000000000, 0.9238795325112867385, 1.000000000000000000, 0.9238795325112867385, 1.000000000000000000, 0.9238795325112867385, 1.000000000000000000, 0.9238795325112867385, 1.000000000000000000, 0.9238795325112867385, 1.000000000000000000, 0.9238795325112867385, 1.000000000000000000, 0.9238795325112867385, 1.000000000000000000, 0.9238795325112867385, 1.000000000000000000, 0.9238795325112867385, 1.000000000000000000, 0.9238795325112867385, 1.000000000000000000, 0.9238795325112867385, 1.000000000000000000, 0.9238795325112867385, 1.000000000000000000, 0.9238795325112867385, 1.000000000000000000, 0.9238795325112867385, 1.000000000000000000, 0.9238795325112867385, 1.000000000000000000, 0.9238795325112867385, 1.000000000000000000, 0.9238795325112867385, 1.000000000000000000, 0.9238795325112867385, 1.000000000000000000, 0.9238795325112867385, 1.000000000000000000, 0.9238795325112867385, 1.000000000000000000, 0.9238795325112867385, 1.000000000000000000, 0.9238795325112867385, 1.000000000000000000, 0.9238795325112867385, 1.000000000000000000, 0.9238795325112867385, 1.000000000000000000, 0.9238795325112867385, 1.000000000000000000, 0.9238795325112867385, 1.000000000000000000, 0.9238795325112867385, 1.000000000000000000, 0.9238795325112867385, 1.000000000000000000, 0.9238795325112867385, 1.000000000000000000, 0.9238795325112867385, 1.000000000000000000, 0.9238795325112867385, 1.000000000000000000, 0.9238795325112867385, 1.000000000000000000, 0.9238795325112867385, 1.000000000000000000, 0.9238795325112867385, 1.000000000000000000, 0.9238795325112867385, 1.000000000000000000, 0.9238795325112867385, 1.000000000000000000, 0.9238795325112867385, 1.000000000000000000, 0.9238795325112867385, 1.000000000000000000, 0.9238795325112867385, 1.000000000000000000, 0.9238795325112867385, 1.000000000000000000, 0.9238795325112867385, 1.000000000000000000, 0.9238795325112867385, 1.000000000000000000, 0.9238795325112867385, 1.000000000000000000, 0.9238795325112867385, 1.000000000000000000, 0.9238795325112867385, 1.000000000000000000, 0.9238795325112867385, 1.000000000000000000, 0.9238795325112867385, 1.000000000000000000, 0.9238795325112867385, 1.000000000000000000, 0.9238795325112867385, 1.000000000000000000, 0.9462258435690522607, 0.9684275710300105366) ) ) 
 REPRESENTATION_ITEM ( '' )  SURFACE ( )  );
#10418 = CARTESIAN_POINT ( 'NONE',  ( 98.15313185440925281, 4.458734125000016313, 5.250000001365592972 ) ) ;
#10419 = CARTESIAN_POINT ( 'NONE',  ( 9.295050272127047819, 32.31835937608393294, 9.295050272127046043 ) ) ;
#10420 = CARTESIAN_POINT ( 'NONE',  ( 103.1528011352953342, 3.152801135295383084, 4.312500001365592084 ) ) ;
#10421 = CARTESIAN_POINT ( 'NONE',  ( 98.15313185440923860, 81.87500000136560629, 4.458734124999987891 ) ) ;
#10422 = CARTESIAN_POINT ( 'NONE',  ( -8.049105076161786076E-16, 31.62382812608393579, -13.14518615778179544 ) ) ;
#10423 = CARTESIAN_POINT ( 'NONE',  ( 107.0000000000000142, 110.0000000000000000, -55.00000000000000711 ) ) ;
#10424 = ORIENTED_EDGE ( 'NONE', *, *, #14399, .T. ) ;
#10425 = CARTESIAN_POINT ( 'NONE',  ( 9.295050272127047819, 33.11210937608393579, 9.295050272127046043 ) ) ;
#10426 = CARTESIAN_POINT ( 'NONE',  ( 92.99999999999998579, 110.0000000000000000, -54.49999999453763877 ) ) ;
#10427 = DIRECTION ( 'NONE',  ( 1.000000000000000000, 0.000000000000000000, 0.000000000000000000 ) ) ;
#10428 = CARTESIAN_POINT ( 'NONE',  ( 102.0710678118654329, 83.43750000273121259, 4.999999999999989342 ) ) ;
#10429 = CARTESIAN_POINT ( 'NONE',  ( 108.0825317499999869, 112.6261737610028320, -52.77499999726883573 ) ) ;
#10430 = CARTESIAN_POINT ( 'NONE',  ( 102.0710678118654329, -4.999999999999989342, 6.437500002731185944 ) ) ;
#10431 =( GEOMETRIC_REPRESENTATION_CONTEXT ( 3 ) GLOBAL_UNCERTAINTY_ASSIGNED_CONTEXT ( ( #16613 ) ) GLOBAL_UNIT_ASSIGNED_CONTEXT ( ( #16598, #8460, #23855 ) ) REPRESENTATION_CONTEXT ( 'NONE', 'WORKASPACE' ) );
#10432 = VERTEX_POINT ( 'NONE', #3507 ) ;
#10433 = CARTESIAN_POINT ( 'NONE',  ( 51.85481384221820633, 38.32109375108394289, -5.444914386472297529 ) ) ;
#10434 = AXIS2_PLACEMENT_3D ( 'NONE', #18412, #5866, #10249 ) ;
#10435 = DIRECTION ( 'NONE',  ( 0.000000000000000000, 1.000000000000000000, 0.000000000000000000 ) ) ;
#10436 = DIRECTION ( 'NONE',  ( 0.000000000000000000, -0.000000000000000000, 1.000000000000000000 ) ) ;
#10437 = ORIENTED_EDGE ( 'NONE', *, *, #12599, .F. ) ;
#10438 = CARTESIAN_POINT ( 'NONE',  ( 97.92893218813455292, 92.68749999999998579, 5.000000000000011546 ) ) ;
#10439 = CARTESIAN_POINT ( 'NONE',  ( -6.412866676253197618, 50.00000000108475717, -11.99502265407683943 ) ) ;
#10440 = CARTESIAN_POINT ( 'NONE',  ( 99.99999999999995737, 80.87500000273119838, -5.000000000000018652 ) ) ;
#10441 = AXIS2_PLACEMENT_3D ( 'NONE', #21439, #6593, #10586 ) ;
#10442 = CARTESIAN_POINT ( 'NONE',  ( 116.4251840539369596, 34.00507812716787015, 5.622872871577880183 ) ) ;
#10443 = CARTESIAN_POINT ( 'NONE',  ( 59.55508561352770158, 39.80937500108392868, -13.14518615778179900 ) ) ;
#10444 = CYLINDRICAL_SURFACE ( 'NONE', #24625, 5.000000000000004441 ) ;
#10445 = CARTESIAN_POINT ( 'NONE',  ( 204.2950502721270425, 39.46210937608393721, 9.295050272127046043 ) ) ;
#10446 = ORIENTED_EDGE ( 'NONE', *, *, #15415, .F. ) ;
#10447 = EDGE_CURVE ( 'NONE', #4790, #4419, #18752, .T. ) ;
#10448 = ORIENTED_EDGE ( 'NONE', *, *, #4953, .F. ) ;
#10449 = CARTESIAN_POINT ( 'NONE',  ( -5.444914386472299306, 34.35234375108392868, 13.14518615778179722 ) ) ;
#10450 =( NAMED_UNIT ( * ) SI_UNIT ( $, .STERADIAN. ) SOLID_ANGLE_UNIT ( ) );
#10451 = CARTESIAN_POINT ( 'NONE',  ( 104.4587341249999639, 1.442382525525748735E-14, 14.18750000136559208 ) ) ;
#10452 = CARTESIAN_POINT ( 'NONE',  ( 5.622872871577742515, 39.66054687500000142, 13.57481594606318076 ) ) ;
#10453 = CARTESIAN_POINT ( 'NONE',  ( 103.1528011352953342, 84.06250000136560629, -3.152801135295383084 ) ) ;
#10454 = CARTESIAN_POINT ( 'NONE',  ( 102.0669872999999797, 122.5500000010924850, -9.794112055954760458E-15 ) ) ;
#10455 = VECTOR ( 'NONE', #1722, 1000.000000000000000 ) ;
#10456 = FACE_OUTER_BOUND ( 'NONE', #11088, .T. ) ;
#10457 = CARTESIAN_POINT ( 'NONE',  ( 94.99999999999995737, 1.387778780781445676E-14, 5.999999999999998224 ) ) ;
#10458 = DIRECTION ( 'NONE',  ( 1.000000000000000000, 0.000000000000000000, -3.469446951953613696E-16 ) ) ;
#10459 = LINE ( 'NONE', #21170, #7597 ) ;
#10460 = ORIENTED_EDGE ( 'NONE', *, *, #25852, .F. ) ;
#10461 = CARTESIAN_POINT ( 'NONE',  ( -13.57481594606304576, 40.20624999999999005, 0.000000000000000000 ) ) ;
#10462 = CARTESIAN_POINT ( 'NONE',  ( -5.622872871577873077, 32.21914062716787441, -13.57481594606304753 ) ) ;
#10463 = CARTESIAN_POINT ( 'NONE',  ( 102.0710678118654329, 5.000000000000018652, 1.812500002731185278 ) ) ;
#10464 = CARTESIAN_POINT ( 'NONE',  ( 124.5550856135277087, 37.72578125108395142, 13.14518615778179722 ) ) ;
#10465 = CARTESIAN_POINT ( 'NONE',  ( 74.29505027212704249, 37.87460937608393152, -9.295050272127046043 ) ) ;
#10466 = CARTESIAN_POINT ( 'NONE',  ( 189.5550856135277229, 39.01562500108394005, -13.14518615778179900 ) ) ;
#10467 = CARTESIAN_POINT ( 'NONE',  ( 51.94161814354912110, 36.00000000000000000, 1.569311539113921405 ) ) ;
#10468 = CARTESIAN_POINT ( 'NONE',  ( -8.049105076161786076E-16, 36.38632812608393152, -13.14518615778179544 ) ) ;
#10469 = CARTESIAN_POINT ( 'NONE',  ( 97.92893218813451028, -4.999999999999989342, 9.312500002731184168 ) ) ;
#10470 = LINE ( 'NONE', #4355, #23518 ) ;
#10471 = DIRECTION ( 'NONE',  ( -0.000000000000000000, -1.000000000000000000, -0.000000000000000000 ) ) ;
#10472 = AXIS2_PLACEMENT_3D ( 'NONE', #6844, #2731, #736 ) ;
#10473 = CARTESIAN_POINT ( 'NONE',  ( -5.444914386472297529, 38.81718750108393579, -13.14518615778179900 ) ) ;
#10474 = CARTESIAN_POINT ( 'NONE',  ( 7.616525325480809627, 54.91574374957784244, 14.99999999999999467 ) ) ;
#10475 = CARTESIAN_POINT ( 'NONE',  ( 102.4999999999999858, 122.9976688166997860, 0.1932551333443592867 ) ) ;
#10476 = CARTESIAN_POINT ( 'NONE',  ( 98.53841926354351699, 123.8500000010924680, -1.461580736456474794 ) ) ;
#10477 = CARTESIAN_POINT ( 'NONE',  ( 97.93301270000000613, 123.2000000010924765, 0.8561741729129328515 ) ) ;
#10478 =( NAMED_UNIT ( * ) SI_UNIT ( $, .STERADIAN. ) SOLID_ANGLE_UNIT ( ) );
#10479 = ORIENTED_EDGE ( 'NONE', *, *, #24799, .T. ) ;
#10480 = CARTESIAN_POINT ( 'NONE',  ( 104.4587341249999781, -1.846868145590721655, 10.87500000136559386 ) ) ;
#10481 = FACE_OUTER_BOUND ( 'NONE', #20978, .T. ) ;
#10482 = ORIENTED_EDGE ( 'NONE', *, *, #13111, .T. ) ;
#10483 = FACE_OUTER_BOUND ( 'NONE', #21156, .T. ) ;
#10484 = CARTESIAN_POINT ( 'NONE',  ( 13.57481594606304753, 39.85898437499999858, -5.622872871577873077 ) ) ;
#10485 = CARTESIAN_POINT ( 'NONE',  ( 103.5355339059327093, 3.535533905932755072, 8.624999999999998224 ) ) ;
#10486 = CARTESIAN_POINT ( 'NONE',  ( -13.57481594606304576, 33.16171875216787868, 0.000000000000000000 ) ) ;
#10487 = PLANE ( 'NONE',  #4021 ) ;
#10488 = CARTESIAN_POINT ( 'NONE',  ( 96.84719886470459471, 84.56250000136560629, -3.152801135295383084 ) ) ;
#10489 = CARTESIAN_POINT ( 'NONE',  ( 70.44491438647230552, 38.12265625108393152, -13.14518615778179900 ) ) ;
#10490 = EDGE_CURVE ( 'NONE', #27733, #23414, #24415, .T. ) ;
#10491 = CARTESIAN_POINT ( 'NONE',  ( 97.50236033167492167, 102.3130555110000159, -46.97500000273119269 ) ) ;
#10492 = CARTESIAN_POINT ( 'NONE',  ( 102.0710678118654329, 5.000000000000018652, 11.68750000000000000 ) ) ;
#10493 = ORIENTED_EDGE ( 'NONE', *, *, #9321, .T. ) ;
#10494 = CARTESIAN_POINT ( 'NONE',  ( 97.93301270000000613, 124.7500000010924737, -9.540979117872439019E-15 ) ) ;
#10495 = CARTESIAN_POINT ( 'NONE',  ( 55.40115559117954547, 38.81718750216787583, 9.598844408820459861 ) ) ;
#10496 = CARTESIAN_POINT ( 'NONE',  ( 95.67376207875069838, 115.9545556584642867, -52.79999999453764303 ) ) ;
#10497 = CARTESIAN_POINT ( 'NONE',  ( 116.8548138422182205, 32.81445312608393294, 0.000000000000000000 ) ) ;
#10498 = ORIENTED_EDGE ( 'NONE', *, *, #5538, .T. ) ;
#10499 = DIRECTION ( 'NONE',  ( 1.000000000000000000, -0.000000000000000000, -7.228014483236696740E-18 ) ) ;
#10500 = CARTESIAN_POINT ( 'NONE',  ( 13.14518615778179900, 39.51171875108392584, 5.444914386472293977 ) ) ;
#10501 = CARTESIAN_POINT ( 'NONE',  ( 5.622872871577878406, 39.75976562716787299, 13.57481594606304576 ) ) ;
#10502 = CARTESIAN_POINT ( 'NONE',  ( 130.0000000000000000, 39.56132812608393579, -13.14518615778179544 ) ) ;
#10503 = CARTESIAN_POINT ( 'NONE',  ( 59.37712712842213136, 35.69179687716786731, 13.57481594606304753 ) ) ;
#10504 = AXIS2_PLACEMENT_3D ( 'NONE', #12126, #25404, #14555 ) ;
#10505 = CARTESIAN_POINT ( 'NONE',  ( 99.99999999999997158, 118.4984768113314004, -50.12499999726881583 ) ) ;
#10506 = CARTESIAN_POINT ( 'NONE',  ( -13.57481594606304576, 34.79882812716787299, 5.622872871577880183 ) ) ;
#10507 = ORIENTED_EDGE ( 'NONE', *, *, #118, .T. ) ;
#10508 = CARTESIAN_POINT ( 'NONE',  ( 104.9999999999999574, 2.071067811865491937, 4.562500000000000000 ) ) ;
#10509 = CARTESIAN_POINT ( 'NONE',  ( 94.33688103937537051, 114.1144967660473242, -46.70000000546237828 ) ) ;
#10510 = EDGE_CURVE ( 'NONE', #5473, #6416, #22255, .T. ) ;
#10511 = CARTESIAN_POINT ( 'NONE',  ( 208.1451861577817795, 38.51953125108393294, 5.444914386472293977 ) ) ;
#10512 = CARTESIAN_POINT ( 'NONE',  ( -9.598844408820458085, 38.51953124999999289, -9.598844408820458085 ) ) ;
#10513 = CARTESIAN_POINT ( 'NONE',  ( 120.7049497278729575, 38.86679687608393863, -9.295050272127046043 ) ) ;
#10514 = DIRECTION ( 'NONE',  ( -0.000000000000000000, 1.000000000000000000, -0.000000000000000000 ) ) ;
#10515 = CARTESIAN_POINT ( 'NONE',  ( 94.99999999999995737, 2.071067811865491493, 6.937499999999999112 ) ) ;
#10516 = CARTESIAN_POINT ( 'NONE',  ( 95.54126587499999346, 94.74999999863439371, -1.846868145590737864 ) ) ;
#10517 = CARTESIAN_POINT ( 'NONE',  ( 99.99999999999998579, 89.99899999999999523, -2.500000000000004885 ) ) ;
#10518 = CARTESIAN_POINT ( 'NONE',  ( 98.96446609406727646, 123.2500000000000000, -2.499999999999997780 ) ) ;
#10519 = ADVANCED_FACE ( 'NONE', ( #10040 ), #14594, .T. ) ;
#10520 = CARTESIAN_POINT ( 'NONE',  ( 181.4251840539369596, 36.18789062499999432, -5.622872871577873077 ) ) ;
#10521 = CONTEXT_DEPENDENT_SHAPE_REPRESENTATION ( #22626, #3099 ) ;
#10522 = CARTESIAN_POINT ( 'NONE',  ( 126.8638263786525044, 36.00000000000000711, 12.79489613812760851 ) ) ;
#10523 = CARTESIAN_POINT ( 'NONE',  ( 104.4587341249999781, 1.846868145590750299, 3.250000001365592528 ) ) ;
#10524 = CARTESIAN_POINT ( 'NONE',  ( 55.70494972787295751, 38.07304687608393579, -9.295050272127046043 ) ) ;
#10525 = EDGE_CURVE ( 'NONE', #23799, #8723, #14739, .T. ) ;
#10526 = CARTESIAN_POINT ( 'NONE',  ( 104.4587341249999781, -1.846868145590721655, 6.875000001365592972 ) ) ;
#10527 = CARTESIAN_POINT ( 'NONE',  ( 107.0000000000000142, 107.7255621263696526, -43.60000000546237686 ) ) ;
#10528 = CARTESIAN_POINT ( 'NONE',  ( 104.4587341249999781, 94.31249999863440792, -6.938893903907228378E-15 ) ) ;
#10529 = FACE_BOUND ( 'NONE', #3637, .T. ) ;
#10530 = CARTESIAN_POINT ( 'NONE',  ( -9.598844408820458085, 40.90078124999999432, -9.598844408820458085 ) ) ;
#10531 = CARTESIAN_POINT ( 'NONE',  ( 107.0000000000000142, 110.0000000000000000, -45.00000000000000711 ) ) ;
#10532 = ADVANCED_FACE ( 'NONE', ( #27731 ), #9904, .T. ) ;
#10533 = ORIENTED_EDGE ( 'NONE', *, *, #11012, .F. ) ;
#10534 = CARTESIAN_POINT ( 'NONE',  ( 103.1528011352953342, 83.06250000136560629, 3.152801135295355106 ) ) ;
#10535 = ORIENTED_EDGE ( 'NONE', *, *, #24994, .T. ) ;
#10536 = ADVANCED_FACE ( 'NONE', ( #12312, #8191 ), #14729, .T. ) ;
#10537 = CARTESIAN_POINT ( 'NONE',  ( 95.67376207875069838, 104.0454443415356991, -46.70000000000000284 ) ) ;
#10538 = CARTESIAN_POINT ( 'NONE',  ( 78.14518615778179367, 35.54296875108394715, 5.444914386472293977 ) ) ;
#10539 = ORIENTED_EDGE ( 'NONE', *, *, #28153, .F. ) ;
#10540 =( BOUNDED_SURFACE ( )  B_SPLINE_SURFACE ( 1, 2, ( 
 ( #15907, #9364, #20068, #2955, #5103, #14058, #11772, #9227, #20497, #15774, #15636, #24626, #22489, #26773, #1120, #26917, #22348, #16201, #13628, #27058, #3247, #18058, #17920, #26631, #18350, #16055, #7078, #20352, #13766, #7217, #24480, #837, #980, #7361, #4966, #24764, #2819, #13483, #11487, #17782, #26485, #20203, #7508, #24337, #24907, #5388, #22778, #11914, #20636, #6940, #4823, #22205, #690, #24777, #16069, #24918, #13922, #9241, #2967, #7669, #5258, #13499, #17933, #26931, #20511, #5115, #11788, #18073, #11358, #26643, #22650, #993, #9661, #11642, #7232, #4838, #7375, #7091, #2698, #15790, #16217, #3120, #20082, #18364, #22219, #13644, #16361, #27071, #9802, #7522, #24493, #18508, #5402, #20650, #14072, #22792, #3261, #2833, #15923, #4978, #11928, #22359, #1134, #20366, #851, #27214, #559, #11501, #20218, #703, #9376, #26787, #24641, #13780, #22502, #9523, #18223, #8218, #12199, #14622, #12063, #5548, #14213, #18648, #25333, #16908, #21342, #20788, #7811, #25062, #18781, #9933, #22931, #8081, #25606, #1269, #27759, #25476, #6090, #5819, #16776, #27353, #16503, #3392, #10486, #19194, #14489, #12345, #23206, #10343, #12474, #19050, #14757, #23477, #25197, #3681, #21063, #1821, #21201, #5683, #1684, #23064, #14349, #1551, #10204, #18914, #8357, #5955, #1410, #3957, #20927, #12617, #27897, #16641, #3542, #10069, #27488, #23340, #7945, #27623, #3814, #8643, #10626 ),
 ( #12757, #10762, #380, #25747, #8501, #26026, #23617, #17332, #21764, #15319, #17608, #4371, #21908, #2383, #6497, #8920, #11041, #25893, #24033, #21478, #17466, #17043, #6363, #26316, #12888, #10903, #1957, #2094, #28172, #19896, #6229, #2241, #4094, #19750, #13027, #15462, #19331, #233, #19473, #15173, #97, #26168, #14896, #6635, #28034, #4512, #23752, #13169, #23892, #15035, #8778, #19612, #21618, #6777, #24177, #4654, #17186, #4230, #13315, #22041, #2516, #11178, #24603, #10004, #16570, #17897, #7190, #667, #2932, #26606, #12271, #16028, #22326, #15609, #2661, #26892, #25125, #5612, #15888, #11464, #9064, #11602, #22181, #6916, #11322, #20858, #20325, #24311, #7339, #17759, #7052, #20997, #813, #14421, #9481, #20043, #23136, #18182, #25261, #14278, #3466, #7876, #15751, #20183, #522, #18713, #9203, #1340, #5081, #13743, #12132, #22996, #27413, #5752, #24454, #4940, #3612, #9340, #26462, #4797, #18035, #13604, #13455, #2797, #26748, #22467, #10134, #18846, #23277, #1756, #21556, #25965, #25410, #12412, #1478, #23411, #14562, #8289, #6438, #5892, #27555, #3750, #15107, #25822, #6027, #21132, #4169, #14973, #1897, #27694, #4308, #21419, #12965, #6296, #10699, #8012, #16713, #14691, #14828, #6162, #17264, #18984, #12829, #23692, #3885, #21273, #1617, #27835, #23552, #10275, #2030, #19272, #8156, #27971, #16848, #25547, #12546, #19405, #16981, #23828, #10422, #4029, #28110 ) ),
 .UNSPECIFIED., .F., .F., .F. ) 
 B_SPLINE_SURFACE_WITH_KNOTS ( ( 2, 2 ),
 ( 3, 2, 2, 2, 2, 2, 2, 2, 2, 2, 2, 2, 2, 2, 2, 2, 2, 2, 2, 2, 2, 2, 2, 2, 2, 2, 2, 2, 2, 2, 2, 2, 2, 2, 2, 2, 2, 2, 2, 2, 2, 2, 2, 2, 2, 2, 2, 2, 2, 2, 2, 2, 2, 2, 2, 2, 2, 2, 2, 2, 2, 2, 2, 2, 2, 2, 2, 2, 2, 2, 2, 2, 2, 2, 2, 2, 2, 2, 2, 2, 2, 2, 2, 2, 2, 2, 2, 2, 2, 2, 2, 3 ),
 ( 0.000000000000000000, 1.000000000000000000 ),
 ( 0.000000000000000000, 0.01041666666666666609, 0.02083333333333333218, 0.03125000000000000000, 0.04166666666666666435, 0.05208333333333333565, 0.06250000000000000000, 0.07291666666666667129, 0.08333333333333332871, 0.09375000000000000000, 0.1041666666666666713, 0.1145833333333333287, 0.1250000000000000000, 0.1354166666666666574, 0.1458333333333333426, 0.1562500000000000000, 0.1666666666666666574, 0.1770833333333333426, 0.1875000000000000000, 0.1979166666666666574, 0.2083333333333333426, 0.2187500000000000000, 0.2291666666666666574, 0.2395833333333333426, 0.2500000000000000000, 0.2604166666666666852, 0.2708333333333333148, 0.2812500000000000000, 0.2916666666666666852, 0.3020833333333333148, 0.3125000000000000000, 0.3229166666666666852, 0.3333333333333333148, 0.3437500000000000000, 0.3541666666666666852, 0.3645833333333333148, 0.3750000000000000000, 0.3854166666666666852, 0.3958333333333333148, 0.4062500000000000000, 0.4166666666666666852, 0.4270833333333333148, 0.4375000000000000000, 0.4479166666666666852, 0.4583333333333333148, 0.4687500000000000000, 0.4791666666666666852, 0.4895833333333333148, 0.5000000000000000000, 0.5104166666666666297, 0.5208333333333333703, 0.5312500000000000000, 0.5416666666666666297, 0.5520833333333333703, 0.5625000000000000000, 0.5729166666666666297, 0.5833333333333333703, 0.5937500000000000000, 0.6041666666666666297, 0.6145833333333333703, 0.6250000000000000000, 0.6354166666666666297, 0.6458333333333333703, 0.6562500000000000000, 0.6666666666666666297, 0.6770833333333333703, 0.6875000000000000000, 0.6979166666666666297, 0.7083333333333333703, 0.7187500000000000000, 0.7291666666666666297, 0.7395833333333333703, 0.7500000000000000000, 0.7604166666666666297, 0.7708333333333333703, 0.7812500000000000000, 0.7916666666666666297, 0.8020833333333333703, 0.8125000000000000000, 0.8229166666666666297, 0.8333333333333333703, 0.8437500000000000000, 0.8541666666666666297, 0.8645833333333333703, 0.8750000000000000000, 0.8854166666666666297, 0.8958333333333333703, 0.9062500000000000000, 0.9166666666666666297, 0.9270833333333333703, 0.9375000000000000000, 0.9448586970929392370 ),
 .UNSPECIFIED. ) 
 GEOMETRIC_REPRESENTATION_ITEM ( )  RATIONAL_B_SPLINE_SURFACE ( (
 ( 1.000000000000000000, 0.9238795325112867385, 1.000000000000000000, 0.9238795325112867385, 1.000000000000000000, 0.9238795325112867385, 1.000000000000000000, 0.9238795325112867385, 1.000000000000000000, 0.9238795325112867385, 1.000000000000000000, 0.9238795325112867385, 1.000000000000000000, 0.9238795325112867385, 1.000000000000000000, 0.9238795325112867385, 1.000000000000000000, 0.9238795325112867385, 1.000000000000000000, 0.9238795325112867385, 1.000000000000000000, 0.9238795325112867385, 1.000000000000000000, 0.9238795325112867385, 1.000000000000000000, 0.9238795325112867385, 1.000000000000000000, 0.9238795325112867385, 1.000000000000000000, 0.9238795325112867385, 1.000000000000000000, 0.9238795325112867385, 1.000000000000000000, 0.9238795325112867385, 1.000000000000000000, 0.9238795325112867385, 1.000000000000000000, 0.9238795325112867385, 1.000000000000000000, 0.9238795325112867385, 1.000000000000000000, 0.9238795325112867385, 1.000000000000000000, 0.9238795325112867385, 1.000000000000000000, 0.9238795325112867385, 1.000000000000000000, 0.9238795325112867385, 1.000000000000000000, 0.9238795325112867385, 1.000000000000000000, 0.9238795325112867385, 1.000000000000000000, 0.9238795325112867385, 1.000000000000000000, 0.9238795325112867385, 1.000000000000000000, 0.9238795325112867385, 1.000000000000000000, 0.9238795325112867385, 1.000000000000000000, 0.9238795325112867385, 1.000000000000000000, 0.9238795325112867385, 1.000000000000000000, 0.9238795325112867385, 1.000000000000000000, 0.9238795325112867385, 1.000000000000000000, 0.9238795325112867385, 1.000000000000000000, 0.9238795325112867385, 1.000000000000000000, 0.9238795325112867385, 1.000000000000000000, 0.9238795325112867385, 1.000000000000000000, 0.9238795325112867385, 1.000000000000000000, 0.9238795325112867385, 1.000000000000000000, 0.9238795325112867385, 1.000000000000000000, 0.9238795325112867385, 1.000000000000000000, 0.9238795325112867385, 1.000000000000000000, 0.9238795325112867385, 1.000000000000000000, 0.9238795325112867385, 1.000000000000000000, 0.9238795325112867385, 1.000000000000000000, 0.9238795325112867385, 1.000000000000000000, 0.9238795325112867385, 1.000000000000000000, 0.9238795325112867385, 1.000000000000000000, 0.9238795325112867385, 1.000000000000000000, 0.9238795325112867385, 1.000000000000000000, 0.9238795325112867385, 1.000000000000000000, 0.9238795325112867385, 1.000000000000000000, 0.9238795325112867385, 1.000000000000000000, 0.9238795325112867385, 1.000000000000000000, 0.9238795325112867385, 1.000000000000000000, 0.9238795325112867385, 1.000000000000000000, 0.9238795325112867385, 1.000000000000000000, 0.9238795325112867385, 1.000000000000000000, 0.9238795325112867385, 1.000000000000000000, 0.9238795325112867385, 1.000000000000000000, 0.9238795325112867385, 1.000000000000000000, 0.9238795325112867385, 1.000000000000000000, 0.9238795325112867385, 1.000000000000000000, 0.9238795325112867385, 1.000000000000000000, 0.9238795325112867385, 1.000000000000000000, 0.9238795325112867385, 1.000000000000000000, 0.9238795325112867385, 1.000000000000000000, 0.9238795325112867385, 1.000000000000000000, 0.9238795325112867385, 1.000000000000000000, 0.9238795325112867385, 1.000000000000000000, 0.9238795325112867385, 1.000000000000000000, 0.9238795325112867385, 1.000000000000000000, 0.9238795325112867385, 1.000000000000000000, 0.9238795325112867385, 1.000000000000000000, 0.9238795325112867385, 1.000000000000000000, 0.9238795325112867385, 1.000000000000000000, 0.9238795325112867385, 1.000000000000000000, 0.9238795325112867385, 1.000000000000000000, 0.9238795325112867385, 1.000000000000000000, 0.9238795325112867385, 1.000000000000000000, 0.9238795325112867385, 1.000000000000000000, 0.9238795325112867385, 1.000000000000000000, 0.9238795325112867385, 1.000000000000000000, 0.9238795325112867385, 1.000000000000000000, 0.9238795325112867385, 1.000000000000000000, 0.9238795325112867385, 1.000000000000000000, 0.9238795325112867385, 1.000000000000000000, 0.9238795325112867385, 1.000000000000000000, 0.9238795325112867385, 1.000000000000000000, 0.9462258435690522607, 0.9684275710300105366),
 ( 1.000000000000000000, 0.9238795325112867385, 1.000000000000000000, 0.9238795325112867385, 1.000000000000000000, 0.9238795325112867385, 1.000000000000000000, 0.9238795325112867385, 1.000000000000000000, 0.9238795325112867385, 1.000000000000000000, 0.9238795325112867385, 1.000000000000000000, 0.9238795325112867385, 1.000000000000000000, 0.9238795325112867385, 1.000000000000000000, 0.9238795325112867385, 1.000000000000000000, 0.9238795325112867385, 1.000000000000000000, 0.9238795325112867385, 1.000000000000000000, 0.9238795325112867385, 1.000000000000000000, 0.9238795325112867385, 1.000000000000000000, 0.9238795325112867385, 1.000000000000000000, 0.9238795325112867385, 1.000000000000000000, 0.9238795325112867385, 1.000000000000000000, 0.9238795325112867385, 1.000000000000000000, 0.9238795325112867385, 1.000000000000000000, 0.9238795325112867385, 1.000000000000000000, 0.9238795325112867385, 1.000000000000000000, 0.9238795325112867385, 1.000000000000000000, 0.9238795325112867385, 1.000000000000000000, 0.9238795325112867385, 1.000000000000000000, 0.9238795325112867385, 1.000000000000000000, 0.9238795325112867385, 1.000000000000000000, 0.9238795325112867385, 1.000000000000000000, 0.9238795325112867385, 1.000000000000000000, 0.9238795325112867385, 1.000000000000000000, 0.9238795325112867385, 1.000000000000000000, 0.9238795325112867385, 1.000000000000000000, 0.9238795325112867385, 1.000000000000000000, 0.9238795325112867385, 1.000000000000000000, 0.9238795325112867385, 1.000000000000000000, 0.9238795325112867385, 1.000000000000000000, 0.9238795325112867385, 1.000000000000000000, 0.9238795325112867385, 1.000000000000000000, 0.9238795325112867385, 1.000000000000000000, 0.9238795325112867385, 1.000000000000000000, 0.9238795325112867385, 1.000000000000000000, 0.9238795325112867385, 1.000000000000000000, 0.9238795325112867385, 1.000000000000000000, 0.9238795325112867385, 1.000000000000000000, 0.9238795325112867385, 1.000000000000000000, 0.9238795325112867385, 1.000000000000000000, 0.9238795325112867385, 1.000000000000000000, 0.9238795325112867385, 1.000000000000000000, 0.9238795325112867385, 1.000000000000000000, 0.9238795325112867385, 1.000000000000000000, 0.9238795325112867385, 1.000000000000000000, 0.9238795325112867385, 1.000000000000000000, 0.9238795325112867385, 1.000000000000000000, 0.9238795325112867385, 1.000000000000000000, 0.9238795325112867385, 1.000000000000000000, 0.9238795325112867385, 1.000000000000000000, 0.9238795325112867385, 1.000000000000000000, 0.9238795325112867385, 1.000000000000000000, 0.9238795325112867385, 1.000000000000000000, 0.9238795325112867385, 1.000000000000000000, 0.9238795325112867385, 1.000000000000000000, 0.9238795325112867385, 1.000000000000000000, 0.9238795325112867385, 1.000000000000000000, 0.9238795325112867385, 1.000000000000000000, 0.9238795325112867385, 1.000000000000000000, 0.9238795325112867385, 1.000000000000000000, 0.9238795325112867385, 1.000000000000000000, 0.9238795325112867385, 1.000000000000000000, 0.9238795325112867385, 1.000000000000000000, 0.9238795325112867385, 1.000000000000000000, 0.9238795325112867385, 1.000000000000000000, 0.9238795325112867385, 1.000000000000000000, 0.9238795325112867385, 1.000000000000000000, 0.9238795325112867385, 1.000000000000000000, 0.9238795325112867385, 1.000000000000000000, 0.9238795325112867385, 1.000000000000000000, 0.9238795325112867385, 1.000000000000000000, 0.9238795325112867385, 1.000000000000000000, 0.9238795325112867385, 1.000000000000000000, 0.9238795325112867385, 1.000000000000000000, 0.9238795325112867385, 1.000000000000000000, 0.9238795325112867385, 1.000000000000000000, 0.9238795325112867385, 1.000000000000000000, 0.9238795325112867385, 1.000000000000000000, 0.9238795325112867385, 1.000000000000000000, 0.9238795325112867385, 1.000000000000000000, 0.9238795325112867385, 1.000000000000000000, 0.9238795325112867385, 1.000000000000000000, 0.9238795325112867385, 1.000000000000000000, 0.9238795325112867385, 1.000000000000000000, 0.9238795325112867385, 1.000000000000000000, 0.9238795325112867385, 1.000000000000000000, 0.9462258435690522607, 0.9684275710300105366) ) ) 
 REPRESENTATION_ITEM ( '' )  SURFACE ( )  );
#10541 = CARTESIAN_POINT ( 'NONE',  ( 104.4587341249999781, 1.846868145590750299, 1.250000001365592750 ) ) ;
#10542 = VERTEX_POINT ( 'NONE', #23174 ) ;
#10543 = CARTESIAN_POINT ( 'NONE',  ( -9.295050272127046043, 35.89023437608393152, -9.295050272127046043 ) ) ;
#10544 = CARTESIAN_POINT ( 'NONE',  ( 5.444914386472297529, 33.95546875108393436, -13.14518615778179900 ) ) ;
#10545 = CARTESIAN_POINT ( 'NONE',  ( 181.4251840539369596, 36.33671875216787583, 0.000000000000000000 ) ) ;
#10546 = CARTESIAN_POINT ( 'NONE',  ( -9.295050272127046043, 38.07304687608393579, -9.295050272127046043 ) ) ;
#10547 = DIRECTION ( 'NONE',  ( 0.8660254037844407060, 0.4999999999999963363, 0.000000000000000000 ) ) ;
#10548 = CARTESIAN_POINT ( 'NONE',  ( 190.9374164594231615, 50.00000000116092735, 12.98908657125209665 ) ) ;
#10549 = ADVANCED_FACE ( 'NONE', ( #8328 ), #27322, .T. ) ;
#10550 = CARTESIAN_POINT ( 'NONE',  ( 143.1451861577818079, 38.76757812608393294, -1.609821015232357215E-15 ) ) ;
#10551 = CARTESIAN_POINT ( 'NONE',  ( -13.14518615778179544, 37.57695312608393579, 0.000000000000000000 ) ) ;
#10552 = ORIENTED_EDGE ( 'NONE', *, *, #11729, .T. ) ;
#10553 = CARTESIAN_POINT ( 'NONE',  ( 74.59884440882045453, 38.32109374999999574, -9.598844408820458085 ) ) ;
#10554 = DIRECTION ( 'NONE',  ( 0.8660254037844380415, 0.5000000000000013323, 0.000000000000000000 ) ) ;
#10555 = EDGE_CURVE ( 'NONE', #7171, #4924, #18880, .T. ) ;
#10556 = CARTESIAN_POINT ( 'NONE',  ( 101.8468681455906903, -4.458734124999987891, 0.7500000013655925279 ) ) ;
#10557 = CARTESIAN_POINT ( 'NONE',  ( 94.99999999999995737, 84.12500000273119838, -1.387778780781445676E-14 ) ) ;
#10559 = EDGE_CURVE ( 'NONE', #2183, #13505, #18669, .T. ) ;
#10558 = CARTESIAN_POINT ( 'NONE',  ( 104.4587341249999639, 1.442382525525748735E-14, 5.937500001365592084 ) ) ;
#10560 = CARTESIAN_POINT ( 'NONE',  ( 108.0825317500000153, 110.0000000000000000, -50.12500000273119127 ) ) ;
#10561 = CARTESIAN_POINT ( 'NONE',  ( 104.4587341249999781, -1.846868145590721655, 3.125000001365592528 ) ) ;
#10562 = CARTESIAN_POINT ( 'NONE',  ( 101.8468681455907046, 80.00000000136560629, 4.458734124999987891 ) ) ;
#10563 = CARTESIAN_POINT ( 'NONE',  ( 93.46109445667489979, 114.7507929638356785, -45.82499999726881867 ) ) ;
#10564 = CARTESIAN_POINT ( 'NONE',  ( -13.14518615778179189, 38.42031250108393436, 5.444914386472304635 ) ) ;
#10565 = ADVANCED_FACE ( 'NONE', ( #3785 ), #26000, .T. ) ;
#10566 = CARTESIAN_POINT ( 'NONE',  ( 104.9952793366501709, 116.8754121666685393, -46.57499999726881157 ) ) ;
#10567 = EDGE_LOOP ( 'NONE', ( #18325, #19276 ) ) ;
#10568 = CARTESIAN_POINT ( 'NONE',  ( -13.14518615778179189, 32.86406250108393579, 5.444914386472304635 ) ) ;
#10569 = DIRECTION ( 'NONE',  ( -0.000000000000000000, 1.000000000000000000, -0.000000000000000000 ) ) ;
#10570 = CARTESIAN_POINT ( 'NONE',  ( 104.9999999999999574, 2.071067811865511032, 5.562500000000000888 ) ) ;
#10571 = CARTESIAN_POINT ( 'NONE',  ( 99.99999999999997158, 101.5015231886685854, -53.37499999726883004 ) ) ;
#10572 = CARTESIAN_POINT ( 'NONE',  ( -13.57481594606304753, 37.08085937716787583, -5.622872871577872189 ) ) ;
#10573 = CARTESIAN_POINT ( 'NONE',  ( 185.7049497278729575, 39.66054687608393436, -9.295050272127046043 ) ) ;
#10574 = EDGE_LOOP ( 'NONE', ( #20522, #21819, #9847, #5998 ) ) ;
#10575 = DIRECTION ( 'NONE',  ( 1.000000000000000000, 0.000000000000000000, -2.385244779468110248E-16 ) ) ;
#10576 = DIRECTION ( 'NONE',  ( -0.000000000000000000, -0.000000000000000000, -1.000000000000000000 ) ) ;
#10577 = CARTESIAN_POINT ( 'NONE',  ( 58.92091997948118376, 54.65154858643462887, -15.00000000000000355 ) ) ;
#10578 = EDGE_LOOP ( 'NONE', ( #16832, #12852, #3728, #3271, #22365, #26400, #11510, #9586 ) ) ;
#10579 = CARTESIAN_POINT ( 'NONE',  ( 102.1631189606246295, 103.3426043859339103, -49.40000000000000568 ) ) ;
#10580 = CARTESIAN_POINT ( 'NONE',  ( -9.180175813648011385, 50.00000000000000000, -9.999999999999978684 ) ) ;
#10581 = CARTESIAN_POINT ( 'NONE',  ( 99.99999999999998579, 124.5500000010924708, -2.066987299999998751 ) ) ;
#10582 = AXIS2_PLACEMENT_3D ( 'NONE', #12297, #20881, #3210 ) ;
#10583 = CARTESIAN_POINT ( 'NONE',  ( 116.4251840539369596, 35.54296875216788010, 0.000000000000000000 ) ) ;
#10584 =( BOUNDED_SURFACE ( )  B_SPLINE_SURFACE ( 3, 2, ( 
 ( #23740, #2225, #28019 ),
 ( #23876, #12872, #17312 ),
 ( #21602, #8485, #6764 ),
 ( #8341, #14881, #2080 ),
 ( #24020, #19459, #4498 ),
 ( #25876, #79, #26012 ),
 ( #4354, #4215, #15447 ),
 ( #6619, #2367, #25729 ),
 ( #17595, #6483, #26302 ),
 ( #23596, #2503, #13010 ),
 ( #24162, #11024, #19736 ),
 ( #10889, #19177, #8906 ),
 ( #22025, #12741, #4639 ),
 ( #21749, #10748, #19596 ),
 ( #13298, #27880, #26152 ),
 ( #17027, #21465, #1942 ),
 ( #10611, #19318, #17174 ),
 ( #15020, #28157, #15304 ),
 ( #20030, #940, #11164 ),
 ( #16015, #5351, #24585 ) ),
 .UNSPECIFIED., .F., .F., .T. ) 
 B_SPLINE_SURFACE_WITH_KNOTS ( ( 4, 2, 2, 2, 2, 2, 2, 2, 2, 4 ),
 ( 3, 3 ),
 ( 0.009073803551359458167, 0.01139250602759180747, 0.01371120850382415851, 0.01602991098005650955, 0.01834861345628885712, 0.01950796469440502917, 0.02066731593252120469, 0.02298601840875355573, 0.02530472088498590677, 0.02762342336121825434 ),
 ( 0.000000000000000000, 1.000000000000000000 ),
 .UNSPECIFIED. ) 
 GEOMETRIC_REPRESENTATION_ITEM ( )  RATIONAL_B_SPLINE_SURFACE ( (
 ( 1.000000000000000000, 0.7071067811865482389, 1.000000000000000000),
 ( 1.000000000000000000, 0.7344871497829537077, 1.000000000000000000),
 ( 1.000000000000000000, 0.7612510203318018087, 1.000000000000000000),
 ( 1.000000000000000000, 0.8116663633844866110, 1.000000000000000000),
 ( 1.000000000000000000, 0.8353358059749917963, 1.000000000000000000),
 ( 1.000000000000000000, 0.8764699612587962818, 1.000000000000000000),
 ( 1.000000000000000000, 0.8939017358718740480, 1.000000000000000000),
 ( 1.000000000000000000, 0.9185314935647553858, 1.000000000000000000),
 ( 1.000000000000000000, 0.9256439951239483488, 1.000000000000000000),
 ( 1.000000000000000000, 0.9261623622476518047, 1.000000000000000000),
 ( 1.000000000000000000, 0.9246301385978411558, 1.000000000000000000),
 ( 1.000000000000000000, 0.9183304321348458865, 1.000000000000000000),
 ( 1.000000000000000000, 0.9135987334167114948, 1.000000000000000000),
 ( 1.000000000000000000, 0.8954110486042292649, 1.000000000000000000),
 ( 1.000000000000000000, 0.8779877431164835322, 1.000000000000000000),
 ( 1.000000000000000000, 0.8366182664708665673, 1.000000000000000000),
 ( 1.000000000000000000, 0.8126941604013132592, 1.000000000000000000),
 ( 1.000000000000000000, 0.7617527316308130292, 1.000000000000000000),
 ( 1.000000000000000000, 0.7347103785790367603, 1.000000000000000000),
 ( 1.000000000000000000, 0.7071067811865459074, 1.000000000000000000) ) ) 
 REPRESENTATION_ITEM ( '' )  SURFACE ( )  );
#10585 = CARTESIAN_POINT ( 'NONE',  ( 102.0710678118654045, 81.43750000273119838, 5.000000000000019540 ) ) ;
#10586 = DIRECTION ( 'NONE',  ( 0.000000000000000000, 0.000000000000000000, 1.000000000000000000 ) ) ;
#10587 = CARTESIAN_POINT ( 'NONE',  ( 200.4449143864723055, 34.65000000108393863, 13.14518615778179189 ) ) ;
#10588 = VERTEX_POINT ( 'NONE', #4342 ) ;
#10589 = ORIENTED_EDGE ( 'NONE', *, *, #151, .T. ) ;
#10590 = ORIENTED_EDGE ( 'NONE', *, *, #16450, .F. ) ;
#10591 = CARTESIAN_POINT ( 'NONE',  ( 13.14518615778179900, 38.71796875108393721, 5.444914386472293977 ) ) ;
#10592 = CARTESIAN_POINT ( 'NONE',  ( 97.92893218813449607, 84.18750000000000000, 4.999999999999981348 ) ) ;
#10593 = CARTESIAN_POINT ( 'NONE',  ( 51.85481384221821344, 39.80937500108393579, 5.444914386472304635 ) ) ;
#10594 = CARTESIAN_POINT ( 'NONE',  ( 51.42518405393695957, 36.38632812716788578, 5.622872871577880183 ) ) ;
#10595 = FACE_OUTER_BOUND ( 'NONE', #17560, .T. ) ;
#10596 = CARTESIAN_POINT ( 'NONE',  ( -5.444914386472299306, 40.10703125108393152, 13.14518615778179722 ) ) ;
#10597 = CARTESIAN_POINT ( 'NONE',  ( 99.99999999999995737, 1.387778780781445676E-14, 34.79898987322334136 ) ) ;
#10598 = CARTESIAN_POINT ( 'NONE',  ( 99.99999999999998579, 123.2000000000000028, -2.499999999999997780 ) ) ;
#10599 = CARTESIAN_POINT ( 'NONE',  ( 189.5550856135277229, 39.80937500108393579, -13.14518615778179722 ) ) ;
#10600 = CARTESIAN_POINT ( 'NONE',  ( 93.46109445667489979, 114.7507929638356785, -47.82499999726882578 ) ) ;
#10601 = VECTOR ( 'NONE', #2629, 1000.000000000000000 ) ;
#10602 = VERTEX_POINT ( 'NONE', #9037 ) ;
#10603 = CARTESIAN_POINT ( 'NONE',  ( -5.622872871577873077, 39.56132812499999574, 13.57481594606304753 ) ) ;
#10604 = CARTESIAN_POINT ( 'NONE',  ( 5.622872871577871301, 32.11992187716787583, -13.57481594606304753 ) ) ;
#10605 = CARTESIAN_POINT ( 'NONE',  ( 94.99999999999995737, 1.387778780781445676E-14, 0.1250000027311851669 ) ) ;
#10606 = CARTESIAN_POINT ( 'NONE',  ( 116.8548138422182205, 37.57695312608393579, 0.000000000000000000 ) ) ;
#10607 = CARTESIAN_POINT ( 'NONE',  ( 78.14518615778179367, 36.23750000108393010, -5.444914386472297529 ) ) ;
#10608 = CARTESIAN_POINT ( 'NONE',  ( 208.1451861577817795, 32.26875000108393721, -5.444914386472297529 ) ) ;
#10609 = FACE_OUTER_BOUND ( 'NONE', #26507, .T. ) ;
#10610 = CARTESIAN_POINT ( 'NONE',  ( 13.14518615778179544, 34.60039062608392868, -1.609821015232357215E-15 ) ) ;
#10611 = CARTESIAN_POINT ( 'NONE',  ( 122.9105827276628418, 49.99999999943648987, -11.59823041028630364 ) ) ;
#10612 = CARTESIAN_POINT ( 'NONE',  ( -8.312177448680279460E-16, 38.51953125216787299, -13.57481594606304576 ) ) ;
#10613 = DIRECTION ( 'NONE',  ( -0.000000000000000000, 1.000000000000000000, -0.000000000000000000 ) ) ;
#10614 = CARTESIAN_POINT ( 'NONE',  ( -8.049105076161786076E-16, 39.56132812608393579, -13.14518615778179544 ) ) ;
#10615 =( BOUNDED_CURVE ( )  B_SPLINE_CURVE ( 2, ( #25593, #17175, #23464, #27606, #25317, #12601, #12330, #21326, #23191 ),
 .UNSPECIFIED., .F., .F. ) 
 B_SPLINE_CURVE_WITH_KNOTS ( ( 3, 2, 2, 2, 3 ),
 ( 0.06250000000000004163, 0.07291666666666665741, 0.08333333333333325932, 0.09374999999999987510, 0.1041666666666664909 ),
 .UNSPECIFIED. ) 
 CURVE ( )  GEOMETRIC_REPRESENTATION_ITEM ( )  RATIONAL_B_SPLINE_CURVE ( ( 0.9999999999999996669, 0.9238795325112870716, 1.000000000000000000, 0.9238795325112867385, 1.000000000000000000, 0.9238795325112867385, 1.000000000000000000, 0.9238795325112880708, 0.9999999999999986677 ) ) 
 REPRESENTATION_ITEM ( '' )  );
#10616 = CARTESIAN_POINT ( 'NONE',  ( 1.887528725876407965, 53.66306546785492060, 14.99999999999999822 ) ) ;
#10617 = CARTESIAN_POINT ( 'NONE',  ( 99.99999999999998579, 122.9000000021849530, 2.499999999999978684 ) ) ;
#10618 = CARTESIAN_POINT ( 'NONE',  ( 61.28346588621581503, 51.46663580899082291, 14.99999999999794298 ) ) ;
#10619 = CARTESIAN_POINT ( 'NONE',  ( 94.99999999999995737, 1.387778780781445676E-14, 34.79898987322334136 ) ) ;
#10620 = CARTESIAN_POINT ( 'NONE',  ( 99.99999999999995737, -4.458734124999988779, 9.687500001365593860 ) ) ;
#10621 = CARTESIAN_POINT ( 'NONE',  ( 99.99999999999995737, -4.999999999999990230, 13.37500000273118417 ) ) ;
#10622 = ORIENTED_EDGE ( 'NONE', *, *, #15237, .T. ) ;
#10623 = CARTESIAN_POINT ( 'NONE',  ( 95.67376207875072680, 104.0454443415356991, -50.19999999453764161 ) ) ;
#10624 = CARTESIAN_POINT ( 'NONE',  ( 96.84719886470459471, 3.152801135295383084, 12.31250000136559208 ) ) ;
#10625 = CARTESIAN_POINT ( 'NONE',  ( -13.14518615778179722, 31.77265625108393365, -5.444914386472297529 ) ) ;
#10626 = CARTESIAN_POINT ( 'NONE',  ( 7.171391395016640580, 31.30502190640808990, -11.52591746582321974 ) ) ;
#10627 = CARTESIAN_POINT ( 'NONE',  ( 120.4011555911795455, 38.81718750216787583, 9.598844408820459861 ) ) ;
#10628 = CARTESIAN_POINT ( 'NONE',  ( 101.8468681455906903, 80.75000000136560629, 4.458734124999987891 ) ) ;
#10629 = CARTESIAN_POINT ( 'NONE',  ( 55.70494972787295751, 39.06523437608392868, -9.295050272127046043 ) ) ;
#10630 = CARTESIAN_POINT ( 'NONE',  ( 95.00472066334982912, 103.1245878333314323, -50.82500000273118701 ) ) ;
#10631 = CARTESIAN_POINT ( 'NONE',  ( -5.444914386472299306, 39.90859375108392726, 13.14518615778179722 ) ) ;
#10632 = DIRECTION ( 'NONE',  ( 0.000000000000000000, 0.000000000000000000, 1.000000000000000000 ) ) ;
#10633 = CARTESIAN_POINT ( 'NONE',  ( 9.598844408820459861, 33.36015624999999574, 9.598844408820456309 ) ) ;
#10634 = CARTESIAN_POINT ( 'NONE',  ( 104.3262379212492448, 104.0454443415356991, -53.79999999453763593 ) ) ;
#10635 = CARTESIAN_POINT ( 'NONE',  ( 139.2950502721270425, 32.51679687608393721, -9.295050272127046043 ) ) ;
#10636 = ORIENTED_EDGE ( 'NONE', *, *, #12253, .F. ) ;
#10637 = LINE ( 'NONE', #6374, #10827 ) ;
#10638 = CARTESIAN_POINT ( 'NONE',  ( -5.444914386472299306, 38.51953125108393294, 13.14518615778179722 ) ) ;
#10639 = CARTESIAN_POINT ( 'NONE',  ( 95.54126587499995082, 81.37500000136563472, -1.846868145590750077 ) ) ;
#10640 = CARTESIAN_POINT ( 'NONE',  ( 130.0000000000000000, 36.38632812608393152, -13.14518615778179544 ) ) ;
#10641 = CARTESIAN_POINT ( 'NONE',  ( 70.62287287157786864, 37.67617187716787441, -13.57481594606304753 ) ) ;
#10642 = PRODUCT_DEFINITION ( 'UNKNOWN', '', #1314, #14319 ) ;
#10643 = EDGE_CURVE ( 'NONE', #27310, #1696, #11150, .T. ) ;
#10644 = CARTESIAN_POINT ( 'NONE',  ( 13.39333672780506035, 36.00000000000000000, -2.034633736484789068 ) ) ;
#10645 = CARTESIAN_POINT ( 'NONE',  ( 9.598844408820459861, 35.04687500216787299, 9.598844408820456309 ) ) ;
#10646 = CARTESIAN_POINT ( 'NONE',  ( 104.9999999999999574, 2.071067811865491937, 6.562499999999998224 ) ) ;
#10647 = CARTESIAN_POINT ( 'NONE',  ( 94.99999999999995737, 1.387778780781445676E-14, 1.999999999999998224 ) ) ;
#10648 = CARTESIAN_POINT ( 'NONE',  ( 181.8548138422181921, 36.53515625108392584, -5.444914386472297529 ) ) ;
#10649 = CARTESIAN_POINT ( 'NONE',  ( 78.57481594606305464, 39.06523437499999574, -5.622872871577873966 ) ) ;
#10650 = CARTESIAN_POINT ( 'NONE',  ( 99.99999999999998579, 92.75000000000000000, 4.999999999999984013 ) ) ;
#10651 = FACE_OUTER_BOUND ( 'NONE', #19260, .T. ) ;
#10652 = CARTESIAN_POINT ( 'NONE',  ( 208.5748159460630688, 39.11484375216787157, -1.662435489736055892E-15 ) ) ;
#10653 = CARTESIAN_POINT ( 'NONE',  ( 65.00000000000000000, 36.83281249999999574, -13.57481594606304576 ) ) ;
#10654 = CARTESIAN_POINT ( 'NONE',  ( 9.295050272127046043, 37.27929687608394005, -9.295050272127046043 ) ) ;
#10655 = CARTESIAN_POINT ( 'NONE',  ( -9.295050272127046043, 38.07304687608393579, -9.295050272127046043 ) ) ;
#10656 = CARTESIAN_POINT ( 'NONE',  ( 200.6228728715778686, 38.07304687499998863, 13.57481594606304576 ) ) ;
#10657 = CONTEXT_DEPENDENT_SHAPE_REPRESENTATION ( #13126, #5558 ) ;
#10658 = CARTESIAN_POINT ( 'NONE',  ( 97.50236033167492167, 102.3130555110000159, -44.97500000273119980 ) ) ;
#10659 = CARTESIAN_POINT ( 'NONE',  ( 101.8468681455906903, 4.458734125000016313, 4.375000001365592084 ) ) ;
#10660 = CARTESIAN_POINT ( 'NONE',  ( 51.85481384221820633, 37.42812500108393436, 5.444914386472304635 ) ) ;
#10661 = CARTESIAN_POINT ( 'NONE',  ( 101.8468681455907046, 4.458734125000016313, 7.125000001365592084 ) ) ;
#10662 = CARTESIAN_POINT ( 'NONE',  ( 107.0000000000000142, 110.0000000000000000, -43.50000000546237544 ) ) ;
#10663 = CARTESIAN_POINT ( 'NONE',  ( 104.4587341249999923, 92.24999999863439371, 1.846868145590726318 ) ) ;
#10664 = CARTESIAN_POINT ( 'NONE',  ( -9.115657261794327226, 36.00000000000000711, 9.510219181138872102 ) ) ;
#10665 = CARTESIAN_POINT ( 'NONE',  ( -13.57481594606304753, 38.56914062500000284, -5.622872871577873077 ) ) ;
#10666 = CARTESIAN_POINT ( 'NONE',  ( 124.5550856135277087, 40.10703125108393152, 13.14518615778179722 ) ) ;
#10667 = ORIENTED_EDGE ( 'NONE', *, *, #5693, .F. ) ;
#10668 = CARTESIAN_POINT ( 'NONE',  ( 99.99999999999995737, 83.25000000000000000, 4.999999999999990230 ) ) ;
#10669 = CARTESIAN_POINT ( 'NONE',  ( 95.54126587500000767, 94.81249999863440792, -7.484931351350258973E-15 ) ) ;
#10670 = ORIENTED_EDGE ( 'NONE', *, *, #27379, .F. ) ;
#10671 = CARTESIAN_POINT ( 'NONE',  ( 195.0000000000000000, 37.72578125216787726, -13.57481594606304576 ) ) ;
#10672 = CARTESIAN_POINT ( 'NONE',  ( 59.55508561352770158, 33.45937500108394147, -13.14518615778179900 ) ) ;
#10673 = VERTEX_POINT ( 'NONE', #24148 ) ;
#10674 = ADVANCED_FACE ( 'NONE', ( #8611 ), #17583, .T. ) ;
#10675 = CARTESIAN_POINT ( 'NONE',  ( 126.9606029491974510, 53.88964894337311762, -14.99999999999999822 ) ) ;
#10676 = CARTESIAN_POINT ( 'NONE',  ( 99.99999999999995737, -4.458734124999988779, 1.937500001365591640 ) ) ;
#10677 = EDGE_CURVE ( 'NONE', #25390, #19945, #14909, .T. ) ;
#10678 = ORIENTED_EDGE ( 'NONE', *, *, #4769, .T. ) ;
#10679 = CARTESIAN_POINT ( 'NONE',  ( 9.295050272127047819, 35.49335937608393721, 9.295050272127046043 ) ) ;
#10680 = CARTESIAN_POINT ( 'NONE',  ( -13.14518615778179544, 38.37070312608393152, 0.000000000000000000 ) ) ;
#10681 = CARTESIAN_POINT ( 'NONE',  ( 189.3771271284221314, 36.18789062716787441, -13.57481594606304753 ) ) ;
#10682 = CARTESIAN_POINT ( 'NONE',  ( 5.444914386472302859, 36.03906250108393294, 13.14518615778179189 ) ) ;
#10683 = CARTESIAN_POINT ( 'NONE',  ( 102.4976396683250925, 102.3130555110000159, -44.52500000273119696 ) ) ;
#10684 = CARTESIAN_POINT ( 'NONE',  ( 105.6631189606246295, 105.8855032339526758, -51.20000000000000995 ) ) ;
#10685 = CARTESIAN_POINT ( 'NONE',  ( 124.5550856135277087, 38.51953125108393294, 13.14518615778179722 ) ) ;
#10686 = CARTESIAN_POINT ( 'NONE',  ( 5.444914386472297529, 38.91640625108393436, -13.14518615778179900 ) ) ;
#10687 = AXIS2_PLACEMENT_3D ( 'NONE', #25152, #16457, #5642 ) ;
#10688 = CARTESIAN_POINT ( 'NONE',  ( 120.7049497278729575, 34.30273437608393294, 9.295050272127047819 ) ) ;
#10689 = CARTESIAN_POINT ( 'NONE',  ( 78.57481594606304043, 39.06523437499998863, -5.622872871577873077 ) ) ;
#10690 = CARTESIAN_POINT ( 'NONE',  ( 116.8548138422182205, 40.55351562608393579, 0.000000000000000000 ) ) ;
#10691 = EDGE_CURVE ( 'NONE', #20441, #1383, #4485, .T. ) ;
#10692 = CARTESIAN_POINT ( 'NONE',  ( 96.84719886470459471, 3.152801135295383084, 1.312500001365592750 ) ) ;
#10693 = FACE_OUTER_BOUND ( 'NONE', #8844, .T. ) ;
#10694 = CARTESIAN_POINT ( 'NONE',  ( 99.99999999999995737, -4.458734124999988779, 3.687500001365591640 ) ) ;
#10695 = CARTESIAN_POINT ( 'NONE',  ( 99.99999999999998579, 101.5015231886685854, -50.62500000273119838 ) ) ;
#10696 = DIRECTION ( 'NONE',  ( -1.000000000000000000, 0.000000000000000000, 0.000000000000000000 ) ) ;
#10697 = CIRCLE ( 'NONE', #19828, 23.00000000000001421 ) ;
#10698 = CARTESIAN_POINT ( 'NONE',  ( 103.1528011352953342, 80.31250000136559208, -3.152801135295383084 ) ) ;
#10699 = CARTESIAN_POINT ( 'NONE',  ( 9.295050272127047819, 32.91367187608393152, 9.295050272127046043 ) ) ;
#10700 = CARTESIAN_POINT ( 'NONE',  ( -9.295050272127044266, 40.05742187608393579, 9.295050272127047819 ) ) ;
#10701 = CARTESIAN_POINT ( 'NONE',  ( 99.99999999999997158, 118.4984768113314004, -46.37499999726880873 ) ) ;
#10702 = EDGE_LOOP ( 'NONE', ( #18144, #3624, #8878, #24353 ) ) ;
#10703 = CARTESIAN_POINT ( 'NONE',  ( 102.1631189606246295, 116.6573956140660897, -51.10000000546237686 ) ) ;
#10704 =( BOUNDED_CURVE ( )  B_SPLINE_CURVE ( 2, ( #6620, #15306, #6765, #15983, #17596, #7583, #16276, #24974, #5459 ),
 .UNSPECIFIED., .F., .F. ) 
 B_SPLINE_CURVE_WITH_KNOTS ( ( 3, 2, 2, 2, 3 ),
 ( 0.1875000000000001388, 0.1979166666666667407, 0.2083333333333333703, 0.2187499999999999722, 0.2291666666666665741 ),
 .UNSPECIFIED. ) 
 CURVE ( )  GEOMETRIC_REPRESENTATION_ITEM ( )  RATIONAL_B_SPLINE_CURVE ( ( 0.9999999999999990008, 0.9238795325112877377, 1.000000000000000000, 0.9238795325112867385, 1.000000000000000000, 0.9238795325112867385, 1.000000000000000000, 0.9238795325112872936, 0.9999999999999994449 ) ) 
 REPRESENTATION_ITEM ( '' )  );
#10705 = CARTESIAN_POINT ( 'NONE',  ( 99.99999999999998579, 124.3500000010924822, -2.066987299999998751 ) ) ;
#10706 = CARTESIAN_POINT ( 'NONE',  ( 101.7677669209684552, 123.0000000000000000, 1.767766984964258992 ) ) ;
#10707 = CARTESIAN_POINT ( 'NONE',  ( 181.4251840539369596, 36.18789062499999432, -5.622872871577872189 ) ) ;
#10708 = EDGE_CURVE ( 'NONE', #17655, #23999, #197, .T. ) ;
#10709 = CARTESIAN_POINT ( 'NONE',  ( 181.8548138422182205, 39.75976562608393294, 0.000000000000000000 ) ) ;
#10710 = EDGE_LOOP ( 'NONE', ( #11833, #1091, #24150, #26261, #26547 ) ) ;
#10711 = CARTESIAN_POINT ( 'NONE',  ( 97.92893218813451028, -4.999999999999989342, 7.312500002731185056 ) ) ;
#10712 = CARTESIAN_POINT ( 'NONE',  ( 107.0000000000000000, 110.0000000000000000, -48.00000000000001421 ) ) ;
#10713 = FACE_OUTER_BOUND ( 'NONE', #18311, .T. ) ;
#10714 = EDGE_LOOP ( 'NONE', ( #20022, #4712, #19101, #1106 ) ) ;
#10715 = CARTESIAN_POINT ( 'NONE',  ( 93.00000000000000000, 110.0000000000000000, -52.00000000000000711 ) ) ;
#10716 = CARTESIAN_POINT ( 'NONE',  ( 9.295050272127047819, 38.46992187608393010, 9.295050272127046043 ) ) ;
#10717 = AXIS2_PLACEMENT_3D ( 'NONE', #103, #17473, #8785 ) ;
#10718 = CARTESIAN_POINT ( 'NONE',  ( 101.4615807364564546, 124.2500000010924737, 1.461580736456455476 ) ) ;
#10719 = EDGE_CURVE ( 'NONE', #15111, #28147, #4191, .T. ) ;
#10720 = CARTESIAN_POINT ( 'NONE',  ( 116.4251840539369454, 34.69960937716787441, -5.622872871577873077 ) ) ;
#10721 = CARTESIAN_POINT ( 'NONE',  ( 70.44491438647230552, 39.71015625108393010, -13.14518615778179900 ) ) ;
#10722 = CARTESIAN_POINT ( 'NONE',  ( 99.99999999999998579, 128.0000000000000000, -5.204170427930421283E-15 ) ) ;
#10723 = CARTESIAN_POINT ( 'NONE',  ( 189.5550856135277229, 33.75703125108393721, 13.14518615778179722 ) ) ;
#10724 = EDGE_LOOP ( 'NONE', ( #17087, #23388, #24045, #8318 ) ) ;
#10725 = EDGE_LOOP ( 'NONE', ( #27641, #21354, #15523, #7168, #9604, #13466, #16171, #25107, #23025, #1343, #21881, #2188, #12389, #15896, #7602 ) ) ;
#10726 = ORIENTED_EDGE ( 'NONE', *, *, #7041, .F. ) ;
#10727 = CARTESIAN_POINT ( 'NONE',  ( 13.14518615778179544, 37.97382812608393721, -1.609821015232357215E-15 ) ) ;
#10728 = SHAPE_REPRESENTATION_RELATIONSHIP ( 'NONE' , 'NONE' ,  #17883, #26371 ) ;
#10729 = CARTESIAN_POINT ( 'NONE',  ( 98.15313185440923860, 4.458734125000016313, 10.50000000136559208 ) ) ;
#10730 = CARTESIAN_POINT ( 'NONE',  ( 65.00000000000000000, 39.56132812608393579, -13.14518615778179544 ) ) ;
#10731 = CARTESIAN_POINT ( 'NONE',  ( 95.54126587499996504, 80.50000000136560629, 1.846868145590724986 ) ) ;
#10732 = CARTESIAN_POINT ( 'NONE',  ( 181.8548138422182205, 37.37851562608393863, 0.000000000000000000 ) ) ;
#10733 = DIRECTION ( 'NONE',  ( 0.000000000000000000, 0.000000000000000000, 1.000000000000000000 ) ) ;
#10734 = DIRECTION ( 'NONE',  ( 0.000000000000000000, 0.000000000000000000, 1.000000000000000000 ) ) ;
#10735 = CARTESIAN_POINT ( 'NONE',  ( 104.9999999999999716, 1.449011120738813565E-14, 12.49999999999999822 ) ) ;
#10736 = CARTESIAN_POINT ( 'NONE',  ( 65.00000000000000000, 39.61093749999999147, 13.57481594606304576 ) ) ;
#10737 = CARTESIAN_POINT ( 'NONE',  ( 102.4976396683250783, 102.3130555110000159, -53.02499999726882862 ) ) ;
#10738 = EDGE_LOOP ( 'NONE', ( #21172, #18691, #27892, #22802 ) ) ;
#10739 = CARTESIAN_POINT ( 'NONE',  ( 13.57481594606304576, 38.22187499999999716, -1.662435489736055892E-15 ) ) ;
#10740 = CARTESIAN_POINT ( 'NONE',  ( 9.295050272127047819, 36.08867187608392868, 9.295050272127046043 ) ) ;
#10741 = CARTESIAN_POINT ( 'NONE',  ( 103.5355339059327093, 3.535533905932755072, 2.750000002731185944 ) ) ;
#10742 = CARTESIAN_POINT ( 'NONE',  ( 135.4449143864723055, 37.03125000108393294, 13.14518615778179189 ) ) ;
#10743 = CARTESIAN_POINT ( 'NONE',  ( 59.55508561352770158, 34.35234375108392868, 13.14518615778179722 ) ) ;
#10744 = CARTESIAN_POINT ( 'NONE',  ( 204.2950502721270425, 38.66835937608393436, 9.295050272127046043 ) ) ;
#10745 =( BOUNDED_CURVE ( )  B_SPLINE_CURVE ( 2, ( #2822, #22781, #9792, #13769, #20639, #840, #3108, #24483, #17923, #18500, #26920 ),
 .UNSPECIFIED., .F., .F. ) 
 B_SPLINE_CURVE_WITH_KNOTS ( ( 3, 2, 2, 2, 2, 3 ),
 ( 0.6999999999999998446, 0.7199999999999998623, 0.7399999999999998801, 0.7600000000000000089, 0.7800000000000000266, 0.8000000000000000444 ),
 .UNSPECIFIED. ) 
 CURVE ( )  GEOMETRIC_REPRESENTATION_ITEM ( )  RATIONAL_B_SPLINE_CURVE ( ( 1.000000000000000222, 0.9510565162951533091, 1.000000000000000000, 0.9510565162951535312, 1.000000000000000000, 0.9510565162951535312, 1.000000000000000000, 0.9510565162951535312, 1.000000000000000000, 0.9510565162951535312, 1.000000000000000000 ) ) 
 REPRESENTATION_ITEM ( '' )  );
#10746 = CARTESIAN_POINT ( 'NONE',  ( 102.1631189606246295, 103.3426043859339103, -45.90000000546237402 ) ) ;
#10747 = CARTESIAN_POINT ( 'NONE',  ( -13.14518615778179544, 32.61601562608393579, 0.000000000000000000 ) ) ;
#10748 = CARTESIAN_POINT ( 'NONE',  ( 126.3635037532130951, 51.46815297078914142, -14.99999999999931077 ) ) ;
#10749 = AXIS2_PLACEMENT_3D ( 'NONE', #15529, #22249, #9265 ) ;
#10750 = CYLINDRICAL_SURFACE ( 'NONE', #7581, 4.999999999999989342 ) ;
#10751 = CARTESIAN_POINT ( 'NONE',  ( -9.295050272127044266, 34.50117187608393721, 9.295050272127047819 ) ) ;
#10752 = CARTESIAN_POINT ( 'NONE',  ( 106.5389055433251002, 114.7507929638356785, -51.92500000273119554 ) ) ;
#10753 = CARTESIAN_POINT ( 'NONE',  ( 9.295050272127046043, 37.87460937608393152, -9.295050272127046043 ) ) ;
#10754 = AXIS2_PLACEMENT_3D ( 'NONE', #20495, #1255, #7795 ) ;
#10755 = CARTESIAN_POINT ( 'NONE',  ( 99.99999999999995737, 85.00000000000000000, -1.387778780781445676E-14 ) ) ;
#10756 = CARTESIAN_POINT ( 'NONE',  ( 99.99999999999995737, -4.999999999999990230, 10.24999999999999822 ) ) ;
#10757 = CARTESIAN_POINT ( 'NONE',  ( 104.4587341249999781, -1.846868145590721655, 9.875000001365593860 ) ) ;
#10758 = EDGE_LOOP ( 'NONE', ( #7915, #10176, #16995, #9514 ) ) ;
#10759 = CARTESIAN_POINT ( 'NONE',  ( 101.0355339059327378, 124.0500000021849445, -2.499999999999997780 ) ) ;
#10760 = CARTESIAN_POINT ( 'NONE',  ( 101.8468681455906903, 4.458734125000016313, 12.12500000136559208 ) ) ;
#10761 = CARTESIAN_POINT ( 'NONE',  ( 125.0749732163386483, 49.99999999893126557, 12.67776588292038653 ) ) ;
#10762 = CARTESIAN_POINT ( 'NONE',  ( -13.14518615778179900, 40.50390625108394005, -5.444914386472297529 ) ) ;
#10763 = CARTESIAN_POINT ( 'NONE',  ( 116.4251840539369596, 38.71796875216787726, 0.000000000000000000 ) ) ;
#10764 = CARTESIAN_POINT ( 'NONE',  ( 99.99999999999995737, 80.93750000136559208, 4.458734124999988779 ) ) ;
#10765 = CARTESIAN_POINT ( 'NONE',  ( 74.29505027212704249, 34.69960937608393436, 9.295050272127046043 ) ) ;
#10766 = CARTESIAN_POINT ( 'NONE',  ( 108.0825317500000011, 107.3738262389971538, -50.22500000273118559 ) ) ;
#10767 = CARTESIAN_POINT ( 'NONE',  ( 9.295050272127046043, 39.46210937608393010, -9.295050272127046043 ) ) ;
#10768 = APPLICATION_CONTEXT ( 'automotive_design' ) ;
#10769 = CARTESIAN_POINT ( 'NONE',  ( -20.00000000000000355, 75.00000000000000000, -10.00000000000000000 ) ) ;
#10770 = CARTESIAN_POINT ( 'NONE',  ( 103.5355339059327093, -3.535533905932726206, 11.50000000273118417 ) ) ;
#10771 = CARTESIAN_POINT ( 'NONE',  ( 102.1631189606246153, 116.6573956140660897, -55.09999999453764019 ) ) ;
#10772 = CARTESIAN_POINT ( 'NONE',  ( 124.3771271284221314, 39.26367187499999289, -13.57481594606304753 ) ) ;
#10773 = ORIENTED_EDGE ( 'NONE', *, *, #18711, .T. ) ;
#10774 = CARTESIAN_POINT ( 'NONE',  ( 0.000000000000000000, 40.99999999999999289, 0.000000000000000000 ) ) ;
#10775 = CARTESIAN_POINT ( 'NONE',  ( 2.414731522848535132E-15, 36.98164062608393721, 13.14518615778179544 ) ) ;
#10776 = CARTESIAN_POINT ( 'NONE',  ( -9.598844408820458085, 36.23750000216787726, -9.598844408820458085 ) ) ;
#10777 = CARTESIAN_POINT ( 'NONE',  ( 120.7049497278729575, 35.09648437608392868, 9.295050272127047819 ) ) ;
#10778 = CARTESIAN_POINT ( 'NONE',  ( 59.37712712842213136, 33.80664062716786589, -13.57481594606304753 ) ) ;
#10779 = DIRECTION ( 'NONE',  ( 1.000000000000000000, -0.000000000000000000, -5.782411586589357392E-17 ) ) ;
#10780 = CARTESIAN_POINT ( 'NONE',  ( 13.57481594606304753, 36.78320312716786589, -5.622872871577873077 ) ) ;
#10781 = B_SPLINE_CURVE_WITH_KNOTS ( 'NONE', 3,
 ( #20176, #3212, #4932, #22605 ),
 .UNSPECIFIED., .F., .F.,
 ( 4, 4 ),
 ( 0.000000000000000000, 1.000000000000000000 ),
 .UNSPECIFIED. ) ;
#10782 = CARTESIAN_POINT ( 'NONE',  ( 96.46446609406721961, -3.535533905932727539, 7.124999999999999112 ) ) ;
#10783 = CARTESIAN_POINT ( 'NONE',  ( 95.67376207875072680, 115.9545556584642867, -46.80000000546237260 ) ) ;
#10784 = CARTESIAN_POINT ( 'NONE',  ( 181.8548138422181921, 39.01562500108393294, 5.444914386472304635 ) ) ;
#10785 = VECTOR ( 'NONE', #15773, 1000.000000000000000 ) ;
#10786 = CARTESIAN_POINT ( 'NONE',  ( -13.57481594606304753, 33.90585937716787868, -5.622872871577872189 ) ) ;
#10787 = FACE_OUTER_BOUND ( 'NONE', #10983, .T. ) ;
#10788 = CARTESIAN_POINT ( 'NONE',  ( 104.9999999999999716, 1.449011120738813565E-14, 4.625000002731185944 ) ) ;
#10789 = CARTESIAN_POINT ( 'NONE',  ( 97.93301270000000613, 124.6500000010924651, -9.540979117872439019E-15 ) ) ;
#10790 = CARTESIAN_POINT ( 'NONE',  ( 5.622872871577878406, 38.07304687499998863, 13.57481594606304576 ) ) ;
#10791 = CARTESIAN_POINT ( 'NONE',  ( 65.00000000000000000, 37.22968749999999716, 13.57481594606304576 ) ) ;
#10792 = CARTESIAN_POINT ( 'NONE',  ( 13.14518615778179900, 36.33671875108394289, 5.444914386472293977 ) ) ;
#10793 = CARTESIAN_POINT ( 'NONE',  ( -9.295050272127044266, 39.85898437608393152, 9.295050272127047819 ) ) ;
#10794 = CARTESIAN_POINT ( 'NONE',  ( 181.4251840539369596, 33.80664062500000000, -5.622872871577873077 ) ) ;
#10795 = CARTESIAN_POINT ( 'NONE',  ( 65.00000000000000000, 40.40468749999999432, 13.57481594606304576 ) ) ;
#10796 = DIRECTION ( 'NONE',  ( -0.000000000000000000, 1.000000000000000000, -0.000000000000000000 ) ) ;
#10797 = CARTESIAN_POINT ( 'NONE',  ( 74.29505027212704249, 39.26367187608393294, 9.295050272127046043 ) ) ;
#10798 = EDGE_CURVE ( 'NONE', #10159, #25944, #16576, .T. ) ;
#10799 = CARTESIAN_POINT ( 'NONE',  ( 96.84719886470459471, 3.152801135295383084, 1.312500001365592750 ) ) ;
#10800 = CARTESIAN_POINT ( 'NONE',  ( 7.171391131791534868, 31.93754143773660203, -11.52591762960188149 ) ) ;
#10801 = CARTESIAN_POINT ( 'NONE',  ( 95.54126587499999346, 91.74999999863439371, -1.846868145590737864 ) ) ;
#10802 = DIRECTION ( 'NONE',  ( -0.000000000000000000, 1.000000000000000000, -0.000000000000000000 ) ) ;
#10803 = CARTESIAN_POINT ( 'NONE',  ( 13.57481594606304576, 36.63437499999999858, -1.662435489736055892E-15 ) ) ;
#10804 = CARTESIAN_POINT ( 'NONE',  ( 65.00000000000000000, 36.93203125216787441, -13.57481594606304576 ) ) ;
#10805 = VERTEX_POINT ( 'NONE', #23419 ) ;
#10806 = CARTESIAN_POINT ( 'NONE',  ( 103.1528011352953342, 80.06250000136559208, 3.152801135295355106 ) ) ;
#10807 = CARTESIAN_POINT ( 'NONE',  ( 98.15313185440925281, 92.62499999863439371, -4.458734124999994997 ) ) ;
#10808 = ORIENTED_EDGE ( 'NONE', *, *, #9152, .T. ) ;
#10809 = CARTESIAN_POINT ( 'NONE',  ( 93.00000000000000000, 112.2744378736303332, -49.10000000000000853 ) ) ;
#10810 = CARTESIAN_POINT ( 'NONE',  ( 59.55508561352770158, 36.13828125108393863, 13.14518615778179722 ) ) ;
#10811 = ORIENTED_EDGE ( 'NONE', *, *, #4430, .T. ) ;
#10812 = CARTESIAN_POINT ( 'NONE',  ( 122.3834746745191921, 54.91574374957785665, -15.00000000000000000 ) ) ;
#10813 = CARTESIAN_POINT ( 'NONE',  ( 95.54126587499996504, 1.387778780781445676E-14, 2.687500001365592528 ) ) ;
#10814 = ORIENTED_EDGE ( 'NONE', *, *, #8099, .F. ) ;
#10815 = CARTESIAN_POINT ( 'NONE',  ( -9.295050272127044266, 35.29492187608393294, 9.295050272127047819 ) ) ;
#10816 = CARTESIAN_POINT ( 'NONE',  ( -5.444914386472297529, 31.67343750108393863, -13.14518615778179900 ) ) ;
#10817 = CARTESIAN_POINT ( 'NONE',  ( 208.5748159460630688, 37.52734375216787299, -1.662435489736055892E-15 ) ) ;
#10818 = CARTESIAN_POINT ( 'NONE',  ( -13.14518615778179544, 37.37851562608393863, 0.000000000000000000 ) ) ;
#10819 = LINE ( 'NONE', #6148, #25777 ) ;
#10820 = CARTESIAN_POINT ( 'NONE',  ( 195.8765262653620596, 51.45968077934941931, 14.99999999999961098 ) ) ;
#10821 = CARTESIAN_POINT ( 'NONE',  ( 208.5748159460630688, 39.95820312716787726, -5.622872871577873966 ) ) ;
#10822 = EDGE_LOOP ( 'NONE', ( #11460, #19662, #1217, #15670 ) ) ;
#10823 = CARTESIAN_POINT ( 'NONE',  ( -5.444914386472297529, 37.42812500108394147, -13.14518615778179900 ) ) ;
#10824 = CARTESIAN_POINT ( 'NONE',  ( 124.5550856135277087, 35.93984375108392726, 13.14518615778179722 ) ) ;
#10825 = CARTESIAN_POINT ( 'NONE',  ( 51.42518405393695957, 35.39414062499999147, -5.622872871577873077 ) ) ;
#10826 = LINE ( 'NONE', #12956, #12744 ) ;
#10827 = VECTOR ( 'NONE', #23764, 1000.000000000000000 ) ;
#10828 = CARTESIAN_POINT ( 'NONE',  ( 104.4587341249999639, 1.442382525525748735E-14, 10.18750000136559208 ) ) ;
#10829 = CARTESIAN_POINT ( 'NONE',  ( 95.67376207875072680, 115.9545556584642867, -46.30000000000001137 ) ) ;
#10830 = CARTESIAN_POINT ( 'NONE',  ( 95.54126587499996504, -1.846868145590724986, 13.50000000136559386 ) ) ;
#10831 = CARTESIAN_POINT ( 'NONE',  ( 97.50236033167492167, 102.3130555110000159, -50.72500000273119980 ) ) ;
#10832 = PRODUCT_DEFINITION_FORMATION_WITH_SPECIFIED_SOURCE ( 'ANY', '', #26282, .NOT_KNOWN. ) ;
#10833 = DIRECTION ( 'NONE',  ( 0.000000000000000000, 1.000000000000000000, 0.000000000000000000 ) ) ;
#10834 = CARTESIAN_POINT ( 'NONE',  ( 98.15313185440923860, 79.87500000136560629, 4.458734124999987891 ) ) ;
#10835 = CARTESIAN_POINT ( 'NONE',  ( 102.4976396683250783, 102.3130555110000159, -49.02499999726882152 ) ) ;
#10836 = CARTESIAN_POINT ( 'NONE',  ( 2.414731522848535132E-15, 36.18789062608393436, 13.14518615778179544 ) ) ;
#10837 = CARTESIAN_POINT ( 'NONE',  ( 106.5389055433250860, 105.2492070361643215, -49.07499999726882578 ) ) ;
#10838 = ORIENTED_EDGE ( 'NONE', *, *, #24988, .T. ) ;
#10839 = EDGE_CURVE ( 'NONE', #14819, #22694, #17739, .T. ) ;
#10840 = CARTESIAN_POINT ( 'NONE',  ( 97.93301270000000613, 123.9000000010924794, -0.8561741729129506151 ) ) ;
#10841 = CARTESIAN_POINT ( 'NONE',  ( 87.00000000000000000, 97.00000000000000000, -13.00000000000000533 ) ) ;
#10842 = CARTESIAN_POINT ( 'NONE',  ( 195.0000000000000000, 36.03906250000000000, -13.57481594606304576 ) ) ;
#10843 = CARTESIAN_POINT ( 'NONE',  ( 185.7049497278729575, 39.06523437608392868, 9.295050272127047819 ) ) ;
#10844 = ORIENTED_EDGE ( 'NONE', *, *, #15372, .F. ) ;
#10845 = CYLINDRICAL_SURFACE ( 'NONE', #14255, 13.57481594606304576 ) ;
#10846 = CYLINDRICAL_SURFACE ( 'NONE', #26191, 5.000000000000004441 ) ;
#10847 = AXIS2_PLACEMENT_3D ( 'NONE', #18314, #27023, #4927 ) ;
#10848 = CARTESIAN_POINT ( 'NONE',  ( 56.60778470836161347, 54.99999999999999289, -15.00000000000000178 ) ) ;
#10849 = VERTEX_POINT ( 'NONE', #25269 ) ;
#10850 = CARTESIAN_POINT ( 'NONE',  ( 99.99999999999998579, 117.3602355696678501, -52.50000000000000000 ) ) ;
#10851 = CARTESIAN_POINT ( 'NONE',  ( -9.295050272127046043, 40.45429687608393721, -9.295050272127046043 ) ) ;
#10852 = AXIS2_PLACEMENT_3D ( 'NONE', #13013, #6905, #21897 ) ;
#10853 = CARTESIAN_POINT ( 'NONE',  ( 99.99999999999995737, 81.37500000273119838, 4.999999999999990230 ) ) ;
#10854 = CARTESIAN_POINT ( 'NONE',  ( 120.4011555911795455, 32.26875000216787726, -9.598844408820458085 ) ) ;
#10855 = CARTESIAN_POINT ( 'NONE',  ( 65.00000000000000000, -7.395377635281828788, -7.517135062566165128E-15 ) ) ;
#10856 = ADVANCED_FACE ( 'NONE', ( #21006 ), #12420, .T. ) ;
#10857 = CARTESIAN_POINT ( 'NONE',  ( 102.0710678118654613, 93.68749999726881583, 4.999999999999983125 ) ) ;
#10858 = CARTESIAN_POINT ( 'NONE',  ( 51.85481384221819923, 39.90859375108394147, -5.444914386472297529 ) ) ;
#10859 = CARTESIAN_POINT ( 'NONE',  ( 13.57481594606304753, 37.47773437500001137, -5.622872871577873966 ) ) ;
#10860 = CARTESIAN_POINT ( 'NONE',  ( 204.2950502721270425, 36.28710937608393294, 9.295050272127046043 ) ) ;
#10861 = ORIENTED_EDGE ( 'NONE', *, *, #22564, .F. ) ;
#10862 = ORIENTED_EDGE ( 'NONE', *, *, #7944, .T. ) ;
#10863 = CARTESIAN_POINT ( 'NONE',  ( 5.444914386472297529, 39.71015625108393010, -13.14518615778179900 ) ) ;
#10864 = PRESENTATION_STYLE_ASSIGNMENT (( #6056 ) ) ;
#10865 = CARTESIAN_POINT ( 'NONE',  ( 104.4587341249999781, -1.846868145590721655, 12.12500000136559208 ) ) ;
#10866 =( BOUNDED_CURVE ( )  B_SPLINE_CURVE ( 2, ( #2424, #11084, #24354, #26360, #13506, #6818, #17372, #26068, #13358 ),
 .UNSPECIFIED., .F., .F. ) 
 B_SPLINE_CURVE_WITH_KNOTS ( ( 3, 2, 2, 2, 3 ),
 ( 0.7142857142857141906, 0.7232142857142855874, 0.7321428571428569843, 0.7410714285714286031, 0.7500000000000000000 ),
 .UNSPECIFIED. ) 
 CURVE ( )  GEOMETRIC_REPRESENTATION_ITEM ( )  RATIONAL_B_SPLINE_CURVE ( ( 1.000000000000000888, 0.9238795325112857393, 1.000000000000000000, 0.9238795325112867385, 1.000000000000000000, 0.9238795325112867385, 1.000000000000000000, 0.9238795325112867385, 1.000000000000000000 ) ) 
 REPRESENTATION_ITEM ( '' )  );
#10867 = EDGE_CURVE ( 'NONE', #11809, #25304, #1139, .T. ) ;
#10868 = CARTESIAN_POINT ( 'NONE',  ( 55.70494972787295751, 39.06523437608392868, 9.295050272127047819 ) ) ;
#10869 = CARTESIAN_POINT ( 'NONE',  ( 96.84719886470459471, 82.56250000136559208, 3.152801135295355994 ) ) ;
#10870 = CARTESIAN_POINT ( 'NONE',  ( 200.4449143864723055, 39.21406250108392300, 13.14518615778179189 ) ) ;
#10871 = CARTESIAN_POINT ( 'NONE',  ( 5.444914386472302859, 37.03125000108393294, 13.14518615778179189 ) ) ;
#10872 = CARTESIAN_POINT ( 'NONE',  ( -13.57481594606304753, 39.46210937716787726, -5.622872871577872189 ) ) ;
#10873 = AXIS2_PLACEMENT_3D ( 'NONE', #16209, #14483, #24912 ) ;
#10874 = CARTESIAN_POINT ( 'NONE',  ( 65.00000000000000000, 39.71015625216787015, 13.57481594606304576 ) ) ;
#10875 = VECTOR ( 'NONE', #13889, 1000.000000000000000 ) ;
#10876 = CARTESIAN_POINT ( 'NONE',  ( 92.99999999999997158, 107.7255621263696952, -49.89999999999999858 ) ) ;
#10877 = CARTESIAN_POINT ( 'NONE',  ( 99.99999999999997158, 118.4984768113314004, -50.12499999726881583 ) ) ;
#10878 = EDGE_CURVE ( 'NONE', #12008, #26730, #20728, .T. ) ;
#10879 = EDGE_LOOP ( 'NONE', ( #23994, #9748, #25111, #1727, #25426, #9874, #18552, #641 ) ) ;
#10880 = CARTESIAN_POINT ( 'NONE',  ( 5.622872871577878406, 38.07304687499998863, 13.57481594606304576 ) ) ;
#10881 = CARTESIAN_POINT ( 'NONE',  ( -9.295050272127046043, 38.07304687608393579, -9.295050272127046043 ) ) ;
#10882 = CARTESIAN_POINT ( 'NONE',  ( 104.9999999999999574, 2.071067811865491937, 1.687500002731185056 ) ) ;
#10883 = CARTESIAN_POINT ( 'NONE',  ( 120.7049497278729575, 35.09648437608393579, -9.295050272127046043 ) ) ;
#10884 = CARTESIAN_POINT ( 'NONE',  ( 51.85481384221819923, 34.94765625108392726, -5.444914386472297529 ) ) ;
#10885 = EDGE_CURVE ( 'NONE', #12248, #15376, #7746, .T. ) ;
#10886 = CARTESIAN_POINT ( 'NONE',  ( 208.1451861577817795, 36.43593750108392726, -5.444914386472297529 ) ) ;
#10887 = CARTESIAN_POINT ( 'NONE',  ( 99.99999999999998579, 102.6397644303321215, -46.00000000546238255 ) ) ;
#10888 = SURFACE_STYLE_USAGE ( .BOTH. , #2224 ) ;
#10889 = CARTESIAN_POINT ( 'NONE',  ( 127.9753722744671194, 50.00000000050989968, -13.43320860980974807 ) ) ;
#10890 = DIRECTION ( 'NONE',  ( -0.000000000000000000, -0.000000000000000000, -1.000000000000000000 ) ) ;
#10891 = CARTESIAN_POINT ( 'NONE',  ( 143.5748159460630404, 39.95820312716787726, -5.622872871577873077 ) ) ;
#10892 = CARTESIAN_POINT ( 'NONE',  ( 93.46109445667491400, 114.7507929638356785, -53.32500000273119412 ) ) ;
#10893 = CARTESIAN_POINT ( 'NONE',  ( 9.295050272127046043, 33.90585937608393152, -9.295050272127046043 ) ) ;
#10894 = CARTESIAN_POINT ( 'NONE',  ( 9.180175813647995398, 50.00000000000000000, 9.999999999999994671 ) ) ;
#10895 = CARTESIAN_POINT ( 'NONE',  ( 98.96446609406727646, 123.6500000021849530, 2.499999999999977796 ) ) ;
#10896 = CARTESIAN_POINT ( 'NONE',  ( 96.46446609406721961, -3.535533905932727539, 10.12499999999999822 ) ) ;
#10897 = CARTESIAN_POINT ( 'NONE',  ( 107.0000000000000142, 110.0000000000000000, -47.00000000000000711 ) ) ;
#10898 = CARTESIAN_POINT ( 'NONE',  ( 95.54126587499996504, 1.387778780781445676E-14, 9.437500001365593860 ) ) ;
#10899 = VERTEX_POINT ( 'NONE', #21138 ) ;
#10900 = CARTESIAN_POINT ( 'NONE',  ( 99.99999999999998579, 122.7500000010924879, -2.066987299999998751 ) ) ;
#10901 = CARTESIAN_POINT ( 'NONE',  ( 104.4587341249999781, -1.846868145590721655, 10.87500000136559386 ) ) ;
#10902 = LINE ( 'NONE', #6915, #8662 ) ;
#10903 = CARTESIAN_POINT ( 'NONE',  ( 13.14518615778179900, 39.31328125108392868, 5.444914386472293977 ) ) ;
#10904 = CYLINDRICAL_SURFACE ( 'NONE', #10364, 13.57481594606304398 ) ;
#10905 = CARTESIAN_POINT ( 'NONE',  ( 99.99999999999995737, 81.93750000136559208, 4.458734124999988779 ) ) ;
#10906 = CARTESIAN_POINT ( 'NONE',  ( 59.55508561352770158, 34.25312500108393010, -13.14518615778179900 ) ) ;
#10907 = CARTESIAN_POINT ( 'NONE',  ( 95.00472066334982912, 116.8754121666685393, -51.42500000273118843 ) ) ;
#10908 = FACE_OUTER_BOUND ( 'NONE', #2512, .T. ) ;
#10909 = CARTESIAN_POINT ( 'NONE',  ( -15.00000000000000355, 75.00000000000000000, -9.999999999999998224 ) ) ;
#10910 = DIRECTION ( 'NONE',  ( 0.000000000000000000, 0.000000000000000000, 1.000000000000000000 ) ) ;
#10911 = DIRECTION ( 'NONE',  ( -0.000000000000000000, -1.000000000000000000, -0.000000000000000000 ) ) ;
#10912 = CARTESIAN_POINT ( 'NONE',  ( 130.0000000000000000, 38.02343749999999289, 13.57481594606304576 ) ) ;
#10913 = EDGE_CURVE ( 'NONE', #12008, #3132, #2036, .T. ) ;
#10914 = VERTEX_POINT ( 'NONE', #18722 ) ;
#10915 = LINE ( 'NONE', #4105, #1750 ) ;
#10916 =( BOUNDED_SURFACE ( )  B_SPLINE_SURFACE ( 1, 2, ( 
 ( #23080, #16922, #1838, #25622, #3827, #8096, #25489, #5967, #17200, #6104, #21357, #10501, #14771, #19208, #25760, #6242, #4107, #3555, #12212, #20941, #10082, #18794, #27501, #7956, #16655, #5834, #14502, #23219, #17345, #4811, #13470, #21922, #22196, #23905, #21633, #26622, #2397, #15625, #2675, #4385, #13183, #6647, #8934, #13042, #17911, #23767, #20057, #11336, #536, #8791, #19488, #2531, #6512, #11055, #24327, #9218, #21777, #17482, #24190, #8654, #248, #2256, #395, #9077, #26041, #24049, #17772, #15187, #4524, #19764, #28186, #26476, #15049, #10918, #11193, #6932, #19627, #4243, #19912, #15333, #12903, #2109, #10776, #109, #26181, #17623, #26330, #6790, #15475, #4669, #13331, #22057, #1110, #22340, #22625, #22904, #9777, #5378, #25037, #11901, #18195, #5519, #2810, #828, #18623, #15764, #26762, #16043, #5094, #11616, #7069, #18485, #20487, #9637, #26906, #3096, #3367, #7644, #27193, #968, #24471, #4956, #14186, #20196, #16337, #24897, #11479, #14047, #681, #24616, #9356, #12038, #20625, #24753, #5234, #22481, #13617, #18049, #7204, #9495, #20762, #1246, #7352, #15899, #9909, #13756, #2946, #20341, #18342, #13900, #11763, #27047, #7495, #16191, #22768, #3233, #1523, #5656, #5931, #16885, #27327, #1386, #25451, #10462, #14462, #10604, #7786, #14599, #3790, #25308, #27461, #19170, #6204, #10175, #17018, #23317, #27735, #20904, #14321, #14874, #12448, #27871, #7919 ),
 ( #16615, #21175, #18885, #1655, #5796, #1935, #16473, #4071, #23589, #12733, #21039, #3513, #14733, #18758, #10314, #8334, #25721, #23181, #27594, #8195, #10047, #19022, #3655, #12589, #21313, #12318, #8055, #1797, #16750, #25584, #6067, #12174, #21457, #25168, #23453, #3931, #23042, #12865, #11155, #6754, #19590, #13288, #22017, #17735, #15150, #356, #4772, #23868, #19727, #212, #10881, #24012, #24153, #73, #4630, #8754, #26004, #8897, #26145, #24291, #15295, #4346, #6896, #8616, #19871, #22160, #21595, #9043, #26437, #6610, #15583, #28149, #25866, #2638, #4490, #13432, #19311, #17304, #17446, #13147, #21884, #6475, #28011, #8476, #17165, #6337, #15011, #13002, #23732, #15438, #10740, #2359, #4206, #2070, #21741, #2217, #17587, #19450, #11014, #26292, #2494, #24860, #22303, #20302, #5341, #4919, #788, #26872, #15727, #14007, #20590, #13580, #27012, #22730, #2778, #3197, #7459, #11582, #11868, #1073, #9742, #7170, #18451, #25001, #15867, #16154, #24431, #17875, #2912, #9182, #27157, #26581, #7318, #7610, #16300, #9603, #5481, #14151, #22445, #22870, #7030, #5059, #11300, #20021, #11442, #9458, #20162, #18160, #501, #644, #9317, #18014, #26725, #24577, #13723, #16007, #24721, #5199, #13864, #22589, #3058, #11724, #18304, #20450, #932, #7886, #12284, #23007, #18725, #12143, #14290, #27293, #25134, #7750, #14431, #23147, #16581, #27423, #5761, #25273, #5624, #3622, #20732 ) ),
 .UNSPECIFIED., .F., .F., .F. ) 
 B_SPLINE_SURFACE_WITH_KNOTS ( ( 2, 2 ),
 ( 3, 2, 2, 2, 2, 2, 2, 2, 2, 2, 2, 2, 2, 2, 2, 2, 2, 2, 2, 2, 2, 2, 2, 2, 2, 2, 2, 2, 2, 2, 2, 2, 2, 2, 2, 2, 2, 2, 2, 2, 2, 2, 2, 2, 2, 2, 2, 2, 2, 2, 2, 2, 2, 2, 2, 2, 2, 2, 2, 2, 2, 2, 2, 2, 2, 2, 2, 2, 2, 2, 2, 2, 2, 2, 2, 2, 2, 2, 2, 2, 2, 2, 2, 2, 2, 2, 2, 2, 2, 2, 2, 3 ),
 ( 0.000000000000000000, 1.000000000000000000 ),
 ( 0.000000000000000000, 0.01041666666666666609, 0.02083333333333333218, 0.03125000000000000000, 0.04166666666666666435, 0.05208333333333333565, 0.06250000000000000000, 0.07291666666666667129, 0.08333333333333332871, 0.09375000000000000000, 0.1041666666666666713, 0.1145833333333333287, 0.1250000000000000000, 0.1354166666666666574, 0.1458333333333333426, 0.1562500000000000000, 0.1666666666666666574, 0.1770833333333333426, 0.1875000000000000000, 0.1979166666666666574, 0.2083333333333333426, 0.2187500000000000000, 0.2291666666666666574, 0.2395833333333333426, 0.2500000000000000000, 0.2604166666666666852, 0.2708333333333333148, 0.2812500000000000000, 0.2916666666666666852, 0.3020833333333333148, 0.3125000000000000000, 0.3229166666666666852, 0.3333333333333333148, 0.3437500000000000000, 0.3541666666666666852, 0.3645833333333333148, 0.3750000000000000000, 0.3854166666666666852, 0.3958333333333333148, 0.4062500000000000000, 0.4166666666666666852, 0.4270833333333333148, 0.4375000000000000000, 0.4479166666666666852, 0.4583333333333333148, 0.4687500000000000000, 0.4791666666666666852, 0.4895833333333333148, 0.5000000000000000000, 0.5104166666666666297, 0.5208333333333333703, 0.5312500000000000000, 0.5416666666666666297, 0.5520833333333333703, 0.5625000000000000000, 0.5729166666666666297, 0.5833333333333333703, 0.5937500000000000000, 0.6041666666666666297, 0.6145833333333333703, 0.6250000000000000000, 0.6354166666666666297, 0.6458333333333333703, 0.6562500000000000000, 0.6666666666666666297, 0.6770833333333333703, 0.6875000000000000000, 0.6979166666666666297, 0.7083333333333333703, 0.7187500000000000000, 0.7291666666666666297, 0.7395833333333333703, 0.7500000000000000000, 0.7604166666666666297, 0.7708333333333333703, 0.7812500000000000000, 0.7916666666666666297, 0.8020833333333333703, 0.8125000000000000000, 0.8229166666666666297, 0.8333333333333333703, 0.8437500000000000000, 0.8541666666666666297, 0.8645833333333333703, 0.8750000000000000000, 0.8854166666666666297, 0.8958333333333333703, 0.9062500000000000000, 0.9166666666666666297, 0.9270833333333333703, 0.9375000000000000000, 0.9448586970929392370 ),
 .UNSPECIFIED. ) 
 GEOMETRIC_REPRESENTATION_ITEM ( )  RATIONAL_B_SPLINE_SURFACE ( (
 ( 1.000000000000000000, 0.9238795325112867385, 1.000000000000000000, 0.9238795325112867385, 1.000000000000000000, 0.9238795325112867385, 1.000000000000000000, 0.9238795325112867385, 1.000000000000000000, 0.9238795325112867385, 1.000000000000000000, 0.9238795325112867385, 1.000000000000000000, 0.9238795325112867385, 1.000000000000000000, 0.9238795325112867385, 1.000000000000000000, 0.9238795325112867385, 1.000000000000000000, 0.9238795325112867385, 1.000000000000000000, 0.9238795325112867385, 1.000000000000000000, 0.9238795325112867385, 1.000000000000000000, 0.9238795325112867385, 1.000000000000000000, 0.9238795325112867385, 1.000000000000000000, 0.9238795325112867385, 1.000000000000000000, 0.9238795325112867385, 1.000000000000000000, 0.9238795325112867385, 1.000000000000000000, 0.9238795325112867385, 1.000000000000000000, 0.9238795325112867385, 1.000000000000000000, 0.9238795325112867385, 1.000000000000000000, 0.9238795325112867385, 1.000000000000000000, 0.9238795325112867385, 1.000000000000000000, 0.9238795325112867385, 1.000000000000000000, 0.9238795325112867385, 1.000000000000000000, 0.9238795325112867385, 1.000000000000000000, 0.9238795325112867385, 1.000000000000000000, 0.9238795325112867385, 1.000000000000000000, 0.9238795325112867385, 1.000000000000000000, 0.9238795325112867385, 1.000000000000000000, 0.9238795325112867385, 1.000000000000000000, 0.9238795325112867385, 1.000000000000000000, 0.9238795325112867385, 1.000000000000000000, 0.9238795325112867385, 1.000000000000000000, 0.9238795325112867385, 1.000000000000000000, 0.9238795325112867385, 1.000000000000000000, 0.9238795325112867385, 1.000000000000000000, 0.9238795325112867385, 1.000000000000000000, 0.9238795325112867385, 1.000000000000000000, 0.9238795325112867385, 1.000000000000000000, 0.9238795325112867385, 1.000000000000000000, 0.9238795325112867385, 1.000000000000000000, 0.9238795325112867385, 1.000000000000000000, 0.9238795325112867385, 1.000000000000000000, 0.9238795325112867385, 1.000000000000000000, 0.9238795325112867385, 1.000000000000000000, 0.9238795325112867385, 1.000000000000000000, 0.9238795325112867385, 1.000000000000000000, 0.9238795325112867385, 1.000000000000000000, 0.9238795325112867385, 1.000000000000000000, 0.9238795325112867385, 1.000000000000000000, 0.9238795325112867385, 1.000000000000000000, 0.9238795325112867385, 1.000000000000000000, 0.9238795325112867385, 1.000000000000000000, 0.9238795325112867385, 1.000000000000000000, 0.9238795325112867385, 1.000000000000000000, 0.9238795325112867385, 1.000000000000000000, 0.9238795325112867385, 1.000000000000000000, 0.9238795325112867385, 1.000000000000000000, 0.9238795325112867385, 1.000000000000000000, 0.9238795325112867385, 1.000000000000000000, 0.9238795325112867385, 1.000000000000000000, 0.9238795325112867385, 1.000000000000000000, 0.9238795325112867385, 1.000000000000000000, 0.9238795325112867385, 1.000000000000000000, 0.9238795325112867385, 1.000000000000000000, 0.9238795325112867385, 1.000000000000000000, 0.9238795325112867385, 1.000000000000000000, 0.9238795325112867385, 1.000000000000000000, 0.9238795325112867385, 1.000000000000000000, 0.9238795325112867385, 1.000000000000000000, 0.9238795325112867385, 1.000000000000000000, 0.9238795325112867385, 1.000000000000000000, 0.9238795325112867385, 1.000000000000000000, 0.9238795325112867385, 1.000000000000000000, 0.9238795325112867385, 1.000000000000000000, 0.9238795325112867385, 1.000000000000000000, 0.9238795325112867385, 1.000000000000000000, 0.9238795325112867385, 1.000000000000000000, 0.9238795325112867385, 1.000000000000000000, 0.9238795325112867385, 1.000000000000000000, 0.9238795325112867385, 1.000000000000000000, 0.9238795325112867385, 1.000000000000000000, 0.9238795325112867385, 1.000000000000000000, 0.9238795325112867385, 1.000000000000000000, 0.9238795325112867385, 1.000000000000000000, 0.9238795325112867385, 1.000000000000000000, 0.9238795325112867385, 1.000000000000000000, 0.9238795325112867385, 1.000000000000000000, 0.9238795325112867385, 1.000000000000000000, 0.9238795325112867385, 1.000000000000000000, 0.9462258435690522607, 0.9684275710300105366),
 ( 1.000000000000000000, 0.9238795325112867385, 1.000000000000000000, 0.9238795325112867385, 1.000000000000000000, 0.9238795325112867385, 1.000000000000000000, 0.9238795325112867385, 1.000000000000000000, 0.9238795325112867385, 1.000000000000000000, 0.9238795325112867385, 1.000000000000000000, 0.9238795325112867385, 1.000000000000000000, 0.9238795325112867385, 1.000000000000000000, 0.9238795325112867385, 1.000000000000000000, 0.9238795325112867385, 1.000000000000000000, 0.9238795325112867385, 1.000000000000000000, 0.9238795325112867385, 1.000000000000000000, 0.9238795325112867385, 1.000000000000000000, 0.9238795325112867385, 1.000000000000000000, 0.9238795325112867385, 1.000000000000000000, 0.9238795325112867385, 1.000000000000000000, 0.9238795325112867385, 1.000000000000000000, 0.9238795325112867385, 1.000000000000000000, 0.9238795325112867385, 1.000000000000000000, 0.9238795325112867385, 1.000000000000000000, 0.9238795325112867385, 1.000000000000000000, 0.9238795325112867385, 1.000000000000000000, 0.9238795325112867385, 1.000000000000000000, 0.9238795325112867385, 1.000000000000000000, 0.9238795325112867385, 1.000000000000000000, 0.9238795325112867385, 1.000000000000000000, 0.9238795325112867385, 1.000000000000000000, 0.9238795325112867385, 1.000000000000000000, 0.9238795325112867385, 1.000000000000000000, 0.9238795325112867385, 1.000000000000000000, 0.9238795325112867385, 1.000000000000000000, 0.9238795325112867385, 1.000000000000000000, 0.9238795325112867385, 1.000000000000000000, 0.9238795325112867385, 1.000000000000000000, 0.9238795325112867385, 1.000000000000000000, 0.9238795325112867385, 1.000000000000000000, 0.9238795325112867385, 1.000000000000000000, 0.9238795325112867385, 1.000000000000000000, 0.9238795325112867385, 1.000000000000000000, 0.9238795325112867385, 1.000000000000000000, 0.9238795325112867385, 1.000000000000000000, 0.9238795325112867385, 1.000000000000000000, 0.9238795325112867385, 1.000000000000000000, 0.9238795325112867385, 1.000000000000000000, 0.9238795325112867385, 1.000000000000000000, 0.9238795325112867385, 1.000000000000000000, 0.9238795325112867385, 1.000000000000000000, 0.9238795325112867385, 1.000000000000000000, 0.9238795325112867385, 1.000000000000000000, 0.9238795325112867385, 1.000000000000000000, 0.9238795325112867385, 1.000000000000000000, 0.9238795325112867385, 1.000000000000000000, 0.9238795325112867385, 1.000000000000000000, 0.9238795325112867385, 1.000000000000000000, 0.9238795325112867385, 1.000000000000000000, 0.9238795325112867385, 1.000000000000000000, 0.9238795325112867385, 1.000000000000000000, 0.9238795325112867385, 1.000000000000000000, 0.9238795325112867385, 1.000000000000000000, 0.9238795325112867385, 1.000000000000000000, 0.9238795325112867385, 1.000000000000000000, 0.9238795325112867385, 1.000000000000000000, 0.9238795325112867385, 1.000000000000000000, 0.9238795325112867385, 1.000000000000000000, 0.9238795325112867385, 1.000000000000000000, 0.9238795325112867385, 1.000000000000000000, 0.9238795325112867385, 1.000000000000000000, 0.9238795325112867385, 1.000000000000000000, 0.9238795325112867385, 1.000000000000000000, 0.9238795325112867385, 1.000000000000000000, 0.9238795325112867385, 1.000000000000000000, 0.9238795325112867385, 1.000000000000000000, 0.9238795325112867385, 1.000000000000000000, 0.9238795325112867385, 1.000000000000000000, 0.9238795325112867385, 1.000000000000000000, 0.9238795325112867385, 1.000000000000000000, 0.9238795325112867385, 1.000000000000000000, 0.9238795325112867385, 1.000000000000000000, 0.9238795325112867385, 1.000000000000000000, 0.9238795325112867385, 1.000000000000000000, 0.9238795325112867385, 1.000000000000000000, 0.9238795325112867385, 1.000000000000000000, 0.9238795325112867385, 1.000000000000000000, 0.9238795325112867385, 1.000000000000000000, 0.9238795325112867385, 1.000000000000000000, 0.9238795325112867385, 1.000000000000000000, 0.9238795325112867385, 1.000000000000000000, 0.9238795325112867385, 1.000000000000000000, 0.9238795325112867385, 1.000000000000000000, 0.9238795325112867385, 1.000000000000000000, 0.9462258435690522607, 0.9684275710300105366) ) ) 
 REPRESENTATION_ITEM ( '' )  SURFACE ( )  );
#10917 = CARTESIAN_POINT ( 'NONE',  ( -8.049105076161786076E-16, 37.37851562608393863, -13.14518615778179544 ) ) ;
#10918 = CARTESIAN_POINT ( 'NONE',  ( 13.57481594606304931, 36.68398437716788152, 5.622872871577869525 ) ) ;
#10919 = CARTESIAN_POINT ( 'NONE',  ( 116.8548138422182063, 35.74140625108393721, -5.444914386472297529 ) ) ;
#10920 = CARTESIAN_POINT ( 'NONE',  ( 74.59884440882045453, 35.24531250216787726, -9.598844408820458085 ) ) ;
#10921 = AXIS2_PLACEMENT_3D ( 'NONE', #10597, #21166, #27728 ) ;
#10922 = CARTESIAN_POINT ( 'NONE',  ( 6.351932228772031230, 36.00000000000000000, 11.61660627739472140 ) ) ;
#10923 = CARTESIAN_POINT ( 'NONE',  ( -13.14518615778179544, 40.55351562608393579, 0.000000000000000000 ) ) ;
#10924 = CARTESIAN_POINT ( 'NONE',  ( 96.46446609406721961, -3.535533905932727539, 6.124999999999998224 ) ) ;
#10925 = CARTESIAN_POINT ( 'NONE',  ( 106.5389055433250860, 105.2492070361643215, -49.07499999726882578 ) ) ;
#10926 = CARTESIAN_POINT ( 'NONE',  ( 200.4449143864723055, 33.95546875108393436, -13.14518615778179900 ) ) ;
#10927 = DIRECTION ( 'NONE',  ( 0.000000000000000000, 0.000000000000000000, -1.000000000000000000 ) ) ;
#10928 = CARTESIAN_POINT ( 'NONE',  ( 98.23223304703363112, 122.6000000021849559, -1.767766952966370209 ) ) ;
#10929 = DIRECTION ( 'NONE',  ( 0.000000000000000000, -1.000000000000000000, 0.000000000000000000 ) ) ;
#10930 = CARTESIAN_POINT ( 'NONE',  ( 195.0000000000000000, 39.31328125216787583, -13.57481594606304576 ) ) ;
#10931 = CARTESIAN_POINT ( 'NONE',  ( 13.57481594606304931, 36.58476562499999574, 5.622872871577869525 ) ) ;
#10932 = CARTESIAN_POINT ( 'NONE',  ( 107.0000000000000142, 110.0000000000000000, -53.50000000546238255 ) ) ;
#10933 = CARTESIAN_POINT ( 'NONE',  ( -13.14518615778179189, 37.62656250108393863, 5.444914386472304635 ) ) ;
#10934 = CARTESIAN_POINT ( 'NONE',  ( 9.295050272127046043, 39.46210937608393010, -9.295050272127046043 ) ) ;
#10935 = CARTESIAN_POINT ( 'NONE',  ( 208.5748159460630688, 35.84062499999999574, -1.662435489736055892E-15 ) ) ;
#10936 = CARTESIAN_POINT ( 'NONE',  ( 106.5389055433251002, 105.2492070361643215, -46.57500000273119412 ) ) ;
#10937 = CARTESIAN_POINT ( 'NONE',  ( 74.29505027212704249, 37.08085937608393579, -9.295050272127046043 ) ) ;
#10938 = CARTESIAN_POINT ( 'NONE',  ( 104.4587341249999781, 1.846868145590750521, 3.000000001365592528 ) ) ;
#10939 = CARTESIAN_POINT ( 'NONE',  ( 93.00000000000000000, 110.0000000000000000, -44.50000000546237544 ) ) ;
#10940 = CARTESIAN_POINT ( 'NONE',  ( 96.84719886470463734, 93.68749999863440792, -3.152801135295366208 ) ) ;
#10941 = CARTESIAN_POINT ( 'NONE',  ( 98.72729855789484077, 123.0000000000000568, -1.650814227560484460 ) ) ;
#10942 = CARTESIAN_POINT ( 'NONE',  ( 13.57481594606304576, 35.04687499999999289, -1.662435489736055892E-15 ) ) ;
#10943 = CARTESIAN_POINT ( 'NONE',  ( 116.8548138422182205, 37.57695312608393579, 0.000000000000000000 ) ) ;
#10944 = ORIENTED_EDGE ( 'NONE', *, *, #4304, .F. ) ;
#10945 = ORIENTED_EDGE ( 'NONE', *, *, #3383, .T. ) ;
#10946 = CARTESIAN_POINT ( 'NONE',  ( 96.46446609406721961, 82.87500000000000000, -3.535533905932755072 ) ) ;
#10947 = CONICAL_SURFACE ( 'NONE', #6801, 11.50000000000001776, 0.7853981633974473908 ) ;
#10948 = CARTESIAN_POINT ( 'NONE',  ( 102.0710678118654329, 82.81250000273119838, -5.000000000000018652 ) ) ;
#10949 = CARTESIAN_POINT ( 'NONE',  ( 95.54126587500000767, 93.81249999863440792, -7.484931351350258973E-15 ) ) ;
#10950 = CARTESIAN_POINT ( 'NONE',  ( 57.60596795766428357, 36.00000000000002842, -11.20317769887112647 ) ) ;
#10951 = ORIENTED_EDGE ( 'NONE', *, *, #3170, .F. ) ;
#10952 = CARTESIAN_POINT ( 'NONE',  ( 105.6631189606246295, 105.8855032339526758, -52.20000000000000995 ) ) ;
#10953 = CARTESIAN_POINT ( 'NONE',  ( 74.29505027212704249, 35.69179687608394147, -9.295050272127046043 ) ) ;
#10954 = ORIENTED_EDGE ( 'NONE', *, *, #20222, .T. ) ;
#10955 = AXIS2_PLACEMENT_3D ( 'NONE', #7224, #15489, #21932 ) ;
#10956 = CARTESIAN_POINT ( 'NONE',  ( 99.99999999999995737, 4.458734125000016313, 2.437500001365592084 ) ) ;
#10957 = EDGE_CURVE ( 'NONE', #24722, #11653, #19565, .T. ) ;
#10958 = ORIENTED_EDGE ( 'NONE', *, *, #21043, .T. ) ;
#10959 = CARTESIAN_POINT ( 'NONE',  ( 96.46446609406721961, 82.00000000273119838, -3.535533905932755072 ) ) ;
#10960 = CARTESIAN_POINT ( 'NONE',  ( -9.295050272127044266, 39.26367187608393294, 9.295050272127047819 ) ) ;
#10961 = CARTESIAN_POINT ( 'NONE',  ( 181.4251840539369596, 37.87460937716787868, -5.622872871577873077 ) ) ;
#10962 = CARTESIAN_POINT ( 'NONE',  ( 2.414731522848535132E-15, 36.78320312608393294, 13.14518615778179544 ) ) ;
#10963 = LINE ( 'NONE', #19674, #23071 ) ;
#10964 = CARTESIAN_POINT ( 'NONE',  ( 120.7049497278729575, 36.88242187608393152, 9.295050272127047819 ) ) ;
#10965 = CARTESIAN_POINT ( 'NONE',  ( -9.295050272127044266, 39.26367187608393294, 9.295050272127047819 ) ) ;
#10966 = CARTESIAN_POINT ( 'NONE',  ( 124.5550856135277087, 36.43593750108392726, -13.14518615778179900 ) ) ;
#10967 = CARTESIAN_POINT ( 'NONE',  ( 70.62287287157786864, 35.98945312499999716, -13.57481594606304753 ) ) ;
#10968 = DIRECTION ( 'NONE',  ( 0.000000000000000000, 0.000000000000000000, -1.000000000000000000 ) ) ;
#10969 = CARTESIAN_POINT ( 'NONE',  ( 101.8468681455906903, 4.458734125000016313, 11.37500000136559386 ) ) ;
#10970 = CARTESIAN_POINT ( 'NONE',  ( 207.8921516136353773, 35.99999999999997868, -4.169510824908014612 ) ) ;
#10971 = CARTESIAN_POINT ( 'NONE',  ( 95.54126587499996504, -1.846868145590724986, 12.50000000136559208 ) ) ;
#10972 = CARTESIAN_POINT ( 'NONE',  ( 91.91746824999998466, 107.3738262389971538, -53.02500000273119696 ) ) ;
#10973 = CARTESIAN_POINT ( 'NONE',  ( 9.598844408820456309, 39.21406250216787015, -9.598844408820458085 ) ) ;
#10974 = FACE_OUTER_BOUND ( 'NONE', #20949, .T. ) ;
#10975 = CARTESIAN_POINT ( 'NONE',  ( 97.50236033167490746, 117.6869444889999841, -52.02499999726882862 ) ) ;
#10976 = CARTESIAN_POINT ( 'NONE',  ( 9.295050272127046043, 35.69179687608394147, -9.295050272127046043 ) ) ;
#10977 = CARTESIAN_POINT ( 'NONE',  ( 95.00472066334982912, 116.8754121666685393, -50.17499999726882010 ) ) ;
#10978 = VERTEX_POINT ( 'NONE', #1486 ) ;
#10979 = CARTESIAN_POINT ( 'NONE',  ( 99.99999999999998579, 124.1500000010924651, 2.066987299999980099 ) ) ;
#10980 = DIRECTION ( 'NONE',  ( 0.000000000000000000, 0.000000000000000000, 1.000000000000000000 ) ) ;
#10981 = CARTESIAN_POINT ( 'NONE',  ( 99.99999999999998579, 90.25000000000000000, -4.999999999999997335 ) ) ;
#10982 = CARTESIAN_POINT ( 'NONE',  ( 181.8548138422181921, 37.42812500108393436, 5.444914386472304635 ) ) ;
#10983 = EDGE_LOOP ( 'NONE', ( #17146, #14669, #18388, #24357 ) ) ;
#10984 = CARTESIAN_POINT ( 'NONE',  ( 2.385244779468109360E-15, 80.00000000000000000, 9.999999999999996447 ) ) ;
#10985 = CARTESIAN_POINT ( 'NONE',  ( 2.493653234604083739E-15, 39.71015625216787015, 13.57481594606304576 ) ) ;
#10986 = CARTESIAN_POINT ( 'NONE',  ( 63.49898087569502536, 53.60014735326987534, -15.00000000000000000 ) ) ;
#10987 = EDGE_CURVE ( 'NONE', #3669, #6267, #12713, .T. ) ;
#10988 = ORIENTED_EDGE ( 'NONE', *, *, #21874, .T. ) ;
#10989 = CARTESIAN_POINT ( 'NONE',  ( 99.99999999999998579, 102.6397644303321215, -51.50000000000000711 ) ) ;
#10990 = CARTESIAN_POINT ( 'NONE',  ( 9.295050272127046043, 39.46210937608393010, -9.295050272127046043 ) ) ;
#10991 = CARTESIAN_POINT ( 'NONE',  ( 96.46446609406721961, 81.00000000273119838, -3.535533905932755072 ) ) ;
#10992 = CARTESIAN_POINT ( 'NONE',  ( 116.4251840539369596, 32.36796875216787583, 0.000000000000000000 ) ) ;
#10993 = CARTESIAN_POINT ( 'NONE',  ( 13.14518615778179722, 40.40468750108393436, -5.444914386472297529 ) ) ;
#10994 = CARTESIAN_POINT ( 'NONE',  ( 103.5355339059327235, 91.99999999726880162, -3.535533905932738197 ) ) ;
#10995 = CARTESIAN_POINT ( 'NONE',  ( 51.85481384221819923, 38.32109375108394289, -5.444914386472297529 ) ) ;
#10996 = CARTESIAN_POINT ( 'NONE',  ( -13.57481594606304576, 34.74921875216787726, 0.000000000000000000 ) ) ;
#10997 = CARTESIAN_POINT ( 'NONE',  ( 189.5550856135277229, 34.55078125108393294, 13.14518615778179722 ) ) ;
#10998 = EDGE_LOOP ( 'NONE', ( #6419, #6770, #25486, #5631 ) ) ;
#10999 = ORIENTED_EDGE ( 'NONE', *, *, #24239, .F. ) ;
#11000 = ORIENTED_EDGE ( 'NONE', *, *, #19768, .F. ) ;
#11001 = CARTESIAN_POINT ( 'NONE',  ( -13.14518615778179189, 37.62656250108393863, 5.444914386472304635 ) ) ;
#11002 = DIRECTION ( 'NONE',  ( 0.000000000000000000, 0.000000000000000000, 1.000000000000000000 ) ) ;
#11003 = CARTESIAN_POINT ( 'NONE',  ( 98.15313185440923860, -4.458734124999987891, 10.87500000136559208 ) ) ;
#11004 = CARTESIAN_POINT ( 'NONE',  ( 9.598844408820456309, 38.32109374999999574, -9.598844408820458085 ) ) ;
#11005 = CARTESIAN_POINT ( 'NONE',  ( 99.99999999999995737, 81.18750000136559208, -4.458734125000016313 ) ) ;
#11006 = CARTESIAN_POINT ( 'NONE',  ( 208.1451861577818079, 38.51953125108393294, 5.444914386472293977 ) ) ;
#11007 = CARTESIAN_POINT ( 'NONE',  ( 13.14518615778179722, 38.02343750108395426, -5.444914386472297529 ) ) ;
#11008 = DIRECTION ( 'NONE',  ( -1.000000000000000000, 0.000000000000000000, 0.000000000000000000 ) ) ;
#11009 = CARTESIAN_POINT ( 'NONE',  ( 208.1451861577818079, 40.30546875108393579, 5.444914386472293977 ) ) ;
#11010 = CARTESIAN_POINT ( 'NONE',  ( 108.0825317499999869, 112.6261737610028320, -50.52499999726881441 ) ) ;
#11011 = ORIENTED_EDGE ( 'NONE', *, *, #25297, .F. ) ;
#11012 = EDGE_CURVE ( 'NONE', #19984, #27020, #9878, .T. ) ;
#11013 = CARTESIAN_POINT ( 'NONE',  ( -9.598844408820458085, 36.93203124999999432, -9.598844408820458085 ) ) ;
#11014 = CARTESIAN_POINT ( 'NONE',  ( -9.295050272127046043, 35.69179687608393436, -9.295050272127046043 ) ) ;
#11015 = ORIENTED_EDGE ( 'NONE', *, *, #27810, .T. ) ;
#11016 = CARTESIAN_POINT ( 'NONE',  ( 130.0000000000000000, 36.58476562608393579, -13.14518615778179544 ) ) ;
#11017 = CARTESIAN_POINT ( 'NONE',  ( 55.70494972787295751, 34.89804687608393152, -9.295050272127046043 ) ) ;
#11018 = CIRCLE ( 'NONE', #10582, 2.500000000000008882 ) ;
#11019 = CARTESIAN_POINT ( 'NONE',  ( 181.8548138422182205, 35.98945312608393721, 0.000000000000000000 ) ) ;
#11020 = VERTEX_POINT ( 'NONE', #3473 ) ;
#11021 = CARTESIAN_POINT ( 'NONE',  ( 104.9999999999999716, 1.449011120738813565E-14, 12.49999999999999822 ) ) ;
#11022 = CARTESIAN_POINT ( 'NONE',  ( -9.295050272127046043, 33.31054687608393294, -9.295050272127046043 ) ) ;
#11023 =( BOUNDED_CURVE ( )  B_SPLINE_CURVE ( 2, ( #21983, #6304, #14980, #23699, #12972, #10707, #21705, #2180, #10842 ),
 .UNSPECIFIED., .F., .T. ) 
 B_SPLINE_CURVE_WITH_KNOTS ( ( 3, 2, 2, 2, 3 ),
 ( 0.4791666666666667962, 0.4895833333333333703, 0.5000000000000000000, 0.5104166666666665186, 0.5208333333333332593 ),
 .UNSPECIFIED. ) 
 CURVE ( )  GEOMETRIC_REPRESENTATION_ITEM ( )  RATIONAL_B_SPLINE_CURVE ( ( 0.9999999999999992228, 0.9238795325112875156, 1.000000000000000000, 0.9238795325112867385, 1.000000000000000000, 0.9238795325112867385, 1.000000000000000000, 0.9238795325112875156, 0.9999999999999992228 ) ) 
 REPRESENTATION_ITEM ( '' )  );
#11024 = CARTESIAN_POINT ( 'NONE',  ( 129.1234737346379688, 51.45968077934942642, -15.00000000000033928 ) ) ;
#11025 = ADVANCED_FACE ( 'NONE', ( #12140 ), #21679, .T. ) ;
#11026 = FACE_OUTER_BOUND ( 'NONE', #14057, .T. ) ;
#11027 = CARTESIAN_POINT ( 'NONE',  ( 124.3771271284221314, 39.66054687716786731, 13.57481594606304753 ) ) ;
#11028 = DIRECTION ( 'NONE',  ( 0.000000000000000000, 0.000000000000000000, 1.000000000000000000 ) ) ;
#11029 = ADVANCED_FACE ( 'NONE', ( #17056 ), #10916, .F. ) ;
#11030 = CARTESIAN_POINT ( 'NONE',  ( -8.312177448680279460E-16, 34.45156249999999432, -13.57481594606304576 ) ) ;
#11031 = DIRECTION ( 'NONE',  ( 0.000000000000000000, -1.000000000000000000, 0.000000000000000000 ) ) ;
#11032 = ADVANCED_FACE ( 'NONE', ( #16437 ), #3336, .T. ) ;
#11033 = CARTESIAN_POINT ( 'NONE',  ( 181.8548138422182205, 40.55351562608393579, 0.000000000000000000 ) ) ;
#11034 = FILL_AREA_STYLE_COLOUR ( '', #17710 ) ;
#11035 = CARTESIAN_POINT ( 'NONE',  ( 98.15313185440925281, -4.458734124999987891, 10.62500000136559208 ) ) ;
#11036 = ORIENTED_EDGE ( 'NONE', *, *, #899, .F. ) ;
#11037 = CARTESIAN_POINT ( 'NONE',  ( 98.53841926354351699, 123.0500000010924850, 1.461580736456455920 ) ) ;
#11038 = CARTESIAN_POINT ( 'NONE',  ( 101.8468681455906903, -4.458734124999987891, 13.75000000136559208 ) ) ;
#11039 = CARTESIAN_POINT ( 'NONE',  ( 130.7238719380277132, 53.51529642094861572, 14.99999999999996447 ) ) ;
#11040 = EDGE_CURVE ( 'NONE', #8271, #20304, #27357, .T. ) ;
#11041 = CARTESIAN_POINT ( 'NONE',  ( -13.14518615778179544, 39.75976562608393294, 0.000000000000000000 ) ) ;
#11042 = DIRECTION ( 'NONE',  ( 0.000000000000000000, -1.000000000000000000, 0.000000000000000000 ) ) ;
#11043 = CARTESIAN_POINT ( 'NONE',  ( 104.4587341249999781, 83.12500000136560629, 1.846868145590721655 ) ) ;
#11044 = CARTESIAN_POINT ( 'NONE',  ( 78.14518615778179367, 34.74921875108395142, 5.444914386472293977 ) ) ;
#11045 = CARTESIAN_POINT ( 'NONE',  ( 102.4976396683250925, 102.3130555110000159, -44.77500000273119696 ) ) ;
#11046 = CARTESIAN_POINT ( 'NONE',  ( -13.14518615778179189, 36.63437500108393863, 5.444914386472304635 ) ) ;
#11047 = ADVANCED_BREP_SHAPE_REPRESENTATION ( '', ( #16871, #26844 ), #17253 ) ;
#11048 = LINE ( 'NONE', #21914, #1216 ) ;
#11049 = CARTESIAN_POINT ( 'NONE',  ( 130.0000000000000000, 36.03906250000000000, -13.57481594606304576 ) ) ;
#11050 = CARTESIAN_POINT ( 'NONE',  ( 92.99999999999998579, 110.0000000000000000, -49.00000000000001421 ) ) ;
#11051 = CARTESIAN_POINT ( 'NONE',  ( 143.5748159460630404, 38.96601562499999005, 5.622872871577869525 ) ) ;
#11052 = EDGE_LOOP ( 'NONE', ( #502, #25173, #5678, #28090 ) ) ;
#11053 = DIRECTION ( 'NONE',  ( -0.000000000000000000, 1.000000000000000000, -0.000000000000000000 ) ) ;
#11054 = CARTESIAN_POINT ( 'NONE',  ( -9.295050272127044266, 36.88242187608393152, 9.295050272127047819 ) ) ;
#11055 = CARTESIAN_POINT ( 'NONE',  ( 5.622872871577871301, 37.67617187716787441, -13.57481594606304753 ) ) ;
#11056 = CARTESIAN_POINT ( 'NONE',  ( 135.4449143864723055, 37.62656250108393863, 13.14518615778179189 ) ) ;
#11057 = CARTESIAN_POINT ( 'NONE',  ( 59.37712712842213136, 34.89804687716787868, 13.57481594606304753 ) ) ;
#11058 = EDGE_CURVE ( 'NONE', #3039, #27020, #25503, .T. ) ;
#11059 = CARTESIAN_POINT ( 'NONE',  ( 1.685511649082876318, 35.99999999999997868, 13.05727741351675775 ) ) ;
#11060 = CARTESIAN_POINT ( 'NONE',  ( -5.444914386472297529, 40.40468750108393436, -13.14518615778179900 ) ) ;
#11061 = CARTESIAN_POINT ( 'NONE',  ( 96.46446609406721961, -3.535533905932727539, 3.124999999999999112 ) ) ;
#11062 = AXIS2_PLACEMENT_3D ( 'NONE', #20354, #24200, #20070 ) ;
#11063 = DIRECTION ( 'NONE',  ( -0.000000000000000000, -1.000000000000000000, -0.000000000000000000 ) ) ;
#11064 = ADVANCED_FACE ( 'NONE', ( #5437 ), #18110, .F. ) ;
#11065 = CARTESIAN_POINT ( 'NONE',  ( 181.8548138422181921, 35.74140625108393721, -5.444914386472297529 ) ) ;
#11066 = DIRECTION ( 'NONE',  ( 0.000000000000000000, 0.000000000000000000, 1.000000000000000000 ) ) ;
#11067 = EDGE_CURVE ( 'NONE', #12084, #12573, #7412, .T. ) ;
#11068 = CARTESIAN_POINT ( 'NONE',  ( 102.0710678118654187, 93.18749999999998579, -5.000000000000031974 ) ) ;
#11070 = ORIENTED_EDGE ( 'NONE', *, *, #12602, .T. ) ;
#11069 = CARTESIAN_POINT ( 'NONE',  ( -8.312177448680279460E-16, 39.21406249999999716, -13.57481594606304576 ) ) ;
#11071 = CARTESIAN_POINT ( 'NONE',  ( 103.5355339059327093, 3.535533905932755072, 6.624999999999999112 ) ) ;
#11072 = CARTESIAN_POINT ( 'NONE',  ( -5.622872871577688336, 32.21914062716787441, -13.57481594606323050 ) ) ;
#11073 = CARTESIAN_POINT ( 'NONE',  ( 2.493653234604083739E-15, 38.81718749999999574, 13.57481594606304576 ) ) ;
#11074 = CARTESIAN_POINT ( 'NONE',  ( 9.295050272127046043, 36.48554687608393721, -9.295050272127046043 ) ) ;
#11075 = CARTESIAN_POINT ( 'NONE',  ( -9.295050272127044266, 35.09648437608392868, 9.295050272127047819 ) ) ;
#11076 = CARTESIAN_POINT ( 'NONE',  ( 204.5988444088204687, 34.94765624999999432, 9.598844408820456309 ) ) ;
#11077 = CARTESIAN_POINT ( 'NONE',  ( 51.42518405393695957, 40.15664062499999432, -5.622872871577872189 ) ) ;
#11078 = CARTESIAN_POINT ( 'NONE',  ( 95.54126587499995082, -1.846868145590724986, 0.7500000013655925279 ) ) ;
#11079 = CARTESIAN_POINT ( 'NONE',  ( 78.14518615778179367, 36.13828125108393863, 5.444914386472293977 ) ) ;
#11080 =( BOUNDED_CURVE ( )  B_SPLINE_CURVE ( 2, ( #3262, #2834, #9377, #16362, #7523, #16070, #24778, #24642, #852 ),
 .UNSPECIFIED., .F., .F. ) 
 B_SPLINE_CURVE_WITH_KNOTS ( ( 3, 2, 2, 2, 3 ),
 ( 0.2291666666666665741, 0.2395833333333332316, 0.2499999999999998335, 0.2604166666666665186, 0.2708333333333330928 ),
 .UNSPECIFIED. ) 
 CURVE ( )  GEOMETRIC_REPRESENTATION_ITEM ( )  RATIONAL_B_SPLINE_CURVE ( ( 1.000000000000000666, 0.9238795325112861834, 1.000000000000000000, 0.9238795325112867385, 1.000000000000000000, 0.9238795325112867385, 1.000000000000000000, 0.9238795325112884038, 0.9999999999999983347 ) ) 
 REPRESENTATION_ITEM ( '' )  );
#11081 = CARTESIAN_POINT ( 'NONE',  ( 96.84719886470459471, 3.152801135295383084, 3.312500001365592972 ) ) ;
#11082 = CARTESIAN_POINT ( 'NONE',  ( -13.57481594606304398, 35.59257812716789715, 5.622872871577880183 ) ) ;
#11083 = EDGE_CURVE ( 'NONE', #15376, #19908, #27247, .T. ) ;
#11084 = CARTESIAN_POINT ( 'NONE',  ( 94.99999999999997158, 2.071067811865471953, 4.937500000000000000 ) ) ;
#11085 = CARTESIAN_POINT ( 'NONE',  ( 2.493653234604083739E-15, 36.43593749999999432, 13.57481594606304576 ) ) ;
#11086 = CARTESIAN_POINT ( 'NONE',  ( 135.4449143864723055, 37.03125000108393294, 13.14518615778179189 ) ) ;
#11087 = EDGE_LOOP ( 'NONE', ( #13227, #17769, #1317, #10479 ) ) ;
#11088 = EDGE_LOOP ( 'NONE', ( #8193, #2327, #17952, #18279 ) ) ;
#11089 = CARTESIAN_POINT ( 'NONE',  ( 104.9999999999999574, 82.43750000000002842, 2.071067811865462627 ) ) ;
#11090 = CARTESIAN_POINT ( 'NONE',  ( 103.5355339059327093, 80.75000000273119838, -3.535533905932755072 ) ) ;
#11091 = CARTESIAN_POINT ( 'NONE',  ( 99.99999999999998579, 90.25000000000000000, -4.999999999999997335 ) ) ;
#11092 = CARTESIAN_POINT ( 'NONE',  ( 13.57481594606304576, 34.25312499999999716, -1.662435489736055892E-15 ) ) ;
#11093 = CARTESIAN_POINT ( 'NONE',  ( 94.33688103937535629, 105.8855032339526758, -52.80000000000001137 ) ) ;
#11094 = CARTESIAN_POINT ( 'NONE',  ( 55.40115559117954547, 40.30546874999999574, 9.598844408820459861 ) ) ;
#11095 = VERTEX_POINT ( 'NONE', #7270 ) ;
#11096 = CARTESIAN_POINT ( 'NONE',  ( 95.00000000000000000, 95.37499999726881583, -7.551217303480904118E-15 ) ) ;
#11097 = CARTESIAN_POINT ( 'NONE',  ( 99.99999999999995737, 4.458734125000016313, 1.437500001365592972 ) ) ;
#11098 = EDGE_CURVE ( 'NONE', #26503, #13118, #24810, .T. ) ;
#11099 = EDGE_LOOP ( 'NONE', ( #5801, #8695, #3968, #5777, #10257 ) ) ;
#11100 = CARTESIAN_POINT ( 'NONE',  ( -8.049105076161786076E-16, 32.61601562608393579, -13.14518615778179544 ) ) ;
#11101 = CARTESIAN_POINT ( 'NONE',  ( -8.049105076161786076E-16, 40.55351562608393579, -13.14518615778179544 ) ) ;
#11102 = CARTESIAN_POINT ( 'NONE',  ( 181.4251840539369596, 34.00507812716787015, 5.622872871577880183 ) ) ;
#11103 = CARTESIAN_POINT ( 'NONE',  ( 9.295050272127047819, 36.88242187608393152, 9.295050272127046043 ) ) ;
#11104 = CARTESIAN_POINT ( 'NONE',  ( 51.85481384221820633, 40.65273437608393436, 0.000000000000000000 ) ) ;
#11105 = CARTESIAN_POINT ( 'NONE',  ( 135.4449143864723339, 37.82500000108392868, 13.14518615778179189 ) ) ;
#11106 = CARTESIAN_POINT ( 'NONE',  ( -9.295050272127046043, 35.89023437608393152, -9.295050272127046043 ) ) ;
#11107 = CARTESIAN_POINT ( 'NONE',  ( 135.4449143864723055, 33.95546875108393436, -13.14518615778179900 ) ) ;
#11108 = CARTESIAN_POINT ( 'NONE',  ( 59.37712712842213136, 34.00507812499999716, 13.57481594606304753 ) ) ;
#11109 = CARTESIAN_POINT ( 'NONE',  ( -9.598844408820458085, 34.55078124999999289, -9.598844408820458085 ) ) ;
#11110 = CARTESIAN_POINT ( 'NONE',  ( 103.1528011352953342, -3.152801135295355106, 11.06250000136559208 ) ) ;
#11111 = DIRECTION ( 'NONE',  ( 0.000000000000000000, 0.000000000000000000, 1.000000000000000000 ) ) ;
#11112 = CARTESIAN_POINT ( 'NONE',  ( 101.8468681455906903, -4.458734124999987891, 1.750000001365591862 ) ) ;
#11113 = CARTESIAN_POINT ( 'NONE',  ( 0.000000000000000000, 31.00000000000000000, -13.57481594606304576 ) ) ;
#11114 = DIRECTION ( 'NONE',  ( 0.000000000000000000, 0.000000000000000000, -1.000000000000000000 ) ) ;
#11115 = CARTESIAN_POINT ( 'NONE',  ( 101.8468681455907046, 81.00000000136560629, 4.458734124999987891 ) ) ;
#11116 = CARTESIAN_POINT ( 'NONE',  ( 99.99999999999997158, 118.4984768113314146, -50.12499999726882294 ) ) ;
#11117 = CARTESIAN_POINT ( 'NONE',  ( -5.444914386472297529, 35.04687500108393294, -13.14518615778179900 ) ) ;
#11118 = CARTESIAN_POINT ( 'NONE',  ( 102.4976396683250783, 117.6869444889999841, -48.47499999726882436 ) ) ;
#11119 = ORIENTED_EDGE ( 'NONE', *, *, #1334, .F. ) ;
#11120 = CARTESIAN_POINT ( 'NONE',  ( 95.67376207875072680, 115.9545556584642867, -50.80000000546237260 ) ) ;
#11121 = CARTESIAN_POINT ( 'NONE',  ( 104.9999999999999716, 1.449011120738813565E-14, 12.62500000273118594 ) ) ;
#11122 = DIRECTION ( 'NONE',  ( 0.000000000000000000, 0.000000000000000000, 1.000000000000000000 ) ) ;
#11123 = CARTESIAN_POINT ( 'NONE',  ( 200.4449143864723055, 37.92421875108392726, -13.14518615778179900 ) ) ;
#11124 = ORIENTED_EDGE ( 'NONE', *, *, #14556, .F. ) ;
#11125 = LINE ( 'NONE', #17273, #9231 ) ;
#11126 = CARTESIAN_POINT ( 'NONE',  ( 97.83688103937535629, 116.6573956140660897, -48.89999999453763735 ) ) ;
#11127 = CARTESIAN_POINT ( 'NONE',  ( 101.8468681455906903, 4.458734125000016313, 13.37500000136559386 ) ) ;
#11128 = ORIENTED_EDGE ( 'NONE', *, *, #7333, .T. ) ;
#11129 = CARTESIAN_POINT ( 'NONE',  ( 99.99999999999998579, 118.4984768113314004, -51.87500000273118417 ) ) ;
#11130 = AXIS2_PLACEMENT_3D ( 'NONE', #19028, #8060, #23186 ) ;
#11131 = CARTESIAN_POINT ( 'NONE',  ( 102.4999999999999716, 123.7500000000000142, 1.035533905932722876 ) ) ;
#11132 = CARTESIAN_POINT ( 'NONE',  ( 135.6228728715778686, 32.11992187716787583, -13.57481594606304753 ) ) ;
#11133 = CARTESIAN_POINT ( 'NONE',  ( 114.9999999999999858, 95.00000000000000000, 14.99999999999999289 ) ) ;
#11134 = CARTESIAN_POINT ( 'NONE',  ( 96.46446609406726225, 95.49999999726881583, 3.535533905932723986 ) ) ;
#11135 = CARTESIAN_POINT ( 'NONE',  ( 65.00000000000000000, 37.37851562608393863, -13.14518615778179544 ) ) ;
#11136 = CARTESIAN_POINT ( 'NONE',  ( 73.40231578122690337, 54.99999999485618929, -15.00000000000000000 ) ) ;
#11137 = CARTESIAN_POINT ( 'NONE',  ( 189.3771271284221314, 40.85117187499999147, -13.57481594606304753 ) ) ;
#11138 = CARTESIAN_POINT ( 'NONE',  ( 70.36494796471481550, 36.00000000000002842, 12.09311862596063136 ) ) ;
#11139 = ORIENTED_EDGE ( 'NONE', *, *, #8072, .F. ) ;
#11140 = CARTESIAN_POINT ( 'NONE',  ( -9.295050272127046043, 40.65273437608393436, -9.295050272127046043 ) ) ;
#11141 = DIRECTION ( 'NONE',  ( 1.000000000000000000, 0.000000000000000000, 0.000000000000000000 ) ) ;
#11142 = CARTESIAN_POINT ( 'NONE',  ( 99.99999999999995737, 4.458734125000016313, 9.437500001365593860 ) ) ;
#11143 = CARTESIAN_POINT ( 'NONE',  ( 104.9999999999999858, 95.00000000000000000, -6.938893903907228378E-15 ) ) ;
#11144 = CARTESIAN_POINT ( 'NONE',  ( 96.84719886470459471, 80.31250000136559208, -3.152801135295383084 ) ) ;
#11145 = CARTESIAN_POINT ( 'NONE',  ( 204.2950502721270425, 40.25585937608393294, -9.295050272127046043 ) ) ;
#11146 = CARTESIAN_POINT ( 'NONE',  ( 13.14518615778179722, 38.81718750108393579, -5.444914386472297529 ) ) ;
#11147 = EDGE_CURVE ( 'NONE', #21025, #26276, #11837, .T. ) ;
#11148 = AXIS2_PLACEMENT_3D ( 'NONE', #23749, #12885, #10338 ) ;
#11149 = CARTESIAN_POINT ( 'NONE',  ( -5.622872871577873966, 37.67617187499999432, -13.57481594606304753 ) ) ;
#11150 = LINE ( 'NONE', #13142, #8642 ) ;
#11151 = CARTESIAN_POINT ( 'NONE',  ( 106.5389055433250860, 105.2492070361643215, -54.82499999726882578 ) ) ;
#11152 = VERTEX_POINT ( 'NONE', #886 ) ;
#11153 = VERTEX_POINT ( 'NONE', #24951 ) ;
#11154 = CARTESIAN_POINT ( 'NONE',  ( -5.622872871577873077, 37.67617187499999432, -13.57481594606304753 ) ) ;
#11155 = CARTESIAN_POINT ( 'NONE',  ( 9.295050272127046043, 38.66835937608393436, -9.295050272127046043 ) ) ;
#11156 = CIRCLE ( 'NONE', #12963, 13.57481594606304398 ) ;
#11157 = ORIENTED_EDGE ( 'NONE', *, *, #20458, .T. ) ;
#11158 = CARTESIAN_POINT ( 'NONE',  ( 136.9444263933115167, 31.75150625057403175, -11.16113171639042356 ) ) ;
#11159 = CARTESIAN_POINT ( 'NONE',  ( 74.29505027212704249, 33.70742187608393436, 9.295050272127046043 ) ) ;
#11160 = CARTESIAN_POINT ( 'NONE',  ( 200.4449143864723055, 36.53515625108393294, -13.14518615778179900 ) ) ;
#11161 = VERTEX_POINT ( 'NONE', #15960 ) ;
#11162 = CYLINDRICAL_SURFACE ( 'NONE', #4770, 5.000000000000004441 ) ;
#11163 = CARTESIAN_POINT ( 'NONE',  ( 13.14518615778179900, 33.75703125108393010, 5.444914386472293977 ) ) ;
#11164 = CARTESIAN_POINT ( 'NONE',  ( 121.6040612587083416, 54.99999999495823033, -15.00000000000000000 ) ) ;
#11165 = CARTESIAN_POINT ( 'NONE',  ( 92.99999999999998579, 110.0000000000000000, -53.00000000000001421 ) ) ;
#11166 = CARTESIAN_POINT ( 'NONE',  ( 116.4251840539369596, 40.30546875216787583, 0.000000000000000000 ) ) ;
#11167 = FACE_OUTER_BOUND ( 'NONE', #1119, .T. ) ;
#11168 = DIRECTION ( 'NONE',  ( 0.000000000000000000, 0.000000000000000000, -1.000000000000000000 ) ) ;
#11169 = CARTESIAN_POINT ( 'NONE',  ( 98.23223304703363112, 123.6000000021849416, 1.767766952966351557 ) ) ;
#11170 = CARTESIAN_POINT ( 'NONE',  ( 98.96446609406726225, 124.3500000000000085, 2.499999999999981348 ) ) ;
#11171 = EDGE_LOOP ( 'NONE', ( #12932, #15147, #4562, #2491 ) ) ;
#11172 = CARTESIAN_POINT ( 'NONE',  ( 104.4587341249999781, -1.846868145590721655, 7.875000001365591196 ) ) ;
#11173 = AXIS2_PLACEMENT_3D ( 'NONE', #17806, #6168, #26509 ) ;
#11174 = ORIENTED_EDGE ( 'NONE', *, *, #6347, .T. ) ;
#11175 = CARTESIAN_POINT ( 'NONE',  ( 101.0355339059327378, 123.2500000021849758, -2.499999999999997780 ) ) ;
#11176 = CARTESIAN_POINT ( 'NONE',  ( 104.4587341249999639, 1.442382525525748735E-14, 7.937500001365592084 ) ) ;
#11177 = CARTESIAN_POINT ( 'NONE',  ( 126.2834658862103225, 51.46663580899353718, 14.99999999999996270 ) ) ;
#11178 = CARTESIAN_POINT ( 'NONE',  ( -5.444914386472299306, 37.52734375108393294, 13.14518615778179722 ) ) ;
#11179 = CARTESIAN_POINT ( 'NONE',  ( 130.0000000000000000, 38.51953125216787299, -13.57481594606304576 ) ) ;
#11180 = CARTESIAN_POINT ( 'NONE',  ( 98.15313185440925281, 80.87500000136560629, 4.458734124999987891 ) ) ;
#11181 = CARTESIAN_POINT ( 'NONE',  ( 55.70494972787295751, 33.70742187608393436, 9.295050272127047819 ) ) ;
#11182 = CARTESIAN_POINT ( 'NONE',  ( 104.9952793366501851, 103.1245878333314323, -52.42500000273119554 ) ) ;
#11183 = CARTESIAN_POINT ( 'NONE',  ( -13.14518615778179544, 38.96601562608393721, 0.000000000000000000 ) ) ;
#11184 = ADVANCED_FACE ( 'NONE', ( #5153 ), #22828, .T. ) ;
#11185 = LINE ( 'NONE', #19904, #23939 ) ;
#11186 = CARTESIAN_POINT ( 'NONE',  ( 101.7677669209684552, 123.0000000000000000, 1.767766984964258992 ) ) ;
#11187 = CARTESIAN_POINT ( 'NONE',  ( 105.6631189606246153, 114.1144967660473242, -49.80000000000001137 ) ) ;
#11188 = CARTESIAN_POINT ( 'NONE',  ( 116.4251840539369596, 37.82499999999999574, 0.000000000000000000 ) ) ;
#11189 = ORIENTED_EDGE ( 'NONE', *, *, #6021, .T. ) ;
#11190 = CARTESIAN_POINT ( 'NONE',  ( 92.99999999999995737, 112.2744378736303048, -51.10000000000000853 ) ) ;
#11191 = EDGE_CURVE ( 'NONE', #17588, #17231, #12650, .T. ) ;
#11192 = CARTESIAN_POINT ( 'NONE',  ( 13.14518615778179900, 35.54296875108394715, 5.444914386472293977 ) ) ;
#11193 = CARTESIAN_POINT ( 'NONE',  ( 9.598844408820459861, 36.63437500216787157, 9.598844408820456309 ) ) ;
#11194 =( BOUNDED_CURVE ( )  B_SPLINE_CURVE ( 2, ( #1374, #23030, #5923, #8187, #5645, #14589, #23168, #3781, #25576 ),
 .UNSPECIFIED., .F., .T. ) 
 B_SPLINE_CURVE_WITH_KNOTS ( ( 3, 2, 2, 2, 3 ),
 ( 0.6041666666666668517, 0.6145833333333334814, 0.6250000000000001110, 0.6354166666666667407, 0.6458333333333333703 ),
 .UNSPECIFIED. ) 
 CURVE ( )  GEOMETRIC_REPRESENTATION_ITEM ( )  RATIONAL_B_SPLINE_CURVE ( ( 0.9999999999999983347, 0.9238795325112884038, 1.000000000000000000, 0.9238795325112867385, 1.000000000000000000, 0.9238795325112867385, 1.000000000000000000, 0.9238795325112867385, 1.000000000000000000 ) ) 
 REPRESENTATION_ITEM ( '' )  );
#11195 = AXIS2_PLACEMENT_3D ( 'NONE', #442, #17819, #22387 ) ;
#11196 = CARTESIAN_POINT ( 'NONE',  ( 104.9999999999999574, 2.071067811865491937, 7.687500002731185944 ) ) ;
#11197 = CARTESIAN_POINT ( 'NONE',  ( 139.2950502721270425, 35.49335937608393010, -9.295050272127046043 ) ) ;
#11198 = CARTESIAN_POINT ( 'NONE',  ( 74.59884440882045453, 33.65781250216787157, -9.598844408820458085 ) ) ;
#11199 = ORIENTED_EDGE ( 'NONE', *, *, #246, .T. ) ;
#11200 = DIRECTION ( 'NONE',  ( 0.000000000000000000, 0.000000000000000000, -1.000000000000000000 ) ) ;
#11201 = CARTESIAN_POINT ( 'NONE',  ( 9.598844408820459861, 32.66562500216787157, 9.598844408820456309 ) ) ;
#11202 = VECTOR ( 'NONE', #13979, 1000.000000000000000 ) ;
#11203 = CARTESIAN_POINT ( 'NONE',  ( 99.99999999999995737, -4.999999999999990230, 2.249999999999998668 ) ) ;
#11204 = EDGE_CURVE ( 'NONE', #17571, #21956, #23504, .T. ) ;
#11205 = CARTESIAN_POINT ( 'NONE',  ( 91.91746824999997045, 112.6261737610028320, -49.97499999726882436 ) ) ;
#11206 = CARTESIAN_POINT ( 'NONE',  ( 208.1451861577818079, 34.60039062608392868, -1.609821015232357215E-15 ) ) ;
#11207 = CARTESIAN_POINT ( 'NONE',  ( 102.0710678118654329, 5.000000000000018652, 5.812500002731185056 ) ) ;
#11208 = FILL_AREA_STYLE_COLOUR ( '', #7776 ) ;
#11209 = CARTESIAN_POINT ( 'NONE',  ( 94.99999999999995737, -2.071067811865466624, 10.18750000273118417 ) ) ;
#11210 = CARTESIAN_POINT ( 'NONE',  ( 107.0000000000000000, 107.7255621263696668, -47.59999999453764019 ) ) ;
#11211 = CARTESIAN_POINT ( 'NONE',  ( -5.622872871577873077, 36.08867187500000284, -13.57481594606304753 ) ) ;
#11212 = FACE_OUTER_BOUND ( 'NONE', #23422, .T. ) ;
#11213 = AXIS2_PLACEMENT_3D ( 'NONE', #26259, #6859, #13252 ) ;
#11214 = CARTESIAN_POINT ( 'NONE',  ( 13.14518615778179544, 37.18007812608393436, -1.609821015232357215E-15 ) ) ;
#11215 = CARTESIAN_POINT ( 'NONE',  ( 13.14518615778179900, 36.23750000108393010, -5.444914386472297529 ) ) ;
#11216 = CARTESIAN_POINT ( 'NONE',  ( 204.5988444088204687, 33.36015624999999574, 9.598844408820456309 ) ) ;
#11217 = ITEM_DEFINED_TRANSFORMATION ( 'NONE', 'NONE', #26322,  #26844 ) ;
#11218 = CARTESIAN_POINT ( 'NONE',  ( 104.9952793366501709, 103.1245878333314465, -46.67500000273118843 ) ) ;
#11219 = CARTESIAN_POINT ( 'NONE',  ( -8.312177448680279460E-16, 39.21406249999999716, -13.57481594606304576 ) ) ;
#11220 = CARTESIAN_POINT ( 'NONE',  ( 74.29505027212704249, 36.28710937608393294, -9.295050272127046043 ) ) ;
#11221 = CARTESIAN_POINT ( 'NONE',  ( 103.1528011352953342, -3.152801135295355106, 3.812500001365591640 ) ) ;
#11222 = CARTESIAN_POINT ( 'NONE',  ( 102.2453236122039471, 123.0000000000000000, -1.108986377174830507 ) ) ;
#11223 = EDGE_LOOP ( 'NONE', ( #6894, #399, #10278, #21614 ) ) ;
#11224 = EDGE_CURVE ( 'NONE', #2100, #21367, #21096, .T. ) ;
#11225 = CARTESIAN_POINT ( 'NONE',  ( 195.0000000000000000, 50.00000000000000000, -2.255140518769849538E-14 ) ) ;
#11226 = CARTESIAN_POINT ( 'NONE',  ( 9.598844408820456309, 35.93984374999999432, -9.598844408820458085 ) ) ;
#11227 = CARTESIAN_POINT ( 'NONE',  ( 116.8548138422182205, 39.16445312608393436, 0.000000000000000000 ) ) ;
#11228 = VERTEX_POINT ( 'NONE', #9970 ) ;
#11229 = CARTESIAN_POINT ( 'NONE',  ( 94.99999999999995737, 82.93750000000000000, -2.071067811865491048 ) ) ;
#11230 = CARTESIAN_POINT ( 'NONE',  ( 9.598844408820456309, 35.14609374999999858, -9.598844408820458085 ) ) ;
#11231 = CARTESIAN_POINT ( 'NONE',  ( 102.0710678118654329, 82.43750000273119838, 4.999999999999989342 ) ) ;
#11232 = CARTESIAN_POINT ( 'NONE',  ( 96.84719886470463734, 91.93749999863440792, 3.152801135295351997 ) ) ;
#11233 = CARTESIAN_POINT ( 'NONE',  ( 130.0000000000000000, 40.80156249999999574, -13.57481594606304576 ) ) ;
#11234 = EDGE_CURVE ( 'NONE', #6002, #13072, #2741, .T. ) ;
#11235 = CARTESIAN_POINT ( 'NONE',  ( 105.6631189606246153, 114.1144967660473242, -47.80000000000001137 ) ) ;
#11236 = CARTESIAN_POINT ( 'NONE',  ( 65.00000000000000000, 40.40468749999999432, 13.57481594606304576 ) ) ;
#11237 = ORIENTED_EDGE ( 'NONE', *, *, #14372, .T. ) ;
#11238 = DIRECTION ( 'NONE',  ( 1.224646799147353454E-16, 0.000000000000000000, -1.000000000000000000 ) ) ;
#11239 = CARTESIAN_POINT ( 'NONE',  ( 102.0710678118654329, 5.000000000000018652, 12.68749999999999822 ) ) ;
#11240 = ADVANCED_FACE ( 'NONE', ( #20961 ), #27656, .T. ) ;
#11241 = ORIENTED_EDGE ( 'NONE', *, *, #20642, .T. ) ;
#11242 = CARTESIAN_POINT ( 'NONE',  ( -13.14518615778179544, 35.98945312608393721, 0.000000000000000000 ) ) ;
#11243 = CARTESIAN_POINT ( 'NONE',  ( 195.0000000000000000, 35.74140625216787015, 13.57481594606304576 ) ) ;
#11244 = CARTESIAN_POINT ( 'NONE',  ( 13.14518615778179722, 33.85625000108393579, -5.444914386472297529 ) ) ;
#11245 = PRODUCT ( 'Integrated Vacuum Pressure Gauge', 'Integrated Vacuum Pressure Gauge', '', ( #25373 ) ) ;
#11246 = CARTESIAN_POINT ( 'NONE',  ( -13.57481594606304753, 40.95039062499999005, -5.622872871577872189 ) ) ;
#11247 = CARTESIAN_POINT ( 'NONE',  ( 124.5550856135277087, 37.42812500108394147, -13.14518615778179722 ) ) ;
#11248 = VERTEX_POINT ( 'NONE', #14789 ) ;
#11249 = CARTESIAN_POINT ( 'NONE',  ( 9.295050272127046043, 34.10429687608393579, -9.295050272127046043 ) ) ;
#11250 =( BOUNDED_CURVE ( )  B_SPLINE_CURVE ( 2, ( #7422, #3305, #11545, #7716, #20262, #24686, #7135, #11976, #13689 ),
 .UNSPECIFIED., .F., .F. ) 
 B_SPLINE_CURVE_WITH_KNOTS ( ( 3, 2, 2, 2, 3 ),
 ( 0.3958333333333331483, 0.4062499999999999445, 0.4166666666666667407, 0.4270833333333335369, 0.4375000000000003331 ),
 .UNSPECIFIED. ) 
 CURVE ( )  GEOMETRIC_REPRESENTATION_ITEM ( )  RATIONAL_B_SPLINE_CURVE ( ( 1.000000000000001110, 0.9238795325112855172, 1.000000000000000000, 0.9238795325112867385, 1.000000000000000000, 0.9238795325112867385, 1.000000000000000000, 0.9238795325112842960, 1.000000000000002442 ) ) 
 REPRESENTATION_ITEM ( '' )  );
#11251 = CARTESIAN_POINT ( 'NONE',  ( 116.8548138422182063, 31.87187500108393223, 5.444914386472304635 ) ) ;
#11252 = CARTESIAN_POINT ( 'NONE',  ( 51.42518405393695957, 36.23749999999999005, 0.000000000000000000 ) ) ;
#11253 = CARTESIAN_POINT ( 'NONE',  ( 0.000000000000000000, 40.99999999999999289, 0.000000000000000000 ) ) ;
#11254 = CARTESIAN_POINT ( 'NONE',  ( 95.54126587499995082, 1.846868145590750077, 11.62500000136559031 ) ) ;
#11255 = CARTESIAN_POINT ( 'NONE',  ( 99.99999999999995737, 80.87500000273119838, -5.000000000000018652 ) ) ;
#11256 = CARTESIAN_POINT ( 'NONE',  ( 95.54126587499996504, 1.387778780781445676E-14, 1.437500001365591196 ) ) ;
#11257 = CARTESIAN_POINT ( 'NONE',  ( 102.4976396683250925, 102.3130555110000159, -46.52500000273119696 ) ) ;
#11258 = DIRECTION ( 'NONE',  ( 0.000000000000000000, 1.000000000000000000, 0.000000000000000000 ) ) ;
#11259 = CARTESIAN_POINT ( 'NONE',  ( 104.9999999999999716, 1.449011120738813565E-14, 11.62500000273118417 ) ) ;
#11260 = CARTESIAN_POINT ( 'NONE',  ( 108.0825317499999869, 112.6261737610028320, -48.52499999726882152 ) ) ;
#11261 = CARTESIAN_POINT ( 'NONE',  ( 13.14518615778179544, 37.97382812608393721, -1.609821015232357215E-15 ) ) ;
#11262 = CARTESIAN_POINT ( 'NONE',  ( 94.33688103937535629, 105.8855032339526758, -48.29999999453764303 ) ) ;
#11263 = VERTEX_POINT ( 'NONE', #8252 ) ;
#11264 = DIRECTION ( 'NONE',  ( 1.000000000000000000, 0.000000000000000000, -7.228014483236696740E-18 ) ) ;
#11265 = CARTESIAN_POINT ( 'NONE',  ( 99.99999999999998579, 123.1500000010924794, 2.066987299999980099 ) ) ;
#11266 = CARTESIAN_POINT ( 'NONE',  ( 1.417506129906585201E-15, 36.00000000000000000, 11.57481594606304576 ) ) ;
#11267 = EDGE_CURVE ( 'NONE', #23999, #8135, #26594, .T. ) ;
#11268 = CARTESIAN_POINT ( 'NONE',  ( 200.4449143864723055, 37.13046875108393152, -13.14518615778179900 ) ) ;
#11269 = ORIENTED_EDGE ( 'NONE', *, *, #13761, .T. ) ;
#11270 = CYLINDRICAL_SURFACE ( 'NONE', #14441, 5.000000000000004441 ) ;
#11271 = CARTESIAN_POINT ( 'NONE',  ( 104.4587341249999781, -1.846868145590721655, 10.12500000136559386 ) ) ;
#11272 = ORIENTED_EDGE ( 'NONE', *, *, #22909, .T. ) ;
#11273 = CARTESIAN_POINT ( 'NONE',  ( 99.99999999999998579, 102.6397644303321215, -47.50000000000000711 ) ) ;
#11274 = CARTESIAN_POINT ( 'NONE',  ( 9.295050272127046043, 40.25585937608393294, -9.295050272127046043 ) ) ;
#11275 = CARTESIAN_POINT ( 'NONE',  ( 101.0355339059327378, 123.9500000000000028, -2.499999999999997780 ) ) ;
#11276 = VECTOR ( 'NONE', #19789, 1000.000000000000000 ) ;
#11277 = CARTESIAN_POINT ( 'NONE',  ( 124.5550856135277087, 40.40468750108393436, -13.14518615778179900 ) ) ;
#11278 = CARTESIAN_POINT ( 'NONE',  ( 13.14518615778179544, 39.56132812608393579, -1.609821015232357215E-15 ) ) ;
#11279 = CARTESIAN_POINT ( 'NONE',  ( 96.46446609406726225, 94.49999999726881583, 3.535533905932723986 ) ) ;
#11280 =( BOUNDED_CURVE ( )  B_SPLINE_CURVE ( 2, ( #27983, #327, #4459, #17704, #4178 ),
 .UNSPECIFIED., .F., .T. ) 
 B_SPLINE_CURVE_WITH_KNOTS ( ( 3, 2, 3 ),
 ( 0.4375000000000003331, 0.4479166666666667962, 0.4520580917964571177 ),
 .UNSPECIFIED. ) 
 CURVE ( )  GEOMETRIC_REPRESENTATION_ITEM ( )  RATIONAL_B_SPLINE_CURVE ( ( 0.9999999999999975575, 0.9238795325112891810, 1.000000000000000000, 0.9697362671728813055, 0.9635368512068493985 ) ) 
 REPRESENTATION_ITEM ( '' )  );
#11281 = CARTESIAN_POINT ( 'NONE',  ( 51.85481384221819923, 36.73359375108393010, -5.444914386472297529 ) ) ;
#11282 = CARTESIAN_POINT ( 'NONE',  ( 64.01693481490168836, 49.99999999948997242, -13.54930971656747474 ) ) ;
#11283 = CARTESIAN_POINT ( 'NONE',  ( 200.4449143864723055, 33.06250000108393294, 13.14518615778179189 ) ) ;
#11284 = ORIENTED_EDGE ( 'NONE', *, *, #6545, .T. ) ;
#11285 = DIRECTION ( 'NONE',  ( 5.782411586589358625E-17, -0.000000000000000000, 1.000000000000000000 ) ) ;
#11286 = VERTEX_POINT ( 'NONE', #25374 ) ;
#11287 = CARTESIAN_POINT ( 'NONE',  ( -9.295050272127044266, 36.88242187608393152, 9.295050272127047819 ) ) ;
#11288 = CARTESIAN_POINT ( 'NONE',  ( 101.8468681455907046, 4.458734125000016313, 12.37500000136559208 ) ) ;
#11289 = CARTESIAN_POINT ( 'NONE',  ( 70.44491438647229131, 37.62656250108393152, 13.14518615778179189 ) ) ;
#11290 = LINE ( 'NONE', #20011, #5161 ) ;
#11291 = CARTESIAN_POINT ( 'NONE',  ( 195.0000000000000000, 39.56132812608393579, -13.14518615778179544 ) ) ;
#11292 = CARTESIAN_POINT ( 'NONE',  ( -9.295050272127044266, 37.67617187608393436, 9.295050272127047819 ) ) ;
#11293 = CARTESIAN_POINT ( 'NONE',  ( -9.598844408820454532, 36.33671874999999574, 9.598844408820459861 ) ) ;
#11294 = CARTESIAN_POINT ( 'NONE',  ( 189.5550856135277229, 36.63437500108393863, -13.14518615778179722 ) ) ;
#11295 = CARTESIAN_POINT ( 'NONE',  ( 93.46109445667489979, 114.7507929638356785, -53.82499999726881867 ) ) ;
#11296 = AXIS2_PLACEMENT_3D ( 'NONE', #23213, #18788, #1558 ) ;
#11297 = VECTOR ( 'NONE', #7433, 1000.000000000000000 ) ;
#11298 = ORIENTED_EDGE ( 'NONE', *, *, #14123, .T. ) ;
#11299 = CARTESIAN_POINT ( 'NONE',  ( -13.57481594606304576, 33.90585937500000568, 5.622872871577880183 ) ) ;
#11300 = CARTESIAN_POINT ( 'NONE',  ( -9.295050272127044266, 33.50898437608393010, 9.295050272127047819 ) ) ;
#11301 = ORIENTED_EDGE ( 'NONE', *, *, #8104, .F. ) ;
#11302 = CARTESIAN_POINT ( 'NONE',  ( 139.2950502721270425, 34.10429687608393579, -9.295050272127046043 ) ) ;
#11303 = CARTESIAN_POINT ( 'NONE',  ( 78.14518615778179367, 33.01289062608393010, -1.609821015232357215E-15 ) ) ;
#11304 = CARTESIAN_POINT ( 'NONE',  ( 181.8548138422182205, 36.78320312608393294, 0.000000000000000000 ) ) ;
#11305 = ORIENTED_EDGE ( 'NONE', *, *, #21558, .F. ) ;
#11306 = CARTESIAN_POINT ( 'NONE',  ( 99.99999999999995737, 5.000000000000018652, 10.87500000273118594 ) ) ;
#11307 = CARTESIAN_POINT ( 'NONE',  ( -5.444914386472299306, 33.55859375108393294, 13.14518615778179722 ) ) ;
#11308 = CARTESIAN_POINT ( 'NONE',  ( 104.9999999999999716, 1.449011120738813565E-14, 5.625000002731185056 ) ) ;
#11309 = CARTESIAN_POINT ( 'NONE',  ( 135.6228728715778686, 40.05742187716786873, -13.57481594606304753 ) ) ;
#11310 = CARTESIAN_POINT ( 'NONE',  ( 65.00000000000000000, 52.00000000000000711, -11.57481594606305109 ) ) ;
#11311 = EDGE_CURVE ( 'NONE', #3364, #34, #25509, .T. ) ;
#11312 = CARTESIAN_POINT ( 'NONE',  ( 102.0710678118654329, 5.000000000000018652, 10.68749999999999822 ) ) ;
#11313 = CYLINDRICAL_SURFACE ( 'NONE', #13218, 5.000000000000004441 ) ;
#11314 = CARTESIAN_POINT ( 'NONE',  ( 73.75489895324048462, 50.00000000000000000, 10.39041163855394068 ) ) ;
#11315 = EDGE_LOOP ( 'NONE', ( #24088, #17751, #23216, #23112 ) ) ;
#11316 = CARTESIAN_POINT ( 'NONE',  ( 101.8468681455906903, -4.458734124999987891, 5.750000001365591196 ) ) ;
#11317 = ORIENTED_EDGE ( 'NONE', *, *, #26747, .T. ) ;
#11318 = CARTESIAN_POINT ( 'NONE',  ( 98.23223304703363112, 122.6000000021849559, -1.767766952966370209 ) ) ;
#11319 = CARTESIAN_POINT ( 'NONE',  ( 104.4587341249999781, -1.846868145590721655, 6.875000001365592972 ) ) ;
#11320 = CARTESIAN_POINT ( 'NONE',  ( 107.0000000000000142, 110.0000000000000000, -55.00000000000000711 ) ) ;
#11321 = AXIS2_PLACEMENT_3D ( 'NONE', #21423, #23416, #23141 ) ;
#11322 = CARTESIAN_POINT ( 'NONE',  ( -8.049105076161786076E-16, 36.38632812608393152, -13.14518615778179544 ) ) ;
#11323 = CARTESIAN_POINT ( 'NONE',  ( 78.57481594606305464, 39.16445312716788152, -5.622872871577873966 ) ) ;
#11324 = CARTESIAN_POINT ( 'NONE',  ( 70.44491438647230552, 35.74140625108393721, -13.14518615778179900 ) ) ;
#11325 =( BOUNDED_CURVE ( )  B_SPLINE_CURVE ( 2, ( #7231, #24776, #22357, #7374, #18647, #20217, #24639, #5546, #15789, #18071, #1133, #27352, #992, #14210, #13921, #11641, #4977, #18507, #11786, #26786, #702, #5114, #20509, #9660, #9522, #5257, #22930, #3391, #18221, #9375, #22649, #13643, #18363, #27070, #13779, #16360, #2966, #849, #7521, #11927, #25060, #14621, #12756, #3813, #12344, #12473, #1550, #25475, #14894, #25746, #10202, #14348, #23338, #6228, #21199, #19049, #16500, #19193, #23205, #19330, #25195, #14488, #16907, #1682, #21477, #10342, #21061, #23615, #25332, #23476, #27895, #23063, #1409, #4091, #27757, #1955, #16640, #3541, #7810, #8217, #8356, #18780, #17042, #25604, #6089, #1819, #14756, #10625, #5682, #3955, #12615, #12198, #20926 ),
 .UNSPECIFIED., .F., .F. ) 
 B_SPLINE_CURVE_WITH_KNOTS ( ( 3, 2, 2, 2, 2, 2, 2, 2, 2, 2, 2, 2, 2, 2, 2, 2, 2, 2, 2, 2, 2, 2, 2, 2, 2, 2, 2, 2, 2, 2, 2, 2, 2, 2, 2, 2, 2, 2, 2, 2, 2, 2, 2, 2, 2, 2, 3 ),
 ( 0.4779971559588572227, 0.4791666666666666852, 0.4895833333333333148, 0.5000000000000000000, 0.5104166666666666297, 0.5208333333333333703, 0.5312500000000000000, 0.5416666666666666297, 0.5520833333333333703, 0.5625000000000000000, 0.5729166666666666297, 0.5833333333333333703, 0.5937500000000000000, 0.6041666666666666297, 0.6145833333333333703, 0.6250000000000000000, 0.6354166666666666297, 0.6458333333333333703, 0.6562500000000000000, 0.6666666666666666297, 0.6770833333333333703, 0.6875000000000000000, 0.6979166666666666297, 0.7083333333333333703, 0.7187500000000000000, 0.7291666666666666297, 0.7395833333333333703, 0.7500000000000000000, 0.7604166666666666297, 0.7708333333333333703, 0.7812500000000000000, 0.7916666666666666297, 0.8020833333333333703, 0.8125000000000000000, 0.8229166666666666297, 0.8333333333333333703, 0.8437500000000000000, 0.8541666666666666297, 0.8645833333333333703, 0.8750000000000000000, 0.8854166666666666297, 0.8958333333333333703, 0.9062500000000000000, 0.9166666666666665186, 0.9270833333333333703, 0.9375000000000000000, 0.9448586970929392370 ),
 .UNSPECIFIED. ) 
 CURVE ( )  GEOMETRIC_REPRESENTATION_ITEM ( )  RATIONAL_B_SPLINE_CURVE ( ( 0.9848264816800302857, 0.9914537246260948233, 1.000000000000000000, 0.9238795325112867385, 1.000000000000000000, 0.9238795325112867385, 1.000000000000000000, 0.9238795325112867385, 1.000000000000000000, 0.9238795325112867385, 1.000000000000000000, 0.9238795325112867385, 1.000000000000000000, 0.9238795325112867385, 1.000000000000000000, 0.9238795325112867385, 1.000000000000000000, 0.9238795325112867385, 1.000000000000000000, 0.9238795325112867385, 1.000000000000000000, 0.9238795325112867385, 1.000000000000000000, 0.9238795325112867385, 1.000000000000000000, 0.9238795325112867385, 1.000000000000000000, 0.9238795325112867385, 1.000000000000000000, 0.9238795325112867385, 1.000000000000000000, 0.9238795325112867385, 1.000000000000000000, 0.9238795325112867385, 1.000000000000000000, 0.9238795325112867385, 1.000000000000000000, 0.9238795325112867385, 1.000000000000000000, 0.9238795325112867385, 1.000000000000000000, 0.9238795325112867385, 1.000000000000000000, 0.9238795325112867385, 1.000000000000000000, 0.9238795325112867385, 1.000000000000000000, 0.9238795325112867385, 1.000000000000000000, 0.9238795325112867385, 1.000000000000000000, 0.9238795325112867385, 1.000000000000000000, 0.9238795325112867385, 1.000000000000000000, 0.9238795325112867385, 1.000000000000000000, 0.9238795325112867385, 1.000000000000000000, 0.9238795325112867385, 1.000000000000000000, 0.9238795325112867385, 1.000000000000000000, 0.9238795325112867385, 1.000000000000000000, 0.9238795325112867385, 1.000000000000000000, 0.9238795325112867385, 1.000000000000000000, 0.9238795325112867385, 1.000000000000000000, 0.9238795325112867385, 1.000000000000000000, 0.9238795325112867385, 1.000000000000000000, 0.9238795325112867385, 1.000000000000000000, 0.9238795325112867385, 1.000000000000000000, 0.9238795325112867385, 1.000000000000000000, 0.9238795325112867385, 1.000000000000000000, 0.9238795325112867385, 1.000000000000000000, 0.9238795325112867385, 1.000000000000000000, 0.9238795325112867385, 1.000000000000000000, 0.9238795325112867385, 1.000000000000000000, 0.9462258435690522607, 0.9684275710300105366 ) ) 
 REPRESENTATION_ITEM ( '' )  );
#11326 = CARTESIAN_POINT ( 'NONE',  ( 95.00472066334982912, 116.8754121666685393, -45.42500000273119554 ) ) ;
#11327 = CARTESIAN_POINT ( 'NONE',  ( 13.14518615778179544, 37.77539062608393294, -1.609821015232357215E-15 ) ) ;
#11328 = CARTESIAN_POINT ( 'NONE',  ( 104.3262379212492590, 115.9545556584642867, -49.20000000546237828 ) ) ;
#11329 = CARTESIAN_POINT ( 'NONE',  ( 6.873508243573242638, 51.14166184781125679, 15.00000000000065548 ) ) ;
#11330 = CARTESIAN_POINT ( 'NONE',  ( 99.99999999999997158, 117.3602355696678643, -49.50000000000001421 ) ) ;
#11331 = CARTESIAN_POINT ( 'NONE',  ( 124.3771271284221314, 36.88242187499999858, -13.57481594606304753 ) ) ;
#11332 = ORIENTED_EDGE ( 'NONE', *, *, #14922, .F. ) ;
#11333 = ORIENTED_EDGE ( 'NONE', *, *, #13179, .T. ) ;
#11334 = PLANE ( 'NONE',  #7189 ) ;
#11335 = CARTESIAN_POINT ( 'NONE',  ( -13.14518615778179544, 36.78320312608393294, 0.000000000000000000 ) ) ;
#11336 = CARTESIAN_POINT ( 'NONE',  ( -13.57481594606304576, 37.97382812716787726, 5.622872871577880183 ) ) ;
#11337 = CARTESIAN_POINT ( 'NONE',  ( 104.9999999999999574, 2.071067811865491937, 9.687500002731184168 ) ) ;
#11338 = CARTESIAN_POINT ( 'NONE',  ( 130.0000000000000000, 34.00507812608393721, -13.14518615778179544 ) ) ;
#11339 = CARTESIAN_POINT ( 'NONE',  ( 65.00000000000000000, 35.34453125216787583, -13.57481594606304576 ) ) ;
#11340 = CARTESIAN_POINT ( 'NONE',  ( 97.92893218813451028, 5.000000000000018652, 14.81249999999999822 ) ) ;
#11341 = CARTESIAN_POINT ( 'NONE',  ( -13.57481594606304576, 31.62382812716787228, 5.622872871577880183 ) ) ;
#11342 = STYLED_ITEM ( 'NONE', ( #748 ), #7835 ) ;
#11343 = CARTESIAN_POINT ( 'NONE',  ( 94.99999999999995737, 1.387778780781445676E-14, 2.999999999999999112 ) ) ;
#11344 = DIRECTION ( 'NONE',  ( -1.156482317317871478E-16, 0.000000000000000000, -1.000000000000000000 ) ) ;
#11345 = CARTESIAN_POINT ( 'NONE',  ( 0.000000000000000000, 21.95886589889650509, 0.000000000000000000 ) ) ;
#11346 = CARTESIAN_POINT ( 'NONE',  ( 208.1451861577817795, 32.96328125108393436, 5.444914386472293977 ) ) ;
#11347 = CARTESIAN_POINT ( 'NONE',  ( 2.493653234604083739E-15, 31.77265625216787370, 13.57481594606304576 ) ) ;
#11348 = CARTESIAN_POINT ( 'NONE',  ( 99.99999999999995737, 85.00000000000000000, -1.387778780781445676E-14 ) ) ;
#11349 = CARTESIAN_POINT ( 'NONE',  ( 108.0825317500000153, 110.0000000000000000, -54.37500000273119838 ) ) ;
#11350 = CARTESIAN_POINT ( 'NONE',  ( 95.00000000000000000, 94.37499999726881583, -7.551217303480904118E-15 ) ) ;
#11351 = LINE ( 'NONE', #13344, #9044 ) ;
#11352 = CARTESIAN_POINT ( 'NONE',  ( 107.0000000000000000, 110.0000000000000000, -145.0000000000000284 ) ) ;
#11353 = CARTESIAN_POINT ( 'NONE',  ( -5.622872871577873077, 38.76757812500000000, 13.57481594606304753 ) ) ;
#11354 = CARTESIAN_POINT ( 'NONE',  ( -0.1722897647759079331, 36.00000000000000000, -13.51468191220838122 ) ) ;
#11355 = CARTESIAN_POINT ( 'NONE',  ( 9.295050272127047819, 35.49335937608393721, 9.295050272127046043 ) ) ;
#11356 = CARTESIAN_POINT ( 'NONE',  ( 5.444914386472297529, 35.54296875108393294, -13.14518615778179900 ) ) ;
#11357 = CARTESIAN_POINT ( 'NONE',  ( 185.4011555911795597, 35.54296874999999289, 9.598844408820459861 ) ) ;
#11358 = CARTESIAN_POINT ( 'NONE',  ( -8.312177448680279460E-16, 36.93203125216787441, -13.57481594606304576 ) ) ;
#11359 = CARTESIAN_POINT ( 'NONE',  ( 92.99999999999998579, 110.0000000000000000, -48.49999999453763877 ) ) ;
#11360 = DIRECTION ( 'NONE',  ( -0.000000000000000000, -1.000000000000000000, -0.000000000000000000 ) ) ;
#11361 = CARTESIAN_POINT ( 'NONE',  ( 78.14518615778179367, 37.03125000108393294, -5.444914386472297529 ) ) ;
#11362 = CARTESIAN_POINT ( 'NONE',  ( 104.4587341249999781, 1.846868145590750521, 2.000000001365591640 ) ) ;
#11363 = CARTESIAN_POINT ( 'NONE',  ( 97.95371496370606224, 123.0000000000000000, -1.465530591365614477 ) ) ;
#11364 =( BOUNDED_CURVE ( )  B_SPLINE_CURVE ( 2, ( #10671, #11870, #14948, #9882, #25939, #3199, #12522, #19104, #18590 ),
 .UNSPECIFIED., .F., .T. ) 
 B_SPLINE_CURVE_WITH_KNOTS ( ( 3, 2, 2, 2, 3 ),
 ( 0.2708333333333330928, 0.2812499999999998890, 0.2916666666666666852, 0.3020833333333334259, 0.3125000000000002220 ),
 .UNSPECIFIED. ) 
 CURVE ( )  GEOMETRIC_REPRESENTATION_ITEM ( )  RATIONAL_B_SPLINE_CURVE ( ( 1.000000000000001554, 0.9238795325112850731, 1.000000000000000000, 0.9238795325112867385, 1.000000000000000000, 0.9238795325112867385, 1.000000000000000000, 0.9238795325112850731, 1.000000000000001554 ) ) 
 REPRESENTATION_ITEM ( '' )  );
#11365 = EDGE_LOOP ( 'NONE', ( #20900, #18799, #18302, #5653 ) ) ;
#11366 = CARTESIAN_POINT ( 'NONE',  ( 98.95673454514873413, 123.0000000000000426, -1.805156233539860100 ) ) ;
#11367 = CARTESIAN_POINT ( 'NONE',  ( 5.622872871577871301, 35.98945312499999716, -13.57481594606304753 ) ) ;
#11368 = CARTESIAN_POINT ( 'NONE',  ( 135.4449143864723055, 37.82500000108392868, 13.14518615778179189 ) ) ;
#11369 = ORIENTED_EDGE ( 'NONE', *, *, #3399, .T. ) ;
#11370 = CARTESIAN_POINT ( 'NONE',  ( 96.46446609406721961, 80.12500000000000000, 3.535533905932727539 ) ) ;
#11371 = VECTOR ( 'NONE', #16744, 1000.000000000000000 ) ;
#11372 = CARTESIAN_POINT ( 'NONE',  ( 99.99999999999995737, 85.00000000000000000, -1.387778780781445676E-14 ) ) ;
#11373 = CARTESIAN_POINT ( 'NONE',  ( 94.99999999999995737, 82.12500000273119838, -1.387778780781445676E-14 ) ) ;
#11374 = CARTESIAN_POINT ( 'NONE',  ( 103.5355339059327235, 92.87500000000000000, 3.535533905932724874 ) ) ;
#11375 = CARTESIAN_POINT ( 'NONE',  ( 56.33088789466297186, 36.00000000000002842, -10.16963847934322906 ) ) ;
#11376 = ADVANCED_FACE ( 'NONE', ( #10238 ), #23512, .F. ) ;
#11377 = CIRCLE ( 'NONE', #25960, 5.000000000000004441 ) ;
#11378 = CARTESIAN_POINT ( 'NONE',  ( 105.6631189606246295, 105.8855032339526758, -50.20000000000001705 ) ) ;
#11379 = CARTESIAN_POINT ( 'NONE',  ( 70.44491438647230552, 33.06250000108393294, 13.14518615778179189 ) ) ;
#11380 = ORIENTED_EDGE ( 'NONE', *, *, #8087, .F. ) ;
#11381 = DIRECTION ( 'NONE',  ( 0.000000000000000000, 1.000000000000000000, 0.000000000000000000 ) ) ;
#11382 = CARTESIAN_POINT ( 'NONE',  ( 94.99999999999995737, -2.071067811865466624, 13.06250000000000000 ) ) ;
#11383 = ORIENTED_EDGE ( 'NONE', *, *, #23409, .T. ) ;
#11384 = CARTESIAN_POINT ( 'NONE',  ( -8.049105076161786076E-16, 37.37851562608393863, -13.14518615778179544 ) ) ;
#11385 = CARTESIAN_POINT ( 'NONE',  ( 208.5748159460630688, 35.14609375216787157, -1.662435489736055892E-15 ) ) ;
#11386 = ORIENTED_EDGE ( 'NONE', *, *, #17480, .F. ) ;
#11387 = EDGE_CURVE ( 'NONE', #9857, #23574, #22429, .T. ) ;
#11388 = CARTESIAN_POINT ( 'NONE',  ( -8.049105076161786076E-16, 33.21132812608393436, -13.14518615778179544 ) ) ;
#11389 = DIRECTION ( 'NONE',  ( -0.000000000000000000, 1.000000000000000000, -0.000000000000000000 ) ) ;
#11390 = DIRECTION ( 'NONE',  ( 1.000000000000000000, 0.000000000000000000, -5.782411586589357392E-17 ) ) ;
#11392 = AXIS2_PLACEMENT_3D ( 'NONE', #14965, #17256, #21412 ) ;
#11391 = CARTESIAN_POINT ( 'NONE',  ( -5.444914386472299306, 33.75703125108393721, 13.14518615778179722 ) ) ;
#11393 = ADVANCED_FACE ( 'NONE', ( #19087 ), #27795, .T. ) ;
#11394 = FACE_OUTER_BOUND ( 'NONE', #10710, .T. ) ;
#11395 = CARTESIAN_POINT ( 'NONE',  ( 59.37712712842213136, 34.79882812499998579, 13.57481594606304753 ) ) ;
#11396 = CYLINDRICAL_SURFACE ( 'NONE', #6380, 13.57481594606304576 ) ;
#11397 = CARTESIAN_POINT ( 'NONE',  ( 101.8468681455906903, -4.458734124999987891, 12.00000000136559208 ) ) ;
#11398 = DIRECTION ( 'NONE',  ( 0.000000000000000000, 0.000000000000000000, -1.000000000000000000 ) ) ;
#11399 = CARTESIAN_POINT ( 'NONE',  ( 95.54126587499996504, 1.387778780781445676E-14, 14.43750000136559208 ) ) ;
#11400 = CARTESIAN_POINT ( 'NONE',  ( 95.67376207875072680, 115.9545556584642867, -52.80000000546237260 ) ) ;
#11401 = CARTESIAN_POINT ( 'NONE',  ( 98.15313185440925281, 90.87499999863439371, -4.458734124999994997 ) ) ;
#11402 = CARTESIAN_POINT ( 'NONE',  ( 107.0000000000000000, 110.0000000000000000, -54.00000000000001421 ) ) ;
#11403 = CARTESIAN_POINT ( 'NONE',  ( 108.0825317500000011, 110.0000000000000000, -50.62499999726882294 ) ) ;
#11404 = CARTESIAN_POINT ( 'NONE',  ( 13.14518615778179900, 37.22968750108393721, -5.444914386472297529 ) ) ;
#11405 = EDGE_CURVE ( 'NONE', #22871, #20179, #10745, .T. ) ;
#11406 = ORIENTED_EDGE ( 'NONE', *, *, #17196, .F. ) ;
#11407 = DIRECTION ( 'NONE',  ( 0.000000000000000000, 1.000000000000000000, 0.000000000000000000 ) ) ;
#11408 = CARTESIAN_POINT ( 'NONE',  ( 97.92893218813451028, -4.999999999999989342, 1.187499999999999334 ) ) ;
#11409 = VECTOR ( 'NONE', #26779, 1000.000000000000000 ) ;
#11410 = CARTESIAN_POINT ( 'NONE',  ( 204.2950502721270425, 34.50117187608393010, 9.295050272127046043 ) ) ;
#11411 = ORIENTED_EDGE ( 'NONE', *, *, #1492, .F. ) ;
#11412 = CARTESIAN_POINT ( 'NONE',  ( 203.7583343923459154, 50.00000000000000000, -10.38725784494393345 ) ) ;
#11413 = CARTESIAN_POINT ( 'NONE',  ( 96.84719886470459471, 3.152801135295383084, 11.56250000136559208 ) ) ;
#11414 = EDGE_CURVE ( 'NONE', #8614, #10542, #7856, .T. ) ;
#11415 = ORIENTED_EDGE ( 'NONE', *, *, #28113, .F. ) ;
#11416 = CARTESIAN_POINT ( 'NONE',  ( 95.67376207875072680, 104.0454443415356991, -45.70000000000000995 ) ) ;
#11417 = CARTESIAN_POINT ( 'NONE',  ( 9.295050272127047819, 35.29492187608393294, 9.295050272127046043 ) ) ;
#11418 = CARTESIAN_POINT ( 'NONE',  ( 98.96446609406727646, 123.5499999999999972, 2.499999999999977796 ) ) ;
#11419 = CARTESIAN_POINT ( 'NONE',  ( 130.0000000000000000, 39.95820312608393010, 13.14518615778179544 ) ) ;
#11420 = LINE ( 'NONE', #7010, #7988 ) ;
#11421 = CARTESIAN_POINT ( 'NONE',  ( -9.295050272127046043, 35.69179687608393436, -9.295050272127046043 ) ) ;
#11422 = ADVANCED_FACE ( 'NONE', ( #9230 ), #10947, .T. ) ;
#11423 = CARTESIAN_POINT ( 'NONE',  ( 95.00000000000000000, 95.37499999726881583, -7.551217303480904118E-15 ) ) ;
#11424 = CARTESIAN_POINT ( 'NONE',  ( 78.14518615778179367, 38.76757812608393294, -1.609821015232357215E-15 ) ) ;
#11425 = CARTESIAN_POINT ( 'NONE',  ( 72.11549039185503318, 49.99999999945668350, -11.58166858714116998 ) ) ;
#11426 = CARTESIAN_POINT ( 'NONE',  ( 91.91746824999999887, 110.0000000000000000, -49.37500000273119838 ) ) ;
#11427 = EDGE_CURVE ( 'NONE', #23060, #5791, #15442, .T. ) ;
#11428 = CARTESIAN_POINT ( 'NONE',  ( 201.9444236247691720, 31.75150628229955529, -11.16113343896966370 ) ) ;
#11429 = CARTESIAN_POINT ( 'NONE',  ( 77.07727640983618755, 35.99999999999999289, -6.197985357348143154 ) ) ;
#11430 = CARTESIAN_POINT ( 'NONE',  ( 9.295050272127047819, 37.08085937608393579, 9.295050272127046043 ) ) ;
#11431 = CARTESIAN_POINT ( 'NONE',  ( 95.54126587499996504, -1.846868145590724986, 8.750000001365592084 ) ) ;
#11432 = CARTESIAN_POINT ( 'NONE',  ( 66.13716782454086740, 35.99999999999998579, 13.09590655363602707 ) ) ;
#11433 = CARTESIAN_POINT ( 'NONE',  ( 55.40115559117954547, 38.71796874999999716, 9.598844408820459861 ) ) ;
#11434 = CARTESIAN_POINT ( 'NONE',  ( 200.4449143864723055, 36.83281250108392868, 13.14518615778179189 ) ) ;
#11435 = ORIENTED_EDGE ( 'NONE', *, *, #5863, .T. ) ;
#11436 = CARTESIAN_POINT ( 'NONE',  ( 5.444914386472302859, 38.61875000108392442, 13.14518615778179189 ) ) ;
#11437 = CARTESIAN_POINT ( 'NONE',  ( 98.96446609406724804, 124.8499999999999943, -2.500000000000008438 ) ) ;
#11438 = CARTESIAN_POINT ( 'NONE',  ( 204.2950502721270425, 36.48554687608393721, -9.295050272127046043 ) ) ;
#11439 = CARTESIAN_POINT ( 'NONE',  ( 102.4976396683250783, 117.6869444889999841, -46.47499999726882436 ) ) ;
#11440 = ORIENTED_EDGE ( 'NONE', *, *, #8464, .T. ) ;
#11441 = CARTESIAN_POINT ( 'NONE',  ( -5.622872871577873077, 32.11992187499999574, -13.57481594606304753 ) ) ;
#11442 = CARTESIAN_POINT ( 'NONE',  ( -13.14518615778179544, 33.40976562608393863, 0.000000000000000000 ) ) ;
#11443 = ORIENTED_EDGE ( 'NONE', *, *, #6166, .F. ) ;
#11444 = CARTESIAN_POINT ( 'NONE',  ( 135.4449143864723055, 34.15390625108393863, -13.14518615778179900 ) ) ;
#11445 = CARTESIAN_POINT ( 'NONE',  ( 2.816687638038913930E-15, 20.53589838486225361, -23.00000000000001421 ) ) ;
#11446 = CARTESIAN_POINT ( 'NONE',  ( 181.8548138422182205, 35.19570312608393436, 0.000000000000000000 ) ) ;
#11447 = ORIENTED_EDGE ( 'NONE', *, *, #19485, .T. ) ;
#11448 = CARTESIAN_POINT ( 'NONE',  ( 99.14382582708708469, 123.1000000010924822, 2.066987299999979655 ) ) ;
#11449 = CARTESIAN_POINT ( 'NONE',  ( 4.062583540575953833, 50.00000000116115473, -12.98908657125259580 ) ) ;
#11450 = CARTESIAN_POINT ( 'NONE',  ( 99.99999999999998579, 110.0000000000000000, 15.00099999999999412 ) ) ;
#11451 =( BOUNDED_CURVE ( )  B_SPLINE_CURVE ( 2, ( #633, #11859, #11433, #5332, #1064, #7162, #17866, #4909, #20581 ),
 .UNSPECIFIED., .F., .F. ) 
 B_SPLINE_CURVE_WITH_KNOTS ( ( 3, 2, 2, 2, 3 ),
 ( 0.2291666666666665741, 0.2395833333333332316, 0.2499999999999998335, 0.2604166666666665186, 0.2708333333333330928 ),
 .UNSPECIFIED. ) 
 CURVE ( )  GEOMETRIC_REPRESENTATION_ITEM ( )  RATIONAL_B_SPLINE_CURVE ( ( 1.000000000000000666, 0.9238795325112861834, 1.000000000000000000, 0.9238795325112867385, 1.000000000000000000, 0.9238795325112867385, 1.000000000000000000, 0.9238795325112884038, 0.9999999999999983347 ) ) 
 REPRESENTATION_ITEM ( '' )  );
#11452 = CARTESIAN_POINT ( 'NONE',  ( 78.57481594606305464, 40.60312499999999858, -1.662435489736055892E-15 ) ) ;
#11453 = CARTESIAN_POINT ( 'NONE',  ( 106.5389055433251002, 114.7507929638356785, -49.92500000273119554 ) ) ;
#11454 = LINE ( 'NONE', #801, #6083 ) ;
#11455 = CARTESIAN_POINT ( 'NONE',  ( 94.99999999999995737, 1.387778780781445676E-14, 6.999999999999999112 ) ) ;
#11456 = CARTESIAN_POINT ( 'NONE',  ( 72.62196353419399486, 54.91641323977498246, 14.99999999999997868 ) ) ;
#11457 = ORIENTED_EDGE ( 'NONE', *, *, #288, .T. ) ;
#11458 = SURFACE_SIDE_STYLE ('',( #15601 ) ) ;
#11459 = CARTESIAN_POINT ( 'NONE',  ( 101.8468681455906903, 4.458734125000016313, 6.125000001365591196 ) ) ;
#11460 = ORIENTED_EDGE ( 'NONE', *, *, #7622, .F. ) ;
#11461 = CARTESIAN_POINT ( 'NONE',  ( 102.4999999999999858, 123.1000000021849416, -9.847140817659276890E-15 ) ) ;
#11462 = CARTESIAN_POINT ( 'NONE',  ( 95.54126587499996504, 1.387778780781445676E-14, 6.437500001365592084 ) ) ;
#11463 = CARTESIAN_POINT ( 'NONE',  ( 138.2596115288800434, 50.00000000056351723, 10.79618466886582340 ) ) ;
#11464 = CARTESIAN_POINT ( 'NONE',  ( -13.14518615778179189, 36.63437500108393152, 5.444914386472304635 ) ) ;
#11465 = CARTESIAN_POINT ( 'NONE',  ( -13.05838185645087357, 36.00000000000000000, 1.569311539113920739 ) ) ;
#11466 = FACE_OUTER_BOUND ( 'NONE', #6109, .T. ) ;
#11467 = CARTESIAN_POINT ( 'NONE',  ( 101.8468681455907330, 92.49999999863442213, -4.458734124999994997 ) ) ;
#11468 = FACE_OUTER_BOUND ( 'NONE', #17812, .T. ) ;
#11469 = CARTESIAN_POINT ( 'NONE',  ( -13.14518615778179722, 36.53515625108393294, -5.444914386472297529 ) ) ;
#11470 = DIRECTION ( 'NONE',  ( -0.000000000000000000, 1.000000000000000000, -0.000000000000000000 ) ) ;
#11471 = CARTESIAN_POINT ( 'NONE',  ( -9.180175813647995398, 55.00000000000000711, 14.99999999999999822 ) ) ;
#11472 = CARTESIAN_POINT ( 'NONE',  ( 102.0710678118654613, 91.68749999726881583, 4.999999999999983125 ) ) ;
#11473 = CARTESIAN_POINT ( 'NONE',  ( 130.0000000000000000, 36.03906250000000000, -13.57481594606304576 ) ) ;
#11474 = ORIENTED_EDGE ( 'NONE', *, *, #5547, .F. ) ;
#11475 = AXIS2_PLACEMENT_3D ( 'NONE', #1127, #18065, #11922 ) ;
#11476 = ORIENTED_EDGE ( 'NONE', *, *, #4634, .T. ) ;
#11477 = CARTESIAN_POINT ( 'NONE',  ( 99.99999999999997158, 117.3602355696678643, -51.50000000000001421 ) ) ;
#11478 = CARTESIAN_POINT ( 'NONE',  ( -9.295050272127044266, 32.11992187608393579, 9.295050272127047819 ) ) ;
#11479 = CARTESIAN_POINT ( 'NONE',  ( -9.598844408820454532, 34.05468750216788010, 9.598844408820459861 ) ) ;
#11480 = CARTESIAN_POINT ( 'NONE',  ( 97.92893218813451028, -4.999999999999989342, 10.31250000273118594 ) ) ;
#11481 = CARTESIAN_POINT ( 'NONE',  ( 116.8548138422182205, 32.61601562608393579, 0.000000000000000000 ) ) ;
#11482 = CARTESIAN_POINT ( 'NONE',  ( 74.29505027212704249, 39.26367187608393294, 9.295050272127046043 ) ) ;
#11483 = CARTESIAN_POINT ( 'NONE',  ( 103.5355339059327093, 80.62500000000000000, -3.535533905932755072 ) ) ;
#11484 = CARTESIAN_POINT ( 'NONE',  ( 9.598844408820456309, 32.07031250216787299, -9.598844408820458085 ) ) ;
#11485 = DIRECTION ( 'NONE',  ( -1.000000000000000000, 0.000000000000000000, 3.469446951953615175E-16 ) ) ;
#11486 = CARTESIAN_POINT ( 'NONE',  ( 108.0825317499999869, 112.6261737610028320, -46.77499999726882152 ) ) ;
#11487 = CARTESIAN_POINT ( 'NONE',  ( 9.598844408820456309, 38.42031250216787441, -9.598844408820458085 ) ) ;
#11488 = CARTESIAN_POINT ( 'NONE',  ( 208.1451861577817795, 35.44375000108393436, -5.444914386472297529 ) ) ;
#11489 = CARTESIAN_POINT ( 'NONE',  ( 94.99999999999995737, 1.387778780781445676E-14, 13.00000000000000000 ) ) ;
#11490 = CARTESIAN_POINT ( 'NONE',  ( 101.0355339059327378, 124.4569999999781515, 2.499999999999977796 ) ) ;
#11491 = PRESENTATION_STYLE_ASSIGNMENT (( #13633 ) ) ;
#11492 = CARTESIAN_POINT ( 'NONE',  ( 97.92893218813448186, 94.18749999726881583, -4.999999999999963585 ) ) ;
#11493 =( BOUNDED_CURVE ( )  B_SPLINE_CURVE ( 2, ( #9830, #13810, #7119, #24523, #24805, #1023, #5145, #15954, #27241 ),
 .UNSPECIFIED., .F., .F. ) 
 B_SPLINE_CURVE_WITH_KNOTS ( ( 3, 2, 2, 2, 3 ),
 ( 0.8214285714285713969, 0.8303571428571429047, 0.8392857142857143016, 0.8482142857142856984, 0.8571428571428570953 ),
 .UNSPECIFIED. ) 
 CURVE ( )  GEOMETRIC_REPRESENTATION_ITEM ( )  RATIONAL_B_SPLINE_CURVE ( ( 1.000000000000000000, 0.9238795325112867385, 1.000000000000000000, 0.9238795325112867385, 1.000000000000000000, 0.9238795325112867385, 1.000000000000000000, 0.9238795325112867385, 1.000000000000000000 ) ) 
 REPRESENTATION_ITEM ( '' )  );
#11494 = DIRECTION ( 'NONE',  ( 0.000000000000000000, 0.000000000000000000, -1.000000000000000000 ) ) ;
#11495 = CARTESIAN_POINT ( 'NONE',  ( 97.93301270000000613, 124.7500000010924737, -9.540979117872439019E-15 ) ) ;
#11496 = CARTESIAN_POINT ( 'NONE',  ( 9.598844408820459861, 34.15390624999999858, 9.598844408820456309 ) ) ;
#11497 = CARTESIAN_POINT ( 'NONE',  ( -7.228014483236695816E-17, 80.00000000000000000, -9.999999999999998224 ) ) ;
#11498 = CARTESIAN_POINT ( 'NONE',  ( 13.14518615778179900, 34.84843750108393579, -5.444914386472297529 ) ) ;
#11499 = CARTESIAN_POINT ( 'NONE',  ( 13.14518615778179544, 36.98164062608393010, -1.609821015232357215E-15 ) ) ;
#11500 = CARTESIAN_POINT ( 'NONE',  ( 208.5748159460630120, 32.71523437500000142, -5.622872871577873077 ) ) ;
#11501 = CARTESIAN_POINT ( 'NONE',  ( 5.622872871577878406, 34.99726562716787726, 13.57481594606304576 ) ) ;
#11502 = DIRECTION ( 'NONE',  ( 0.000000000000000000, 0.000000000000000000, -1.000000000000000000 ) ) ;
#11503 = CARTESIAN_POINT ( 'NONE',  ( 104.4587341249999781, 82.00000000136560629, -1.846868145590750299 ) ) ;
#11504 = CARTESIAN_POINT ( 'NONE',  ( 78.14518615778179367, 36.23750000108393010, -5.444914386472297529 ) ) ;
#11505 = CARTESIAN_POINT ( 'NONE',  ( 102.4976396683250925, 102.3130555110000159, -52.77500000273119696 ) ) ;
#11506 = CARTESIAN_POINT ( 'NONE',  ( 98.84711739976860656, 122.9999999999999574, 2.236958744467042237 ) ) ;
#11507 = CARTESIAN_POINT ( 'NONE',  ( 13.57481594606304931, 37.37851562499999858, 5.622872871577868636 ) ) ;
#11508 = CARTESIAN_POINT ( 'NONE',  ( -9.598844408820454532, 33.16171874999999858, 9.598844408820459861 ) ) ;
#11509 = CARTESIAN_POINT ( 'NONE',  ( 116.8548138422182205, 36.78320312608393294, 0.000000000000000000 ) ) ;
#11510 = ORIENTED_EDGE ( 'NONE', *, *, #8481, .T. ) ;
#11511 = CYLINDRICAL_SURFACE ( 'NONE', #12706, 7.000000000000006217 ) ;
#11512 = EDGE_CURVE ( 'NONE', #26308, #3039, #20500, .T. ) ;
#11513 = CARTESIAN_POINT ( 'NONE',  ( 95.00000000000000000, 94.56250000000000000, 2.071067811865463959 ) ) ;
#11514 = CARTESIAN_POINT ( 'NONE',  ( 101.8468681455906903, 83.12500000136560629, -4.458734125000016313 ) ) ;
#11515 = CARTESIAN_POINT ( 'NONE',  ( 99.99999999999998579, 92.25000000000000000, -4.999999999999997335 ) ) ;
#11516 = CARTESIAN_POINT ( 'NONE',  ( 2.493653234604083739E-15, 34.05468749999999289, 13.57481594606304576 ) ) ;
#11517 = CARTESIAN_POINT ( 'NONE',  ( 108.0825317499999869, 107.3738262389971538, -46.72499999726881015 ) ) ;
#11518 = CARTESIAN_POINT ( 'NONE',  ( 65.00000000000000000, 31.82226562608393650, -13.14518615778179544 ) ) ;
#11519 = ORIENTED_EDGE ( 'NONE', *, *, #3475, .T. ) ;
#11520 = CARTESIAN_POINT ( 'NONE',  ( 9.598844408820459861, 32.66562500216787157, 9.598844408820456309 ) ) ;
#11521 = CARTESIAN_POINT ( 'NONE',  ( 104.9999999999999716, 1.449011120738813565E-14, 13.50000000000000000 ) ) ;
#11522 = ORIENTED_EDGE ( 'NONE', *, *, #21171, .T. ) ;
#11523 = CARTESIAN_POINT ( 'NONE',  ( -5.444914386472297529, 35.84062500108394289, -13.14518615778179900 ) ) ;
#11524 = CARTESIAN_POINT ( 'NONE',  ( 185.4011555911795313, 33.85625000216787583, -9.598844408820458085 ) ) ;
#11525 = ORIENTED_EDGE ( 'NONE', *, *, #1184, .F. ) ;
#11526 = CARTESIAN_POINT ( 'NONE',  ( 2.414731522848535132E-15, 32.81445312608393294, 13.14518615778179544 ) ) ;
#11527 = FACE_OUTER_BOUND ( 'NONE', #20209, .T. ) ;
#11528 = CARTESIAN_POINT ( 'NONE',  ( -8.312177448680279460E-16, 34.45156249999999432, -13.57481594606304576 ) ) ;
#11529 = CARTESIAN_POINT ( 'NONE',  ( -5.444914386472297529, 35.04687500108393294, -13.14518615778179900 ) ) ;
#11530 = CARTESIAN_POINT ( 'NONE',  ( 143.1451861577818079, 32.21914062608393436, -1.609821015232357215E-15 ) ) ;
#11531 = CARTESIAN_POINT ( 'NONE',  ( 95.54126587499999346, 91.74999999863439371, -1.846868145590737864 ) ) ;
#11532 =( BOUNDED_CURVE ( )  B_SPLINE_CURVE ( 2, ( #13809, #24375, #13378, #15381, #2999, #4864, #6979, #13232, #2859 ),
 .UNSPECIFIED., .F., .F. ) 
 B_SPLINE_CURVE_WITH_KNOTS ( ( 3, 2, 2, 2, 3 ),
 ( 0.8958333333333335924, 0.9062500000000002220, 0.9166666666666667407, 0.9270833333333334814, 0.9375000000000000000 ),
 .UNSPECIFIED. ) 
 CURVE ( )  GEOMETRIC_REPRESENTATION_ITEM ( )  RATIONAL_B_SPLINE_CURVE ( ( 0.9999999999999983347, 0.9238795325112884038, 1.000000000000000000, 0.9238795325112867385, 1.000000000000000000, 0.9238795325112867385, 1.000000000000000000, 0.9238795325112867385, 1.000000000000000000 ) ) 
 REPRESENTATION_ITEM ( '' )  );
#11533 = CARTESIAN_POINT ( 'NONE',  ( 98.53841926354351699, 124.6500000010924651, -1.461580736456474794 ) ) ;
#11534 = CARTESIAN_POINT ( 'NONE',  ( 65.00000000000000000, 36.93203125216787441, -13.57481594606304576 ) ) ;
#11535 = CARTESIAN_POINT ( 'NONE',  ( 96.84719886470459471, 3.152801135295383084, 6.562500001365592084 ) ) ;
#11537 = LINE ( 'NONE', #20252, #6235 ) ;
#11536 = VECTOR ( 'NONE', #19322, 1000.000000000000000 ) ;
#11538 = CARTESIAN_POINT ( 'NONE',  ( 96.84719886470459471, 3.152801135295383084, 8.312500001365592084 ) ) ;
#11539 = CARTESIAN_POINT ( 'NONE',  ( 94.33688103937537051, 114.1144967660473242, -52.70000000546237828 ) ) ;
#11540 = CARTESIAN_POINT ( 'NONE',  ( 103.1528011352953484, 92.43749999863440792, 3.152801135295352886 ) ) ;
#11541 = CARTESIAN_POINT ( 'NONE',  ( 103.5355339059327093, 83.50000000273119838, 3.535533905932726206 ) ) ;
#11542 = DIRECTION ( 'NONE',  ( 1.000000000000000000, -0.000000000000000000, -7.228014483236696740E-18 ) ) ;
#11543 = CARTESIAN_POINT ( 'NONE',  ( 2.414731522848535132E-15, 33.80664062608393294, 13.14518615778179544 ) ) ;
#11544 = VERTEX_POINT ( 'NONE', #9650 ) ;
#11545 = CARTESIAN_POINT ( 'NONE',  ( 120.4011555911795455, 37.13046874999999147, 9.598844408820459861 ) ) ;
#11547 = ADVANCED_FACE ( 'NONE', ( #5535 ), #11667, .F. ) ;
#11546 = CARTESIAN_POINT ( 'NONE',  ( -13.57481594606304576, 37.82499999999999574, 0.000000000000000000 ) ) ;
#11548 = CARTESIAN_POINT ( 'NONE',  ( 103.5355339059327093, -3.535533905932726206, 1.374999999999999556 ) ) ;
#11549 = ADVANCED_FACE ( 'NONE', ( #2232 ), #17178, .T. ) ;
#11550 = CARTESIAN_POINT ( 'NONE',  ( 189.5550856135277229, 34.35234375108392868, 13.14518615778179722 ) ) ;
#11551 = ORIENTED_EDGE ( 'NONE', *, *, #18399, .T. ) ;
#11552 = CARTESIAN_POINT ( 'NONE',  ( 92.99999999999998579, 110.0000000000000000, -48.49999999453763877 ) ) ;
#11553 = CARTESIAN_POINT ( 'NONE',  ( 99.99999999999995737, 4.458734125000016313, 10.43750000136559208 ) ) ;
#11554 = VERTEX_POINT ( 'NONE', #19886 ) ;
#11555 = CARTESIAN_POINT ( 'NONE',  ( 91.91746824999998466, 112.6261737610028320, -51.47500000273119980 ) ) ;
#11556 = CARTESIAN_POINT ( 'NONE',  ( -5.444914386472299306, 35.14609375108393152, 13.14518615778179722 ) ) ;
#11557 = CYLINDRICAL_SURFACE ( 'NONE', #20837, 5.000000000000000888 ) ;
#11558 = EDGE_CURVE ( 'NONE', #12573, #15363, #2944, .T. ) ;
#11559 = CARTESIAN_POINT ( 'NONE',  ( 116.8548138422182205, 38.96601562608393721, 0.000000000000000000 ) ) ;
#11560 = CARTESIAN_POINT ( 'NONE',  ( 9.295050272127046043, 36.48554687608393721, -9.295050272127046043 ) ) ;
#11561 = CARTESIAN_POINT ( 'NONE',  ( 5.444914386472302859, 34.45156250108393436, 13.14518615778179189 ) ) ;
#11562 = CARTESIAN_POINT ( 'NONE',  ( 104.4587341249999781, 93.56249999863440792, -6.938893903907228378E-15 ) ) ;
#11563 = CARTESIAN_POINT ( 'NONE',  ( 58.88015637230197541, 51.28708186914660416, -14.99999999999791100 ) ) ;
#11564 = CARTESIAN_POINT ( 'NONE',  ( 99.99999999999998579, 118.4984768113314146, -51.87500000273119127 ) ) ;
#11565 = CARTESIAN_POINT ( 'NONE',  ( 189.3771271284221314, 40.05742187499999574, -13.57481594606304753 ) ) ;
#11566 = EDGE_LOOP ( 'NONE', ( #24322, #13753, #16173, #7201 ) ) ;
#11567 = CARTESIAN_POINT ( 'NONE',  ( 68.82956275799186585, 36.00000000000000711, 12.63428651647593703 ) ) ;
#11568 = VERTEX_POINT ( 'NONE', #2374 ) ;
#11569 = CARTESIAN_POINT ( 'NONE',  ( -8.049105076161786076E-16, 35.79101562608394005, -13.14518615778179544 ) ) ;
#11570 = CARTESIAN_POINT ( 'NONE',  ( 101.8468681455907046, 4.458734125000016313, 7.375000001365592084 ) ) ;
#11571 = CARTESIAN_POINT ( 'NONE',  ( 78.14518615778180788, 38.61875000108392442, -5.444914386472297529 ) ) ;
#11572 = EDGE_CURVE ( 'NONE', #14907, #26503, #18262, .T. ) ;
#11573 = CARTESIAN_POINT ( 'NONE',  ( 181.8548138422182205, 36.53515625108393294, -5.444914386472297529 ) ) ;
#11574 = CARTESIAN_POINT ( 'NONE',  ( 13.14518615778179722, 33.26093750108393721, -5.444914386472297529 ) ) ;
#11575 = CARTESIAN_POINT ( 'NONE',  ( 101.4615807364564546, 123.2500000010924879, 1.461580736456455476 ) ) ;
#11576 = CARTESIAN_POINT ( 'NONE',  ( 98.15313185440923860, 91.87499999863439371, -4.458734124999994997 ) ) ;
#11577 = CARTESIAN_POINT ( 'NONE',  ( 185.7049497278729575, 37.67617187608393436, 9.295050272127047819 ) ) ;
#11578 = CARTESIAN_POINT ( 'NONE',  ( 106.5389055433250860, 105.2492070361643215, -51.07499999726882578 ) ) ;
#11579 = ORIENTED_EDGE ( 'NONE', *, *, #23099, .T. ) ;
#11580 = CIRCLE ( 'NONE', #27110, 11.57481594606304398 ) ;
#11581 = CARTESIAN_POINT ( 'NONE',  ( -13.57481594606304753, 33.80664062500000000, -5.622872871577873077 ) ) ;
#11582 = CARTESIAN_POINT ( 'NONE',  ( 5.444914386472297529, 34.74921875108394431, -13.14518615778179900 ) ) ;
#11583 = VERTEX_POINT ( 'NONE', #22173 ) ;
#11584 = CARTESIAN_POINT ( 'NONE',  ( 130.0000000000000000, 32.61601562608393579, -13.14518615778179544 ) ) ;
#11585 = CARTESIAN_POINT ( 'NONE',  ( 65.00000000000000000, 36.83281249999999574, -13.57481594606304576 ) ) ;
#11586 = EDGE_CURVE ( 'NONE', #18466, #3788, #22317, .T. ) ;
#11587 = CARTESIAN_POINT ( 'NONE',  ( 200.4449143864723055, 32.56640625108394005, -13.14518615778179900 ) ) ;
#11588 = EDGE_LOOP ( 'NONE', ( #6863, #27028, #872, #70 ) ) ;
#11589 = CARTESIAN_POINT ( 'NONE',  ( 102.0669873000000081, 123.4000000010924794, -0.8561741729129508371 ) ) ;
#11590 = CARTESIAN_POINT ( 'NONE',  ( 95.00000000000000000, 91.31249999726880162, -2.071067811865479058 ) ) ;
#11591 = CARTESIAN_POINT ( 'NONE',  ( 94.99999999999997158, -2.071067811865486608, 5.187500002731184168 ) ) ;
#11592 = CARTESIAN_POINT ( 'NONE',  ( 143.5748159460630404, 36.78320312716786589, -5.622872871577873077 ) ) ;
#11593 = CARTESIAN_POINT ( 'NONE',  ( 99.99999999999998579, 118.4984768113314146, -45.62500000273119127 ) ) ;
#11594 = CARTESIAN_POINT ( 'NONE',  ( 97.92893218813451028, -4.999999999999989342, 2.312500002731185500 ) ) ;
#11595 = CARTESIAN_POINT ( 'NONE',  ( 99.99999999999998579, 90.00000000000000000, -6.938893903907228378E-15 ) ) ;
#11596 = CARTESIAN_POINT ( 'NONE',  ( 69.50488708631583279, 51.44650206077173493, 15.00000000000263611 ) ) ;
#11597 = CARTESIAN_POINT ( 'NONE',  ( 104.4587341249999639, 1.442382525525748735E-14, 4.937500001365592972 ) ) ;
#11598 = ORIENTED_EDGE ( 'NONE', *, *, #17878, .F. ) ;
#11599 = CARTESIAN_POINT ( 'NONE',  ( 94.99999999999997158, 2.071067811865503483, 13.06250000273118239 ) ) ;
#11600 = CARTESIAN_POINT ( 'NONE',  ( 96.84719886470459471, -3.152801135295355994, 6.562500001365592084 ) ) ;
#11601 = CARTESIAN_POINT ( 'NONE',  ( 134.8584992904650051, 49.99999999891522151, 12.70434618648776137 ) ) ;
#11602 = CARTESIAN_POINT ( 'NONE',  ( -13.14518615778179900, 36.53515625108392584, -5.444914386472297529 ) ) ;
#11603 = CARTESIAN_POINT ( 'NONE',  ( 0.000000000000000000, 36.00000000000000000, -13.57481594606304576 ) ) ;
#11604 = CARTESIAN_POINT ( 'NONE',  ( 51.85481384221820633, 32.07031250108393294, 5.444914386472304635 ) ) ;
#11605 = CARTESIAN_POINT ( 'NONE',  ( -8.312177448680279460E-16, 40.10703125216787157, -13.57481594606304576 ) ) ;
#11606 = CARTESIAN_POINT ( 'NONE',  ( 91.91746824999999887, 110.0000000000000000, -47.12500000273119838 ) ) ;
#11607 = CARTESIAN_POINT ( 'NONE',  ( 9.295050272127047819, 36.88242187608393152, 9.295050272127046043 ) ) ;
#11608 = AXIS2_PLACEMENT_3D ( 'NONE', #26831, #26396, #5158 ) ;
#11609 = DIRECTION ( 'NONE',  ( 0.000000000000000000, -1.000000000000000000, 0.000000000000000000 ) ) ;
#11610 = CARTESIAN_POINT ( 'NONE',  ( 2.529583995170619826, 49.99999999938378892, 13.34625891065936543 ) ) ;
#11611 = DIRECTION ( 'NONE',  ( -0.000000000000000000, -1.000000000000000000, -0.000000000000000000 ) ) ;
#11612 = CARTESIAN_POINT ( 'NONE',  ( 143.5748159460630404, 33.50898437499999716, -5.622872871577873077 ) ) ;
#11613 = ORIENTED_EDGE ( 'NONE', *, *, #368, .F. ) ;
#11614 = FACE_OUTER_BOUND ( 'NONE', #10758, .T. ) ;
#11615 = CARTESIAN_POINT ( 'NONE',  ( 5.444914386472302859, 34.65000000108393863, 13.14518615778179189 ) ) ;
#11616 = CARTESIAN_POINT ( 'NONE',  ( -5.622872871577873077, 34.89804687716787868, 13.57481594606304753 ) ) ;
#11617 =( BOUNDED_CURVE ( )  B_SPLINE_CURVE ( 2, ( #18478, #18334, #13610, #7488, #674, #20050, #18188, #26898, #7344, #5512, #11755 ),
 .UNSPECIFIED., .F., .F. ) 
 B_SPLINE_CURVE_WITH_KNOTS ( ( 3, 2, 2, 2, 2, 3 ),
 ( 0.5999999999999998668, 0.6199999999999998845, 0.6399999999999999023, 0.6599999999999999201, 0.6799999999999999378, 0.6999999999999998446 ),
 .UNSPECIFIED. ) 
 CURVE ( )  GEOMETRIC_REPRESENTATION_ITEM ( )  RATIONAL_B_SPLINE_CURVE ( ( 1.000000000000000222, 0.9510565162951533091, 1.000000000000000000, 0.9510565162951535312, 1.000000000000000000, 0.9510565162951535312, 1.000000000000000000, 0.9510565162951535312, 1.000000000000000000, 0.9510565162951537532, 0.9999999999999997780 ) ) 
 REPRESENTATION_ITEM ( '' )  );
#11618 = CARTESIAN_POINT ( 'NONE',  ( 103.5355339059327093, -3.535533905932726206, 10.50000000273118594 ) ) ;
#11619 = CARTESIAN_POINT ( 'NONE',  ( 135.4449143864723055, 34.45156250108393436, 13.14518615778179189 ) ) ;
#11620 = CARTESIAN_POINT ( 'NONE',  ( 59.55508561352770158, 40.40468750108393436, -13.14518615778179900 ) ) ;
#11621 = ADVANCED_FACE ( 'NONE', ( #7472 ), #11313, .F. ) ;
#11622 = ORIENTED_EDGE ( 'NONE', *, *, #21676, .T. ) ;
#11623 = FACE_OUTER_BOUND ( 'NONE', #25191, .T. ) ;
#11624 = CARTESIAN_POINT ( 'NONE',  ( -13.14518615778179900, 39.71015625108393010, -5.444914386472297529 ) ) ;
#11625 = CARTESIAN_POINT ( 'NONE',  ( -9.295050272127044266, 32.11992187608393579, 9.295050272127047819 ) ) ;
#11626 = CARTESIAN_POINT ( 'NONE',  ( 96.46446609406721961, 3.535533905932755072, 1.875000000000000000 ) ) ;
#11627 = CARTESIAN_POINT ( 'NONE',  ( 93.46109445667489979, 105.2492070361643215, -55.67499999726882720 ) ) ;
#11628 = DIRECTION ( 'NONE',  ( 0.000000000000000000, 1.000000000000000000, 0.000000000000000000 ) ) ;
#11629 = CARTESIAN_POINT ( 'NONE',  ( 181.8548138422182205, 32.61601562608393579, 0.000000000000000000 ) ) ;
#11630 = AXIS2_PLACEMENT_3D ( 'NONE', #11372, #13363, #17945 ) ;
#11631 = CYLINDRICAL_SURFACE ( 'NONE', #26579, 13.57481594606304398 ) ;
#11632 = CARTESIAN_POINT ( 'NONE',  ( 102.4999999999999858, 124.6069999999781572, -9.847140817659276890E-15 ) ) ;
#11633 = CARTESIAN_POINT ( 'NONE',  ( 99.14382582708707048, 124.4000000010924794, -2.066987299999999195 ) ) ;
#11634 = LINE ( 'NONE', #695, #15500 ) ;
#11635 = CARTESIAN_POINT ( 'NONE',  ( 124.3771271284221740, 36.48554687716787726, 13.57481594606311504 ) ) ;
#11636 = CARTESIAN_POINT ( 'NONE',  ( 99.99999999999995737, 85.00000000000000000, -1.387778780781445676E-14 ) ) ;
#11637 = CARTESIAN_POINT ( 'NONE',  ( 13.57481594606304576, 32.66562499999999858, -1.662435489736055892E-15 ) ) ;
#11638 = CARTESIAN_POINT ( 'NONE',  ( 5.622872871577976994, 40.75195312499999289, -13.57481594606294095 ) ) ;
#11639 = CARTESIAN_POINT ( 'NONE',  ( -5.444914386472297529, 35.84062500108394289, -13.14518615778179900 ) ) ;
#11640 = CARTESIAN_POINT ( 'NONE',  ( 5.444914386472302859, 33.65781250108393152, 13.14518615778179189 ) ) ;
#11641 = CARTESIAN_POINT ( 'NONE',  ( 13.14518615778179722, 35.34453125108392157, 5.444914386472293977 ) ) ;
#11642 = CARTESIAN_POINT ( 'NONE',  ( 13.57481594606304931, 36.68398437716788152, 5.622872871577869525 ) ) ;
#11643 = CARTESIAN_POINT ( 'NONE',  ( 5.622872871578008080, 36.78320312499999289, -13.57481594606290898 ) ) ;
#11644 = CARTESIAN_POINT ( 'NONE',  ( -9.598844408820458085, 35.34453124999998863, -9.598844408820458085 ) ) ;
#11645 = CARTESIAN_POINT ( 'NONE',  ( 70.44491438647230552, 33.65781250108393152, 13.14518615778179189 ) ) ;
#11646 = DIRECTION ( 'NONE',  ( -0.000000000000000000, -1.000000000000000000, -0.000000000000000000 ) ) ;
#11647 = CARTESIAN_POINT ( 'NONE',  ( -5.622872871577920151, 35.39414062716787868, -13.57481594606300135 ) ) ;
#11648 = AXIS2_PLACEMENT_3D ( 'NONE', #21966, #13529, #22531 ) ;
#11649 = EDGE_LOOP ( 'NONE', ( #23077, #2742, #13361, #9566 ) ) ;
#11650 = CARTESIAN_POINT ( 'NONE',  ( 102.0669872999999939, 124.2000000010924907, -0.8561741729129507261 ) ) ;
#11651 = CARTESIAN_POINT ( 'NONE',  ( 214.9999999999999716, 75.00000000000000000, -10.00000000000000000 ) ) ;
#11652 = CARTESIAN_POINT ( 'NONE',  ( 135.4449143864723055, 35.44375000108393436, 13.14518615778179189 ) ) ;
#11653 = VERTEX_POINT ( 'NONE', #4931 ) ;
#11654 = CARTESIAN_POINT ( 'NONE',  ( 99.99999999999995737, 81.25000000000000000, 4.999999999999990230 ) ) ;
#11655 = CARTESIAN_POINT ( 'NONE',  ( -8.312177448680279460E-16, 36.13828125216787157, -13.57481594606304576 ) ) ;
#11656 = CARTESIAN_POINT ( 'NONE',  ( 101.8468681455906903, 82.75000000136560629, 4.458734124999987891 ) ) ;
#11657 = AXIS2_PLACEMENT_3D ( 'NONE', #27569, #27427, #23291 ) ;
#11658 = CARTESIAN_POINT ( 'NONE',  ( 104.9999999999999716, 92.06249999999998579, -2.071067811865478170 ) ) ;
#11659 = CARTESIAN_POINT ( 'NONE',  ( 204.5988444088204687, 37.32890624999999574, 9.598844408820456309 ) ) ;
#11660 = CARTESIAN_POINT ( 'NONE',  ( 91.91746824999997045, 107.3738262389971538, -49.52499999726881441 ) ) ;
#11661 = CARTESIAN_POINT ( 'NONE',  ( 65.00000000000000000, 40.00781250000000000, -13.57481594606304576 ) ) ;
#11662 = CARTESIAN_POINT ( 'NONE',  ( -9.598844408820454532, 38.02343750216788010, 9.598844408820459861 ) ) ;
#11663 = VERTEX_POINT ( 'NONE', #26739 ) ;
#11664 = CARTESIAN_POINT ( 'NONE',  ( 94.99999999999995737, 1.387778780781445676E-14, 9.125000002731184168 ) ) ;
#11665 = CARTESIAN_POINT ( 'NONE',  ( 103.5355339059327093, 3.535533905932755072, 14.62500000000000000 ) ) ;
#11666 = EDGE_LOOP ( 'NONE', ( #6503, #4650, #3733, #22267 ) ) ;
#11667 =( BOUNDED_SURFACE ( )  B_SPLINE_SURFACE ( 1, 2, ( 
 ( #26634, #18210, #16350, #5391, #18353, #25050, #7511, #2957, #20071, #15777, #11632, #549, #13631, #11490, #20355, #693, #9510, #7221, #15910, #7364, #24767, #5248, #13913, #11917, #22640, #27061, #21329, #21054, #18771, #10059, #14479, #1674, #20777, #9920, #8209, #25735, #1538, #10330, #27612, #23196, #3531, #16629, #12187, #10475, #27476 ),
 ( #5809, #17032, #27749, #3673, #16898, #12335, #1399, #3803, #10190, #27885, #18901, #7932, #19183, #20916, #14746, #6219, #25183, #12605, #1810, #8069, #19037, #14336, #16764, #3946, #8347, #25322, #25466, #12463, #16488, #5944, #14612, #25596, #6080, #5671, #23329, #23468, #23054, #21188, #22919, #27341, #3380, #12051, #1259, #18637, #7800 ),
 ( #225, #17748, #13018, #12879, #26451, #6626, #14887, #13304, #21608, #19466, #23603, #17601, #87, #17458, #6489, #10895, #11169, #15455, #26306, #8769, #4084, #12747, #22031, #28025, #24168, #4504, #1948, #13161, #8490, #4220, #10617, #8910, #6769, #4361, #21756, #2086, #21472, #25882, #6351, #17321, #4645, #2507, #15163, #19323, #372 ) ),
 .UNSPECIFIED., .F., .F., .F. ) 
 B_SPLINE_SURFACE_WITH_KNOTS ( ( 2, 1, 2 ),
 ( 3, 2, 2, 2, 2, 2, 2, 2, 2, 2, 2, 2, 2, 2, 2, 2, 2, 2, 2, 2, 2, 2, 3 ),
 ( -0.01000000000000000021, 0.000000000000000000, 1.000000000000000000 ),
 ( -0.008333333333333333218, 0.000000000000000000, 0.04166666666666666435, 0.08333333333333332871, 0.1250000000000000000, 0.1666666666666666574, 0.2083333333333333426, 0.2500000000000000000, 0.2916666666666666852, 0.3333333333333333148, 0.3750000000000000000, 0.4166666666666666852, 0.4583333333333333148, 0.5000000000000000000, 0.5416666666666666297, 0.5833333333333333703, 0.6250000000000000000, 0.6666666666666666297, 0.7083333333333333703, 0.7500000000000000000, 0.7916666666666666297, 0.8333333333333333703, 0.8417499999999999982 ),
 .UNSPECIFIED. ) 
 GEOMETRIC_REPRESENTATION_ITEM ( )  RATIONAL_B_SPLINE_SURFACE ( (
 ( 1.000000000000000000, 1.000000000000000000, 1.000000000000000000, 0.9238795325112867385, 1.000000000000000000, 0.9238795325112867385, 1.000000000000000000, 0.9238795325112867385, 1.000000000000000000, 0.9238795325112867385, 1.000000000000000000, 0.9238795325112867385, 1.000000000000000000, 0.9238795325112867385, 1.000000000000000000, 0.9238795325112867385, 1.000000000000000000, 0.9238795325112867385, 1.000000000000000000, 0.9238795325112867385, 1.000000000000000000, 0.9238795325112867385, 1.000000000000000000, 0.9238795325112867385, 1.000000000000000000, 0.9238795325112867385, 1.000000000000000000, 0.9238795325112867385, 1.000000000000000000, 0.9238795325112867385, 1.000000000000000000, 0.9238795325112867385, 1.000000000000000000, 0.9238795325112867385, 1.000000000000000000, 0.9238795325112867385, 1.000000000000000000, 0.9238795325112867385, 1.000000000000000000, 0.9238795325112867385, 1.000000000000000000, 0.9238795325112867385, 1.000000000000000000, 1.000000000000000000, 1.000000000000000000),
 ( 1.000000000000000000, 1.000000000000000000, 1.000000000000000000, 0.9238795325112867385, 1.000000000000000000, 0.9238795325112867385, 1.000000000000000000, 0.9238795325112867385, 1.000000000000000000, 0.9238795325112867385, 1.000000000000000000, 0.9238795325112867385, 1.000000000000000000, 0.9238795325112867385, 1.000000000000000000, 0.9238795325112867385, 1.000000000000000000, 0.9238795325112867385, 1.000000000000000000, 0.9238795325112867385, 1.000000000000000000, 0.9238795325112867385, 1.000000000000000000, 0.9238795325112867385, 1.000000000000000000, 0.9238795325112867385, 1.000000000000000000, 0.9238795325112867385, 1.000000000000000000, 0.9238795325112867385, 1.000000000000000000, 0.9238795325112867385, 1.000000000000000000, 0.9238795325112867385, 1.000000000000000000, 0.9238795325112867385, 1.000000000000000000, 0.9238795325112867385, 1.000000000000000000, 0.9238795325112867385, 1.000000000000000000, 0.9238795325112867385, 1.000000000000000000, 1.000000000000000000, 1.000000000000000000),
 ( 1.000000000000000000, 1.000000000000000000, 1.000000000000000000, 0.9238795325112867385, 1.000000000000000000, 0.9238795325112867385, 1.000000000000000000, 0.9238795325112867385, 1.000000000000000000, 0.9238795325112867385, 1.000000000000000000, 0.9238795325112867385, 1.000000000000000000, 0.9238795325112867385, 1.000000000000000000, 0.9238795325112867385, 1.000000000000000000, 0.9238795325112867385, 1.000000000000000000, 0.9238795325112867385, 1.000000000000000000, 0.9238795325112867385, 1.000000000000000000, 0.9238795325112867385, 1.000000000000000000, 0.9238795325112867385, 1.000000000000000000, 0.9238795325112867385, 1.000000000000000000, 0.9238795325112867385, 1.000000000000000000, 0.9238795325112867385, 1.000000000000000000, 0.9238795325112867385, 1.000000000000000000, 0.9238795325112867385, 1.000000000000000000, 0.9238795325112867385, 1.000000000000000000, 0.9238795325112867385, 1.000000000000000000, 0.9238795325112867385, 1.000000000000000000, 1.000000000000000000, 1.000000000000000000) ) ) 
 REPRESENTATION_ITEM ( '' )  SURFACE ( )  );
#11668 = CARTESIAN_POINT ( 'NONE',  ( -9.295050272127046043, 35.09648437608393579, -9.295050272127046043 ) ) ;
#11669 = CARTESIAN_POINT ( 'NONE',  ( 185.4011555911795597, 31.67343750216787512, 9.598844408820459861 ) ) ;
#11670 = AXIS2_PLACEMENT_3D ( 'NONE', #19693, #6444, #465 ) ;
#11671 = CARTESIAN_POINT ( 'NONE',  ( -13.14518615778179544, 34.20351562608393436, 0.000000000000000000 ) ) ;
#11672 = CARTESIAN_POINT ( 'NONE',  ( 195.0000000000000000, 36.13828125216787157, -13.57481594606304576 ) ) ;
#11673 = CARTESIAN_POINT ( 'NONE',  ( 116.8548138422182205, 40.50390625108394005, -5.444914386472297529 ) ) ;
#11674 = CARTESIAN_POINT ( 'NONE',  ( -9.295050272127044266, 35.29492187608393294, 9.295050272127047819 ) ) ;
#11675 = EDGE_CURVE ( 'NONE', #3896, #14666, #2650, .T. ) ;
#11676 = CARTESIAN_POINT ( 'NONE',  ( 120.7049497278729575, 31.92148437608393508, 9.295050272127047819 ) ) ;
#11677 = DIRECTION ( 'NONE',  ( 1.000000000000000000, 0.000000000000000000, 0.000000000000000000 ) ) ;
#11678 = CARTESIAN_POINT ( 'NONE',  ( 124.4309414480975136, 36.00000000000002842, 11.91493531101283843 ) ) ;
#11679 = CARTESIAN_POINT ( 'NONE',  ( 104.4587341249999781, 1.846868145590750299, 5.250000001365592972 ) ) ;
#11680 = CARTESIAN_POINT ( 'NONE',  ( -13.57481594606304753, 37.87460937716787868, -5.622872871577872189 ) ) ;
#11681 = CARTESIAN_POINT ( 'NONE',  ( 99.99999999999995737, 4.458734125000016313, 8.187500001365592084 ) ) ;
#11682 = CARTESIAN_POINT ( 'NONE',  ( 99.99999999999998579, 101.5015231886685854, -46.62500000273119838 ) ) ;
#11683 = CYLINDRICAL_SURFACE ( 'NONE', #23016, 13.57481594606304398 ) ;
#11684 = CARTESIAN_POINT ( 'NONE',  ( 91.91746824999998466, 110.0000000000000000, -55.62499999726882294 ) ) ;
#11685 = CARTESIAN_POINT ( 'NONE',  ( 13.14518615778179544, 33.21132812608393436, -1.609821015232357215E-15 ) ) ;
#11686 = ORIENTED_EDGE ( 'NONE', *, *, #1447, .T. ) ;
#11687 = SURFACE_SIDE_STYLE ('',( #2743 ) ) ;
#11688 = AXIS2_PLACEMENT_3D ( 'NONE', #18403, #5721, #3578 ) ;
#11689 = DIRECTION ( 'NONE',  ( 0.000000000000000000, 0.000000000000000000, 1.000000000000000000 ) ) ;
#11690 = CARTESIAN_POINT ( 'NONE',  ( -13.57481594606304398, 36.28710937499999289, 5.622872871577880183 ) ) ;
#11691 = CARTESIAN_POINT ( 'NONE',  ( 204.2950502721270425, 36.08867187608392868, 9.295050272127046043 ) ) ;
#11692 = ORIENTED_EDGE ( 'NONE', *, *, #3251, .F. ) ;
#11693 = LINE ( 'NONE', #1319, #17633 ) ;
#11694 = CARTESIAN_POINT ( 'NONE',  ( 101.8468681455906903, 4.458734125000016313, 9.375000001365592084 ) ) ;
#11695 = ORIENTED_EDGE ( 'NONE', *, *, #22026, .F. ) ;
#11696 = CARTESIAN_POINT ( 'NONE',  ( 104.9952793366501851, 116.8754121666685393, -54.07500000273119412 ) ) ;
#11697 = CARTESIAN_POINT ( 'NONE',  ( 2.414731522848535132E-15, 35.98945312608393010, 13.14518615778179544 ) ) ;
#11698 = CARTESIAN_POINT ( 'NONE',  ( 65.00000000000000000, 40.10703125216787157, -13.57481594606304576 ) ) ;
#11699 =( BOUNDED_SURFACE ( )  B_SPLINE_SURFACE ( 1, 2, ( 
 ( #25086, #7836, #1163, #10093, #9551, #25222, #20540, #16529, #18536, #16097, #9693, #24804, #5711, #18252, #1293, #14377, #1022, #3567, #23093, #5286, #22960, #12225, #14239, #26960, #1435, #3422, #22818, #16247, #24944, #20815, #18393, #12089, #18806, #27240, #27099, #7551, #16388, #3287, #5430, #5574, #5236, #15765, #24328, #4957, #9357, #2676, #13901, #24754, #6933, #24472, #22482, #13619, #7206, #22341, #19913, #22628, #2811, #2947, #11618, #18050, #396, #11480, #3097, #7353, #18196, #20197, #18343, #4670, #11764, #26763, #15627, #11337, #682, #5095, #9078, #4812, #2532, #829, #20343, #15900, #24617, #22197, #6791, #17773, #26477, #9220, #26907, #20488, #7070, #20058, #13472, #16044, #969, #537, #17912, #26623, #15476, #24191, #13757, #9496, #9639, #13332, #22058, #11196, #9910, #16751, #25169, #27463, #20627, #14048, #1387, #27328, #3658, #10048, #12319, #7787, #1657, #7497, #27595, #9778, #10177, #5658, #16192, #7646, #24899, #18886, #5379, #5798, #21040, #22769, #25452, #1525, #3235, #18759, #8057, #7920, #10316, #16616, #18625, #11902, #1111, #18486, #16474, #5932, #14322, #25309, #27195, #27048, #20763, #16338, #25038, #23043, #3516, #14600, #12175, #5520, #20905, #14464, #22905, #23318, #3791, #14187, #23182, #12450, #21176, #3368, #12039, #1248, #8755, #28013, #15151, #23870, #2073, #3932, #15012, #15297, #19591, #2218, #4207, #2360, #16886, #17447, #10741, #19171, #23590, #12866, #17305, #12591, #8335, #14734, #13003, #4349, #8477, #17166, #6205, #19024, #1798, #10463, #21458, #10882, #6613, #19312, #4072, #25722, #74, #4491, #12734, #19451, #27873, #23734, #28150, #17019, #8617, #21886, #26005, #1936, #25869, #25585, #27736, #14875, #26146, #6476, #6338, #24013, #10605 ),
 ( #21596, #13148, #21743, #8196, #6068, #23454, #21315, #19471, #13167, #21906, #2380, #11038, #23750, #13311, #19609, #231, #6633, #23890, #4227, #4369, #21476, #28170, #6495, #6774, #19748, #17464, #8918, #24031, #2092, #17606, #13025, #17184, #23614, #17329, #10624, #8639, #25745, #10760, #22038, #6227, #28033, #26313, #19192, #1954, #4510, #2514, #21762, #15460, #26024, #15033, #17041, #4652, #15171, #2239, #14893, #24175, #27894, #10901, #26166, #94, #8775, #8499, #15317, #8355, #4090, #25890, #12755, #19329, #6359, #12886, #21616, #810, #4794, #9338, #17895, #20323, #18032, #16175, #7187, #15748, #27034, #520, #3081, #14028, #13453, #951, #16026, #11746, #22753, #26603, #22465, #20472, #19894, #24739, #18327, #20041, #26745, #2795, #24883, #15885, #17757, #24601, #5362, #7480, #11176, #4938, #20181, #5079, #22179, #9062, #9622, #26891, #9201, #378, #2930, #26460, #6914, #15605, #7049, #24308, #2658, #11319, #5220, #24452, #13741, #13601, #11600, #22324, #11462, #665, #9478, #18180, #7337, #13885, #22611, #1752, #10558, #8285, #23406, #12407, #3881, #4165, #25817, #1613, #8008, #14687, #25676, #10418, #3218, #21415, #25406, #19124, #10271, #12690, #27831, #8569, #16976, #8152, #19401, #21127, #23688, #6434, #5888, #21551, #8424, #12825, #15102, #18980, #14824, #2026, #11885, #17113, #10694, #27689, #6157, #12542, #17260, #23547, #9761, #4024, #25961, #28105, #20610, #25543, #21268, #1893, #14558, #1094, #18471, #19268, #16845, #27551, #27967, #16708, #23273, #3746, #6292, #14969, #6023, #4582, #9136, #17401, #13242, #11112, #27, #26533, #4874, #26101, #11256, #17829, #6566, #15684, #19975, #24105, #6990, #24385, #13538, #22259, #170, #17972, #24245, #2734, #454, #311, #8852 ) ),
 .UNSPECIFIED., .F., .F., .F. ) 
 B_SPLINE_SURFACE_WITH_KNOTS ( ( 2, 2 ),
 ( 3, 2, 2, 2, 2, 2, 2, 2, 2, 2, 2, 2, 2, 2, 2, 2, 2, 2, 2, 2, 2, 2, 2, 2, 2, 2, 2, 2, 2, 2, 2, 2, 2, 2, 2, 2, 2, 2, 2, 2, 2, 2, 2, 2, 2, 2, 2, 2, 2, 2, 2, 2, 2, 2, 2, 2, 2, 2, 2, 2, 2, 2, 2, 2, 2, 2, 2, 2, 2, 2, 2, 2, 2, 2, 2, 2, 2, 2, 2, 2, 2, 2, 2, 2, 2, 2, 2, 2, 2, 2, 2, 2, 2, 2, 2, 2, 2, 2, 2, 2, 2, 2, 2, 2, 2, 2, 2, 2, 2, 2, 2, 2, 3 ),
 ( 0.000000000000000000, 1.000000000000000000 ),
 ( 0.000000000000000000, 0.008928571428571428076, 0.01785714285714285615, 0.02678571428571428423, 0.03571428571428571230, 0.04464285714285714385, 0.05357142857142856845, 0.06250000000000000000, 0.07142857142857142461, 0.08035714285714286309, 0.08928571428571428770, 0.09821428571428571230, 0.1071428571428571369, 0.1160714285714285754, 0.1250000000000000000, 0.1339285714285714246, 0.1428571428571428492, 0.1517857142857142738, 0.1607142857142857262, 0.1696428571428571508, 0.1785714285714285754, 0.1875000000000000000, 0.1964285714285714246, 0.2053571428571428492, 0.2142857142857142738, 0.2232142857142857262, 0.2321428571428571508, 0.2410714285714285754, 0.2500000000000000000, 0.2589285714285714524, 0.2678571428571428492, 0.2767857142857143016, 0.2857142857142856984, 0.2946428571428571508, 0.3035714285714285476, 0.3125000000000000000, 0.3214285714285714524, 0.3303571428571428492, 0.3392857142857143016, 0.3482142857142856984, 0.3571428571428571508, 0.3660714285714285476, 0.3750000000000000000, 0.3839285714285714524, 0.3928571428571428492, 0.4017857142857143016, 0.4107142857142856984, 0.4196428571428571508, 0.4285714285714285476, 0.4375000000000000000, 0.4464285714285714524, 0.4553571428571428492, 0.4642857142857143016, 0.4732142857142856984, 0.4821428571428571508, 0.4910714285714285476, 0.5000000000000000000, 0.5089285714285713969, 0.5178571428571429047, 0.5267857142857143016, 0.5357142857142856984, 0.5446428571428570953, 0.5535714285714286031, 0.5625000000000000000, 0.5714285714285713969, 0.5803571428571429047, 0.5892857142857143016, 0.5982142857142856984, 0.6071428571428570953, 0.6160714285714286031, 0.6250000000000000000, 0.6339285714285713969, 0.6428571428571429047, 0.6517857142857143016, 0.6607142857142856984, 0.6696428571428570953, 0.6785714285714286031, 0.6875000000000000000, 0.6964285714285713969, 0.7053571428571429047, 0.7142857142857143016, 0.7232142857142856984, 0.7321428571428570953, 0.7410714285714286031, 0.7500000000000000000, 0.7589285714285713969, 0.7678571428571429047, 0.7767857142857143016, 0.7857142857142856984, 0.7946428571428570953, 0.8035714285714286031, 0.8125000000000000000, 0.8214285714285713969, 0.8303571428571429047, 0.8392857142857143016, 0.8482142857142856984, 0.8571428571428570953, 0.8660714285714286031, 0.8750000000000000000, 0.8839285714285713969, 0.8928571428571429047, 0.9017857142857143016, 0.9107142857142856984, 0.9196428571428570953, 0.9285714285714286031, 0.9375000000000000000, 0.9464285714285713969, 0.9553571428571429047, 0.9642857142857143016, 0.9732142857142856984, 0.9821428571428570953, 0.9910714285714286031, 1.000000000000000000 ),
 .UNSPECIFIED. ) 
 GEOMETRIC_REPRESENTATION_ITEM ( )  RATIONAL_B_SPLINE_SURFACE ( (
 ( 1.000000000000000000, 0.9238795325112867385, 1.000000000000000000, 0.9238795325112867385, 1.000000000000000000, 0.9238795325112867385, 1.000000000000000000, 0.9238795325112867385, 1.000000000000000000, 0.9238795325112867385, 1.000000000000000000, 0.9238795325112867385, 1.000000000000000000, 0.9238795325112867385, 1.000000000000000000, 0.9238795325112867385, 1.000000000000000000, 0.9238795325112867385, 1.000000000000000000, 0.9238795325112867385, 1.000000000000000000, 0.9238795325112867385, 1.000000000000000000, 0.9238795325112867385, 1.000000000000000000, 0.9238795325112867385, 1.000000000000000000, 0.9238795325112867385, 1.000000000000000000, 0.9238795325112867385, 1.000000000000000000, 0.9238795325112867385, 1.000000000000000000, 0.9238795325112867385, 1.000000000000000000, 0.9238795325112867385, 1.000000000000000000, 0.9238795325112867385, 1.000000000000000000, 0.9238795325112867385, 1.000000000000000000, 0.9238795325112867385, 1.000000000000000000, 0.9238795325112867385, 1.000000000000000000, 0.9238795325112867385, 1.000000000000000000, 0.9238795325112867385, 1.000000000000000000, 0.9238795325112867385, 1.000000000000000000, 0.9238795325112867385, 1.000000000000000000, 0.9238795325112867385, 1.000000000000000000, 0.9238795325112867385, 1.000000000000000000, 0.9238795325112867385, 1.000000000000000000, 0.9238795325112867385, 1.000000000000000000, 0.9238795325112867385, 1.000000000000000000, 0.9238795325112867385, 1.000000000000000000, 0.9238795325112867385, 1.000000000000000000, 0.9238795325112867385, 1.000000000000000000, 0.9238795325112867385, 1.000000000000000000, 0.9238795325112867385, 1.000000000000000000, 0.9238795325112867385, 1.000000000000000000, 0.9238795325112867385, 1.000000000000000000, 0.9238795325112867385, 1.000000000000000000, 0.9238795325112867385, 1.000000000000000000, 0.9238795325112867385, 1.000000000000000000, 0.9238795325112867385, 1.000000000000000000, 0.9238795325112867385, 1.000000000000000000, 0.9238795325112867385, 1.000000000000000000, 0.9238795325112867385, 1.000000000000000000, 0.9238795325112867385, 1.000000000000000000, 0.9238795325112867385, 1.000000000000000000, 0.9238795325112867385, 1.000000000000000000, 0.9238795325112867385, 1.000000000000000000, 0.9238795325112867385, 1.000000000000000000, 0.9238795325112867385, 1.000000000000000000, 0.9238795325112867385, 1.000000000000000000, 0.9238795325112867385, 1.000000000000000000, 0.9238795325112867385, 1.000000000000000000, 0.9238795325112867385, 1.000000000000000000, 0.9238795325112867385, 1.000000000000000000, 0.9238795325112867385, 1.000000000000000000, 0.9238795325112867385, 1.000000000000000000, 0.9238795325112867385, 1.000000000000000000, 0.9238795325112867385, 1.000000000000000000, 0.9238795325112867385, 1.000000000000000000, 0.9238795325112867385, 1.000000000000000000, 0.9238795325112867385, 1.000000000000000000, 0.9238795325112867385, 1.000000000000000000, 0.9238795325112867385, 1.000000000000000000, 0.9238795325112867385, 1.000000000000000000, 0.9238795325112867385, 1.000000000000000000, 0.9238795325112867385, 1.000000000000000000, 0.9238795325112867385, 1.000000000000000000, 0.9238795325112867385, 1.000000000000000000, 0.9238795325112867385, 1.000000000000000000, 0.9238795325112867385, 1.000000000000000000, 0.9238795325112867385, 1.000000000000000000, 0.9238795325112867385, 1.000000000000000000, 0.9238795325112867385, 1.000000000000000000, 0.9238795325112867385, 1.000000000000000000, 0.9238795325112867385, 1.000000000000000000, 0.9238795325112867385, 1.000000000000000000, 0.9238795325112867385, 1.000000000000000000, 0.9238795325112867385, 1.000000000000000000, 0.9238795325112867385, 1.000000000000000000, 0.9238795325112867385, 1.000000000000000000, 0.9238795325112867385, 1.000000000000000000, 0.9238795325112867385, 1.000000000000000000, 0.9238795325112867385, 1.000000000000000000, 0.9238795325112867385, 1.000000000000000000, 0.9238795325112867385, 1.000000000000000000, 0.9238795325112867385, 1.000000000000000000, 0.9238795325112867385, 1.000000000000000000, 0.9238795325112867385, 1.000000000000000000, 0.9238795325112867385, 1.000000000000000000, 0.9238795325112867385, 1.000000000000000000, 0.9238795325112867385, 1.000000000000000000, 0.9238795325112867385, 1.000000000000000000, 0.9238795325112867385, 1.000000000000000000, 0.9238795325112867385, 1.000000000000000000, 0.9238795325112867385, 1.000000000000000000, 0.9238795325112867385, 1.000000000000000000, 0.9238795325112867385, 1.000000000000000000, 0.9238795325112867385, 1.000000000000000000, 0.9238795325112867385, 1.000000000000000000, 0.9238795325112867385, 1.000000000000000000, 0.9238795325112867385, 1.000000000000000000, 0.9238795325112867385, 1.000000000000000000, 0.9238795325112867385, 1.000000000000000000, 0.9238795325112867385, 1.000000000000000000, 0.9238795325112867385, 1.000000000000000000, 0.9238795325112867385, 1.000000000000000000, 0.9238795325112867385, 1.000000000000000000, 0.9238795325112867385, 1.000000000000000000, 0.9238795325112867385, 1.000000000000000000, 0.9238795325112867385, 1.000000000000000000),
 ( 1.000000000000000000, 0.9238795325112867385, 1.000000000000000000, 0.9238795325112867385, 1.000000000000000000, 0.9238795325112867385, 1.000000000000000000, 0.9238795325112867385, 1.000000000000000000, 0.9238795325112867385, 1.000000000000000000, 0.9238795325112867385, 1.000000000000000000, 0.9238795325112867385, 1.000000000000000000, 0.9238795325112867385, 1.000000000000000000, 0.9238795325112867385, 1.000000000000000000, 0.9238795325112867385, 1.000000000000000000, 0.9238795325112867385, 1.000000000000000000, 0.9238795325112867385, 1.000000000000000000, 0.9238795325112867385, 1.000000000000000000, 0.9238795325112867385, 1.000000000000000000, 0.9238795325112867385, 1.000000000000000000, 0.9238795325112867385, 1.000000000000000000, 0.9238795325112867385, 1.000000000000000000, 0.9238795325112867385, 1.000000000000000000, 0.9238795325112867385, 1.000000000000000000, 0.9238795325112867385, 1.000000000000000000, 0.9238795325112867385, 1.000000000000000000, 0.9238795325112867385, 1.000000000000000000, 0.9238795325112867385, 1.000000000000000000, 0.9238795325112867385, 1.000000000000000000, 0.9238795325112867385, 1.000000000000000000, 0.9238795325112867385, 1.000000000000000000, 0.9238795325112867385, 1.000000000000000000, 0.9238795325112867385, 1.000000000000000000, 0.9238795325112867385, 1.000000000000000000, 0.9238795325112867385, 1.000000000000000000, 0.9238795325112867385, 1.000000000000000000, 0.9238795325112867385, 1.000000000000000000, 0.9238795325112867385, 1.000000000000000000, 0.9238795325112867385, 1.000000000000000000, 0.9238795325112867385, 1.000000000000000000, 0.9238795325112867385, 1.000000000000000000, 0.9238795325112867385, 1.000000000000000000, 0.9238795325112867385, 1.000000000000000000, 0.9238795325112867385, 1.000000000000000000, 0.9238795325112867385, 1.000000000000000000, 0.9238795325112867385, 1.000000000000000000, 0.9238795325112867385, 1.000000000000000000, 0.9238795325112867385, 1.000000000000000000, 0.9238795325112867385, 1.000000000000000000, 0.9238795325112867385, 1.000000000000000000, 0.9238795325112867385, 1.000000000000000000, 0.9238795325112867385, 1.000000000000000000, 0.9238795325112867385, 1.000000000000000000, 0.9238795325112867385, 1.000000000000000000, 0.9238795325112867385, 1.000000000000000000, 0.9238795325112867385, 1.000000000000000000, 0.9238795325112867385, 1.000000000000000000, 0.9238795325112867385, 1.000000000000000000, 0.9238795325112867385, 1.000000000000000000, 0.9238795325112867385, 1.000000000000000000, 0.9238795325112867385, 1.000000000000000000, 0.9238795325112867385, 1.000000000000000000, 0.9238795325112867385, 1.000000000000000000, 0.9238795325112867385, 1.000000000000000000, 0.9238795325112867385, 1.000000000000000000, 0.9238795325112867385, 1.000000000000000000, 0.9238795325112867385, 1.000000000000000000, 0.9238795325112867385, 1.000000000000000000, 0.9238795325112867385, 1.000000000000000000, 0.9238795325112867385, 1.000000000000000000, 0.9238795325112867385, 1.000000000000000000, 0.9238795325112867385, 1.000000000000000000, 0.9238795325112867385, 1.000000000000000000, 0.9238795325112867385, 1.000000000000000000, 0.9238795325112867385, 1.000000000000000000, 0.9238795325112867385, 1.000000000000000000, 0.9238795325112867385, 1.000000000000000000, 0.9238795325112867385, 1.000000000000000000, 0.9238795325112867385, 1.000000000000000000, 0.9238795325112867385, 1.000000000000000000, 0.9238795325112867385, 1.000000000000000000, 0.9238795325112867385, 1.000000000000000000, 0.9238795325112867385, 1.000000000000000000, 0.9238795325112867385, 1.000000000000000000, 0.9238795325112867385, 1.000000000000000000, 0.9238795325112867385, 1.000000000000000000, 0.9238795325112867385, 1.000000000000000000, 0.9238795325112867385, 1.000000000000000000, 0.9238795325112867385, 1.000000000000000000, 0.9238795325112867385, 1.000000000000000000, 0.9238795325112867385, 1.000000000000000000, 0.9238795325112867385, 1.000000000000000000, 0.9238795325112867385, 1.000000000000000000, 0.9238795325112867385, 1.000000000000000000, 0.9238795325112867385, 1.000000000000000000, 0.9238795325112867385, 1.000000000000000000, 0.9238795325112867385, 1.000000000000000000, 0.9238795325112867385, 1.000000000000000000, 0.9238795325112867385, 1.000000000000000000, 0.9238795325112867385, 1.000000000000000000, 0.9238795325112867385, 1.000000000000000000, 0.9238795325112867385, 1.000000000000000000, 0.9238795325112867385, 1.000000000000000000, 0.9238795325112867385, 1.000000000000000000, 0.9238795325112867385, 1.000000000000000000, 0.9238795325112867385, 1.000000000000000000, 0.9238795325112867385, 1.000000000000000000, 0.9238795325112867385, 1.000000000000000000, 0.9238795325112867385, 1.000000000000000000, 0.9238795325112867385, 1.000000000000000000, 0.9238795325112867385, 1.000000000000000000, 0.9238795325112867385, 1.000000000000000000, 0.9238795325112867385, 1.000000000000000000, 0.9238795325112867385, 1.000000000000000000, 0.9238795325112867385, 1.000000000000000000, 0.9238795325112867385, 1.000000000000000000, 0.9238795325112867385, 1.000000000000000000) ) ) 
 REPRESENTATION_ITEM ( '' )  SURFACE ( )  );
#11700 = CARTESIAN_POINT ( 'NONE',  ( 130.0000000000000000, -7.395377635281828788, -13.57481594606305997 ) ) ;
#11701 = CARTESIAN_POINT ( 'NONE',  ( 124.5550856135277087, 38.81718750108393579, -13.14518615778179900 ) ) ;
#11702 = CARTESIAN_POINT ( 'NONE',  ( -9.295050272127046043, 37.47773437608393010, -9.295050272127046043 ) ) ;
#11703 = CARTESIAN_POINT ( 'NONE',  ( 9.295050272127046043, 35.49335937608393010, -9.295050272127046043 ) ) ;
#11704 = CARTESIAN_POINT ( 'NONE',  ( 99.99999999999998579, 92.81249999863440792, -4.458734124999994997 ) ) ;
#11705 = VECTOR ( 'NONE', #10186, 1000.000000000000000 ) ;
#11706 = VECTOR ( 'NONE', #25806, 1000.000000000000000 ) ;
#11707 = CARTESIAN_POINT ( 'NONE',  ( 63.18564464541649528, 51.46618445021698562, -14.99999999999862865 ) ) ;
#11708 = CARTESIAN_POINT ( 'NONE',  ( 108.0825317500000011, 107.3738262389971680, -52.47500000273119269 ) ) ;
#11709 = EDGE_CURVE ( 'NONE', #3863, #7002, #18318, .T. ) ;
#11710 = CARTESIAN_POINT ( 'NONE',  ( 84.99999999999998579, 120.0000000000000000, -15.00000000000000533 ) ) ;
#11711 = CARTESIAN_POINT ( 'NONE',  ( -9.295050272127046043, 36.68398437608393436, -9.295050272127046043 ) ) ;
#11712 = CARTESIAN_POINT ( 'NONE',  ( 104.4587341249999781, -1.846868145590721655, 7.125000001365593860 ) ) ;
#11713 = CARTESIAN_POINT ( 'NONE',  ( 78.14518615778180788, 37.82500000108392868, -5.444914386472297529 ) ) ;
#11714 = PRODUCT ( 'vaccum generator', 'vaccum generator', '', ( #1857 ) ) ;
#11715 = CARTESIAN_POINT ( 'NONE',  ( 101.0355339059327235, 124.4499999999999744, 2.499999999999974687 ) ) ;
#11716 = DIRECTION ( 'NONE',  ( -0.000000000000000000, -1.000000000000000000, -0.000000000000000000 ) ) ;
#11717 = CARTESIAN_POINT ( 'NONE',  ( -9.295050272127044266, 33.70742187608393436, 9.295050272127047819 ) ) ;
#11718 = CARTESIAN_POINT ( 'NONE',  ( 99.99999999999998579, 122.7500000010924879, -2.066987299999998751 ) ) ;
#11719 = CARTESIAN_POINT ( 'NONE',  ( 98.23223304703363112, 124.8999999999999915, -1.767766952966370209 ) ) ;
#11720 = CARTESIAN_POINT ( 'NONE',  ( 204.2950502721270425, 38.66835937608393436, 9.295050272127046043 ) ) ;
#11721 = CARTESIAN_POINT ( 'NONE',  ( 93.46109445667489979, 105.2492070361643215, -51.67499999726882010 ) ) ;
#11722 = ORIENTED_EDGE ( 'NONE', *, *, #17150, .F. ) ;
#11723 = CARTESIAN_POINT ( 'NONE',  ( -13.57481594606304576, 34.69960937499999432, 5.622872871577880183 ) ) ;
#11724 = CARTESIAN_POINT ( 'NONE',  ( -13.14518615778179900, 32.56640625108394005, -5.444914386472297529 ) ) ;
#11725 = VERTEX_POINT ( 'NONE', #14021 ) ;
#11726 = CARTESIAN_POINT ( 'NONE',  ( 120.7049497278729575, 33.70742187608393436, 9.295050272127047819 ) ) ;
#11727 = CARTESIAN_POINT ( 'NONE',  ( 181.4251840539369596, 37.13046875216787868, 0.000000000000000000 ) ) ;
#11728 = CARTESIAN_POINT ( 'NONE',  ( 195.0000000000000000, 33.40976562608393863, -13.14518615778179544 ) ) ;
#11729 = EDGE_CURVE ( 'NONE', #7953, #8513, #8018, .T. ) ;
#11730 = ORIENTED_EDGE ( 'NONE', *, *, #22425, .F. ) ;
#11731 = CARTESIAN_POINT ( 'NONE',  ( 100.8561741729129437, 124.0000000010925021, 2.066987299999979655 ) ) ;
#11732 = CYLINDRICAL_SURFACE ( 'NONE', #5629, 7.000000000000006217 ) ;
#11733 = FACE_OUTER_BOUND ( 'NONE', #10879, .T. ) ;
#11734 = CARTESIAN_POINT ( 'NONE',  ( 120.4011555911795455, 36.23750000216787726, -9.598844408820458085 ) ) ;
#11735 = CARTESIAN_POINT ( 'NONE',  ( 108.0825317500000011, 107.3738262389971680, -50.22500000273118559 ) ) ;
#11736 = DIRECTION ( 'NONE',  ( 0.000000000000000000, 0.000000000000000000, 1.000000000000000000 ) ) ;
#11737 = ADVANCED_FACE ( 'NONE', ( #1087 ), #15879, .T. ) ;
#11738 = CARTESIAN_POINT ( 'NONE',  ( 9.598844408820456309, 32.07031250216787299, -9.598844408820458085 ) ) ;
#11739 = CARTESIAN_POINT ( 'NONE',  ( 67.27614684454866278, 51.46995505939283078, 14.99999999999998046 ) ) ;
#11740 = EDGE_CURVE ( 'NONE', #19588, #19872, #6930, .T. ) ;
#11741 = ORIENTED_EDGE ( 'NONE', *, *, #10447, .T. ) ;
#11742 = SURFACE_STYLE_USAGE ( .BOTH. , #27030 ) ;
#11743 = CARTESIAN_POINT ( 'NONE',  ( 99.99999999999995737, 4.458734125000016313, 6.187500001365592084 ) ) ;
#11744 = VERTEX_POINT ( 'NONE', #11455 ) ;
#11745 = CARTESIAN_POINT ( 'NONE',  ( -9.839381608887936892, 36.00000000000000711, -9.004033604613056241 ) ) ;
#11746 = CARTESIAN_POINT ( 'NONE',  ( 104.4587341249999781, 1.846868145590750299, 9.000000001365593860 ) ) ;
#11747 = LINE ( 'NONE', #16176, #9409 ) ;
#11748 = EDGE_CURVE ( 'NONE', #10079, #1506, #20601, .T. ) ;
#11749 = AXIS2_PLACEMENT_3D ( 'NONE', #21765, #8779, #8502 ) ;
#11750 = DIRECTION ( 'NONE',  ( -0.000000000000000000, 1.000000000000000000, -0.000000000000000000 ) ) ;
#11751 = CARTESIAN_POINT ( 'NONE',  ( 55.70494972787295751, 32.71523437608393436, -9.295050272127046043 ) ) ;
#11752 = CARTESIAN_POINT ( 'NONE',  ( 103.5355339059327235, 91.74999999726880162, 3.535533905932724874 ) ) ;
#11753 = CARTESIAN_POINT ( 'NONE',  ( 102.4976396683250925, 117.6869444889999841, -47.72500000273119269 ) ) ;
#11754 = CARTESIAN_POINT ( 'NONE',  ( 13.14518615778179544, 36.18789062608393436, -1.609821015232357215E-15 ) ) ;
#11755 = CARTESIAN_POINT ( 'NONE',  ( 107.0000000000000000, 110.0000000000000000, -53.49999999453763877 ) ) ;
#11756 = CARTESIAN_POINT ( 'NONE',  ( -7.115490391851705176, 49.99999999945661244, 11.58166858714319147 ) ) ;
#11757 = CARTESIAN_POINT ( 'NONE',  ( 65.00000000000000000, 40.80156249999999574, -13.57481594606304576 ) ) ;
#11758 = CARTESIAN_POINT ( 'NONE',  ( 120.4011555911795455, 32.96328124999999432, -9.598844408820458085 ) ) ;
#11759 = ADVANCED_FACE ( 'NONE', ( #803 ), #13877, .F. ) ;
#11760 = ORIENTED_EDGE ( 'NONE', *, *, #14543, .T. ) ;
#11761 = FACE_OUTER_BOUND ( 'NONE', #25941, .T. ) ;
#11762 = CARTESIAN_POINT ( 'NONE',  ( 13.14518615778179900, 34.84843750108393579, -5.444914386472297529 ) ) ;
#11763 = CARTESIAN_POINT ( 'NONE',  ( 9.598844408820456309, 32.86406250216787583, -9.598844408820458085 ) ) ;
#11764 = CARTESIAN_POINT ( 'NONE',  ( 99.99999999999995737, 5.000000000000018652, 9.875000002731185944 ) ) ;
#11765 = CARTESIAN_POINT ( 'NONE',  ( 143.1451861577818079, 33.85625000108393579, -5.444914386472297529 ) ) ;
#11766 = CARTESIAN_POINT ( 'NONE',  ( 59.37712712842213136, 31.42539062716787157, -13.57481594606304753 ) ) ;
#11767 = CARTESIAN_POINT ( 'NONE',  ( 103.5355339059327093, 80.37500000000000000, 3.535533905932726206 ) ) ;
#11768 = CARTESIAN_POINT ( 'NONE',  ( 5.444914386472297529, 40.30546875108393579, -13.14518615778179900 ) ) ;
#11769 = CARTESIAN_POINT ( 'NONE',  ( -13.14518615778179189, 32.07031250108393294, 5.444914386472304635 ) ) ;
#11770 = CARTESIAN_POINT ( 'NONE',  ( 182.0005117698094352, 35.99999999999999289, 1.999176114741937349 ) ) ;
#11771 = CARTESIAN_POINT ( 'NONE',  ( 95.54126587499996504, 84.68750000136560629, -1.387778780781445676E-14 ) ) ;
#11772 = CARTESIAN_POINT ( 'NONE',  ( 9.598844408820456309, 40.00781250216787299, -9.598844408820458085 ) ) ;
#11773 = AXIS2_PLACEMENT_3D ( 'NONE', #8667, #2122, #19639 ) ;
#11774 = CARTESIAN_POINT ( 'NONE',  ( 200.4449143864723055, 32.36796875108393579, -13.14518615778179900 ) ) ;
#11775 = DIRECTION ( 'NONE',  ( 0.000000000000000000, 1.000000000000000000, 0.000000000000000000 ) ) ;
#11776 = CARTESIAN_POINT ( 'NONE',  ( -13.57481594606304398, 33.21132812716787441, 5.622872871577880183 ) ) ;
#11777 = EDGE_CURVE ( 'NONE', #28027, #8402, #18603, .T. ) ;
#11778 = CARTESIAN_POINT ( 'NONE',  ( 100.8561741729129153, 124.3000000010924708, -2.066987299999999195 ) ) ;
#11779 = CARTESIAN_POINT ( 'NONE',  ( 121.3308878946625384, 36.00000000000000711, -10.16963847934280096 ) ) ;
#11780 = CARTESIAN_POINT ( 'NONE',  ( -13.57481594606304576, 35.44374999999999432, 0.000000000000000000 ) ) ;
#11781 = CARTESIAN_POINT ( 'NONE',  ( 101.7677669209684552, 123.0000000000000000, 1.767766984964258992 ) ) ;
#11782 = CARTESIAN_POINT ( 'NONE',  ( 9.598844408820456309, 33.55859375000000000, -9.598844408820458085 ) ) ;
#11783 = DIRECTION ( 'NONE',  ( -0.000000000000000000, 1.000000000000000000, -0.000000000000000000 ) ) ;
#11784 = CARTESIAN_POINT ( 'NONE',  ( -9.295050272127044266, 35.29492187608393294, 9.295050272127047819 ) ) ;
#11785 = CARTESIAN_POINT ( 'NONE',  ( 5.444914386472302859, 32.86406250108392868, 13.14518615778179189 ) ) ;
#11786 = CARTESIAN_POINT ( 'NONE',  ( 2.414731522848535132E-15, 35.19570312608392726, 13.14518615778179544 ) ) ;
#11787 = EDGE_CURVE ( 'NONE', #23665, #7323, #17842, .T. ) ;
#11788 = CARTESIAN_POINT ( 'NONE',  ( -9.598844408820458085, 37.03125000216787299, -9.598844408820458085 ) ) ;
#11789 = CARTESIAN_POINT ( 'NONE',  ( 112.9999999999999858, 102.0000000000000142, -15.00000000000000711 ) ) ;
#11790 = CARTESIAN_POINT ( 'NONE',  ( 55.70494972787295751, 40.05742187608393579, 9.295050272127047819 ) ) ;
#11791 = CARTESIAN_POINT ( 'NONE',  ( 106.5389055433251002, 114.7507929638356785, -54.17500000273119554 ) ) ;
#11792 = CARTESIAN_POINT ( 'NONE',  ( 92.99999999999998579, 110.0000000000000000, -47.00000000000001421 ) ) ;
#11793 =( BOUNDED_SURFACE ( )  B_SPLINE_SURFACE ( 1, 2, ( 
 ( #19561, #19699, #28121, #25978, #17135, #15120, #12977, #2187, #26117, #43, #15409, #6723, #24125, #21988, #13257, #21713, #8726, #6582, #26408, #2466, #23983, #11127, #4461, #13117, #19841, #328, #9014, #17706, #6867, #9288, #24969, #26693, #7144, #17984, #13974, #1045, #20565, #9717, #7288, #24829, #15838, #469, #5453, #9427, #22702, #18419, #2750, #20269, #13696, #15978, #11413, #22130, #2609, #5169, #5313, #17846, #3169, #22558, #11841, #2882, #13833, #7004, #15698, #19991, #7576, #16271, #22412, #18128, #11553, #7429, #9573, #16123, #27125, #11271, #24401, #755, #26840, #9153, #18278, #13552, #26984, #20133, #26549, #24692, #3025, #11694, #4889, #20417, #24547, #22276, #5030, #612, #903, #5736, #16413, #22983, #6006, #12392, #14263, #16693, #12252, #14403, #7721, #27537, #1599, #5873, #25109, #23257, #5597, #9855, #7860, #25659, #22844, #3450, #23120, #20706, #3594, #18829, #21113, #14671, #1460, #18966, #27673, #20980, #23392, #8137, #12116, #10256, #18562, #14542, #14121, #20842, #3865, #18697, #12526, #21255, #27265, #25246, #16959, #3311, #7994, #1188, #16831, #10117, #1736, #1320, #25527, #27400, #16555, #9988, #10402, #19108, #27816, #8270, #25392, #11982, #3732, #12674, #17667, #21675, #6687, #13226, #14952, #4284, #25943, #9, #23671, #8978, #14807, #17384, #17526, #1878, #8836, #6550, #26228, #15087, #26083, #19248, #27949, #4008, #19810, #293, #6418, #2151, #23806, #19667, #21821, #150, #15374, #24090, #8407, #12941, #10813, #2437, #2297, #25799, #10956, #4149, #21400, #19528, #8694, #15230, #6142, #23948, #10676, #4565, #2008, #21958, #23531, #4429, #17096, #12809, #11097, #13082, #6275, #10541, #21532, #19384, #28089, #8552, #17240, #18096, #9120, #7257, #17814 ),
 ( #17954, #2853, #24662, #26954, #13665, #2993, #11665, #26665, #18247, #20387, #6974, #5137, #22100, #26808, #9686, #15669, #7398, #2721, #16091, #24798, #2580, #9260, #1017, #26375, #11521, #13371, #874, #22380, #5281, #19958, #9545, #11382, #7111, #13802, #4856, #15522, #20103, #11239, #22526, #13523, #13945, #22242, #6832, #582, #20240, #22672, #15946, #26518, #3144, #24369, #435, #15811, #24230, #4711, #24516, #5002, #725, #9397, #11812, #20534, #18934, #5705, #23226, #3702, #9957, #10224, #12364, #27235, #16664, #14094, #18801, #1706, #7690, #27643, #22955, #8103, #16797, #22813, #1288, #21222, #18387, #23087, #5425, #21083, #14371, #25495, #11952, #1571, #3416, #18670, #5840, #25081, #7545, #12085, #3281, #25359, #5569, #14509, #14233, #27093, #20808, #27371, #7830, #5975, #14642, #23361, #3833, #3561, #12495, #16524, #24939, #16242, #12220, #20674, #1158, #16382, #25216, #20948, #1429, #10088, #9823, #18530, #27507, #7963, #6110, #13048, #10782, #21784, #19352, #2115, #23498, #3977, #8238, #24054, #4531, #10646, #25912, #28055, #23911, #26048, #4392, #2264, #10924, #12638, #8521, #6383, #6653, #6517, #1845, #15193, #8378, #16929, #17207, #15056, #23772, #21927, #19494, #14917, #8799, #6247, #19633, #13191, #1977, #21366, #19214, #115, #8660, #10508, #12908, #4249, #21641, #27918, #17063, #25767, #17488, #17351, #23638, #28193, #26187, #15339, #4114, #10365, #19074, #27779, #12779, #25629, #21495, #14777, #24334, #13907, #11061, #22065, #11343, #8940, #22203, #7076, #687, #2953, #17917, #7215, #15905, #2682, #22487, #24623, #11203, #9362, #26339, #2817, #2403, #19918, #11626, #6938, #20350, #835, #6797, #13481, #5242, #19773, #15772, #17629, #5100, #26628, #9504, #24197, #13764 ) ),
 .UNSPECIFIED., .F., .F., .F. ) 
 B_SPLINE_SURFACE_WITH_KNOTS ( ( 2, 2 ),
 ( 3, 2, 2, 2, 2, 2, 2, 2, 2, 2, 2, 2, 2, 2, 2, 2, 2, 2, 2, 2, 2, 2, 2, 2, 2, 2, 2, 2, 2, 2, 2, 2, 2, 2, 2, 2, 2, 2, 2, 2, 2, 2, 2, 2, 2, 2, 2, 2, 2, 2, 2, 2, 2, 2, 2, 2, 2, 2, 2, 2, 2, 2, 2, 2, 2, 2, 2, 2, 2, 2, 2, 2, 2, 2, 2, 2, 2, 2, 2, 2, 2, 2, 2, 2, 2, 2, 2, 2, 2, 2, 2, 2, 2, 2, 2, 2, 2, 2, 2, 2, 2, 2, 2, 2, 2, 2, 2, 2, 2, 2, 2, 2, 3 ),
 ( 0.000000000000000000, 1.000000000000000000 ),
 ( 0.000000000000000000, 0.008928571428571428076, 0.01785714285714285615, 0.02678571428571428423, 0.03571428571428571230, 0.04464285714285714385, 0.05357142857142856845, 0.06250000000000000000, 0.07142857142857142461, 0.08035714285714286309, 0.08928571428571428770, 0.09821428571428571230, 0.1071428571428571369, 0.1160714285714285754, 0.1250000000000000000, 0.1339285714285714246, 0.1428571428571428492, 0.1517857142857142738, 0.1607142857142857262, 0.1696428571428571508, 0.1785714285714285754, 0.1875000000000000000, 0.1964285714285714246, 0.2053571428571428492, 0.2142857142857142738, 0.2232142857142857262, 0.2321428571428571508, 0.2410714285714285754, 0.2500000000000000000, 0.2589285714285714524, 0.2678571428571428492, 0.2767857142857143016, 0.2857142857142856984, 0.2946428571428571508, 0.3035714285714285476, 0.3125000000000000000, 0.3214285714285714524, 0.3303571428571428492, 0.3392857142857143016, 0.3482142857142856984, 0.3571428571428571508, 0.3660714285714285476, 0.3750000000000000000, 0.3839285714285714524, 0.3928571428571428492, 0.4017857142857143016, 0.4107142857142856984, 0.4196428571428571508, 0.4285714285714285476, 0.4375000000000000000, 0.4464285714285714524, 0.4553571428571428492, 0.4642857142857143016, 0.4732142857142856984, 0.4821428571428571508, 0.4910714285714285476, 0.5000000000000000000, 0.5089285714285713969, 0.5178571428571429047, 0.5267857142857143016, 0.5357142857142856984, 0.5446428571428570953, 0.5535714285714286031, 0.5625000000000000000, 0.5714285714285713969, 0.5803571428571429047, 0.5892857142857143016, 0.5982142857142856984, 0.6071428571428570953, 0.6160714285714286031, 0.6250000000000000000, 0.6339285714285713969, 0.6428571428571429047, 0.6517857142857143016, 0.6607142857142856984, 0.6696428571428570953, 0.6785714285714286031, 0.6875000000000000000, 0.6964285714285713969, 0.7053571428571429047, 0.7142857142857143016, 0.7232142857142856984, 0.7321428571428570953, 0.7410714285714286031, 0.7500000000000000000, 0.7589285714285713969, 0.7678571428571429047, 0.7767857142857143016, 0.7857142857142856984, 0.7946428571428570953, 0.8035714285714286031, 0.8125000000000000000, 0.8214285714285713969, 0.8303571428571429047, 0.8392857142857143016, 0.8482142857142856984, 0.8571428571428570953, 0.8660714285714286031, 0.8750000000000000000, 0.8839285714285713969, 0.8928571428571429047, 0.9017857142857143016, 0.9107142857142856984, 0.9196428571428570953, 0.9285714285714286031, 0.9375000000000000000, 0.9464285714285713969, 0.9553571428571429047, 0.9642857142857143016, 0.9732142857142856984, 0.9821428571428570953, 0.9910714285714286031, 1.000000000000000000 ),
 .UNSPECIFIED. ) 
 GEOMETRIC_REPRESENTATION_ITEM ( )  RATIONAL_B_SPLINE_SURFACE ( (
 ( 1.000000000000000000, 0.9238795325112867385, 1.000000000000000000, 0.9238795325112867385, 1.000000000000000000, 0.9238795325112867385, 1.000000000000000000, 0.9238795325112867385, 1.000000000000000000, 0.9238795325112867385, 1.000000000000000000, 0.9238795325112867385, 1.000000000000000000, 0.9238795325112867385, 1.000000000000000000, 0.9238795325112867385, 1.000000000000000000, 0.9238795325112867385, 1.000000000000000000, 0.9238795325112867385, 1.000000000000000000, 0.9238795325112867385, 1.000000000000000000, 0.9238795325112867385, 1.000000000000000000, 0.9238795325112867385, 1.000000000000000000, 0.9238795325112867385, 1.000000000000000000, 0.9238795325112867385, 1.000000000000000000, 0.9238795325112867385, 1.000000000000000000, 0.9238795325112867385, 1.000000000000000000, 0.9238795325112867385, 1.000000000000000000, 0.9238795325112867385, 1.000000000000000000, 0.9238795325112867385, 1.000000000000000000, 0.9238795325112867385, 1.000000000000000000, 0.9238795325112867385, 1.000000000000000000, 0.9238795325112867385, 1.000000000000000000, 0.9238795325112867385, 1.000000000000000000, 0.9238795325112867385, 1.000000000000000000, 0.9238795325112867385, 1.000000000000000000, 0.9238795325112867385, 1.000000000000000000, 0.9238795325112867385, 1.000000000000000000, 0.9238795325112867385, 1.000000000000000000, 0.9238795325112867385, 1.000000000000000000, 0.9238795325112867385, 1.000000000000000000, 0.9238795325112867385, 1.000000000000000000, 0.9238795325112867385, 1.000000000000000000, 0.9238795325112867385, 1.000000000000000000, 0.9238795325112867385, 1.000000000000000000, 0.9238795325112867385, 1.000000000000000000, 0.9238795325112867385, 1.000000000000000000, 0.9238795325112867385, 1.000000000000000000, 0.9238795325112867385, 1.000000000000000000, 0.9238795325112867385, 1.000000000000000000, 0.9238795325112867385, 1.000000000000000000, 0.9238795325112867385, 1.000000000000000000, 0.9238795325112867385, 1.000000000000000000, 0.9238795325112867385, 1.000000000000000000, 0.9238795325112867385, 1.000000000000000000, 0.9238795325112867385, 1.000000000000000000, 0.9238795325112867385, 1.000000000000000000, 0.9238795325112867385, 1.000000000000000000, 0.9238795325112867385, 1.000000000000000000, 0.9238795325112867385, 1.000000000000000000, 0.9238795325112867385, 1.000000000000000000, 0.9238795325112867385, 1.000000000000000000, 0.9238795325112867385, 1.000000000000000000, 0.9238795325112867385, 1.000000000000000000, 0.9238795325112867385, 1.000000000000000000, 0.9238795325112867385, 1.000000000000000000, 0.9238795325112867385, 1.000000000000000000, 0.9238795325112867385, 1.000000000000000000, 0.9238795325112867385, 1.000000000000000000, 0.9238795325112867385, 1.000000000000000000, 0.9238795325112867385, 1.000000000000000000, 0.9238795325112867385, 1.000000000000000000, 0.9238795325112867385, 1.000000000000000000, 0.9238795325112867385, 1.000000000000000000, 0.9238795325112867385, 1.000000000000000000, 0.9238795325112867385, 1.000000000000000000, 0.9238795325112867385, 1.000000000000000000, 0.9238795325112867385, 1.000000000000000000, 0.9238795325112867385, 1.000000000000000000, 0.9238795325112867385, 1.000000000000000000, 0.9238795325112867385, 1.000000000000000000, 0.9238795325112867385, 1.000000000000000000, 0.9238795325112867385, 1.000000000000000000, 0.9238795325112867385, 1.000000000000000000, 0.9238795325112867385, 1.000000000000000000, 0.9238795325112867385, 1.000000000000000000, 0.9238795325112867385, 1.000000000000000000, 0.9238795325112867385, 1.000000000000000000, 0.9238795325112867385, 1.000000000000000000, 0.9238795325112867385, 1.000000000000000000, 0.9238795325112867385, 1.000000000000000000, 0.9238795325112867385, 1.000000000000000000, 0.9238795325112867385, 1.000000000000000000, 0.9238795325112867385, 1.000000000000000000, 0.9238795325112867385, 1.000000000000000000, 0.9238795325112867385, 1.000000000000000000, 0.9238795325112867385, 1.000000000000000000, 0.9238795325112867385, 1.000000000000000000, 0.9238795325112867385, 1.000000000000000000, 0.9238795325112867385, 1.000000000000000000, 0.9238795325112867385, 1.000000000000000000, 0.9238795325112867385, 1.000000000000000000, 0.9238795325112867385, 1.000000000000000000, 0.9238795325112867385, 1.000000000000000000, 0.9238795325112867385, 1.000000000000000000, 0.9238795325112867385, 1.000000000000000000, 0.9238795325112867385, 1.000000000000000000, 0.9238795325112867385, 1.000000000000000000, 0.9238795325112867385, 1.000000000000000000, 0.9238795325112867385, 1.000000000000000000, 0.9238795325112867385, 1.000000000000000000, 0.9238795325112867385, 1.000000000000000000, 0.9238795325112867385, 1.000000000000000000, 0.9238795325112867385, 1.000000000000000000, 0.9238795325112867385, 1.000000000000000000, 0.9238795325112867385, 1.000000000000000000, 0.9238795325112867385, 1.000000000000000000, 0.9238795325112867385, 1.000000000000000000, 0.9238795325112867385, 1.000000000000000000, 0.9238795325112867385, 1.000000000000000000, 0.9238795325112867385, 1.000000000000000000, 0.9238795325112867385, 1.000000000000000000),
 ( 1.000000000000000000, 0.9238795325112867385, 1.000000000000000000, 0.9238795325112867385, 1.000000000000000000, 0.9238795325112867385, 1.000000000000000000, 0.9238795325112867385, 1.000000000000000000, 0.9238795325112867385, 1.000000000000000000, 0.9238795325112867385, 1.000000000000000000, 0.9238795325112867385, 1.000000000000000000, 0.9238795325112867385, 1.000000000000000000, 0.9238795325112867385, 1.000000000000000000, 0.9238795325112867385, 1.000000000000000000, 0.9238795325112867385, 1.000000000000000000, 0.9238795325112867385, 1.000000000000000000, 0.9238795325112867385, 1.000000000000000000, 0.9238795325112867385, 1.000000000000000000, 0.9238795325112867385, 1.000000000000000000, 0.9238795325112867385, 1.000000000000000000, 0.9238795325112867385, 1.000000000000000000, 0.9238795325112867385, 1.000000000000000000, 0.9238795325112867385, 1.000000000000000000, 0.9238795325112867385, 1.000000000000000000, 0.9238795325112867385, 1.000000000000000000, 0.9238795325112867385, 1.000000000000000000, 0.9238795325112867385, 1.000000000000000000, 0.9238795325112867385, 1.000000000000000000, 0.9238795325112867385, 1.000000000000000000, 0.9238795325112867385, 1.000000000000000000, 0.9238795325112867385, 1.000000000000000000, 0.9238795325112867385, 1.000000000000000000, 0.9238795325112867385, 1.000000000000000000, 0.9238795325112867385, 1.000000000000000000, 0.9238795325112867385, 1.000000000000000000, 0.9238795325112867385, 1.000000000000000000, 0.9238795325112867385, 1.000000000000000000, 0.9238795325112867385, 1.000000000000000000, 0.9238795325112867385, 1.000000000000000000, 0.9238795325112867385, 1.000000000000000000, 0.9238795325112867385, 1.000000000000000000, 0.9238795325112867385, 1.000000000000000000, 0.9238795325112867385, 1.000000000000000000, 0.9238795325112867385, 1.000000000000000000, 0.9238795325112867385, 1.000000000000000000, 0.9238795325112867385, 1.000000000000000000, 0.9238795325112867385, 1.000000000000000000, 0.9238795325112867385, 1.000000000000000000, 0.9238795325112867385, 1.000000000000000000, 0.9238795325112867385, 1.000000000000000000, 0.9238795325112867385, 1.000000000000000000, 0.9238795325112867385, 1.000000000000000000, 0.9238795325112867385, 1.000000000000000000, 0.9238795325112867385, 1.000000000000000000, 0.9238795325112867385, 1.000000000000000000, 0.9238795325112867385, 1.000000000000000000, 0.9238795325112867385, 1.000000000000000000, 0.9238795325112867385, 1.000000000000000000, 0.9238795325112867385, 1.000000000000000000, 0.9238795325112867385, 1.000000000000000000, 0.9238795325112867385, 1.000000000000000000, 0.9238795325112867385, 1.000000000000000000, 0.9238795325112867385, 1.000000000000000000, 0.9238795325112867385, 1.000000000000000000, 0.9238795325112867385, 1.000000000000000000, 0.9238795325112867385, 1.000000000000000000, 0.9238795325112867385, 1.000000000000000000, 0.9238795325112867385, 1.000000000000000000, 0.9238795325112867385, 1.000000000000000000, 0.9238795325112867385, 1.000000000000000000, 0.9238795325112867385, 1.000000000000000000, 0.9238795325112867385, 1.000000000000000000, 0.9238795325112867385, 1.000000000000000000, 0.9238795325112867385, 1.000000000000000000, 0.9238795325112867385, 1.000000000000000000, 0.9238795325112867385, 1.000000000000000000, 0.9238795325112867385, 1.000000000000000000, 0.9238795325112867385, 1.000000000000000000, 0.9238795325112867385, 1.000000000000000000, 0.9238795325112867385, 1.000000000000000000, 0.9238795325112867385, 1.000000000000000000, 0.9238795325112867385, 1.000000000000000000, 0.9238795325112867385, 1.000000000000000000, 0.9238795325112867385, 1.000000000000000000, 0.9238795325112867385, 1.000000000000000000, 0.9238795325112867385, 1.000000000000000000, 0.9238795325112867385, 1.000000000000000000, 0.9238795325112867385, 1.000000000000000000, 0.9238795325112867385, 1.000000000000000000, 0.9238795325112867385, 1.000000000000000000, 0.9238795325112867385, 1.000000000000000000, 0.9238795325112867385, 1.000000000000000000, 0.9238795325112867385, 1.000000000000000000, 0.9238795325112867385, 1.000000000000000000, 0.9238795325112867385, 1.000000000000000000, 0.9238795325112867385, 1.000000000000000000, 0.9238795325112867385, 1.000000000000000000, 0.9238795325112867385, 1.000000000000000000, 0.9238795325112867385, 1.000000000000000000, 0.9238795325112867385, 1.000000000000000000, 0.9238795325112867385, 1.000000000000000000, 0.9238795325112867385, 1.000000000000000000, 0.9238795325112867385, 1.000000000000000000, 0.9238795325112867385, 1.000000000000000000, 0.9238795325112867385, 1.000000000000000000, 0.9238795325112867385, 1.000000000000000000, 0.9238795325112867385, 1.000000000000000000, 0.9238795325112867385, 1.000000000000000000, 0.9238795325112867385, 1.000000000000000000, 0.9238795325112867385, 1.000000000000000000, 0.9238795325112867385, 1.000000000000000000, 0.9238795325112867385, 1.000000000000000000, 0.9238795325112867385, 1.000000000000000000, 0.9238795325112867385, 1.000000000000000000, 0.9238795325112867385, 1.000000000000000000, 0.9238795325112867385, 1.000000000000000000) ) ) 
 REPRESENTATION_ITEM ( '' )  SURFACE ( )  );
#11794 = CARTESIAN_POINT ( 'NONE',  ( 130.0000000000000000, 36.00000000000000000, 11.57481594606302799 ) ) ;
#11795 = CARTESIAN_POINT ( 'NONE',  ( 5.622872871577871301, 33.60820312499998863, -13.57481594606304753 ) ) ;
#11796 = CARTESIAN_POINT ( 'NONE',  ( 93.46109445667489979, 114.7507929638356785, -52.07499999726881867 ) ) ;
#11797 = CARTESIAN_POINT ( 'NONE',  ( 143.1451861577818079, 33.21132812608393436, -1.609821015232357215E-15 ) ) ;
#11798 = VERTEX_POINT ( 'NONE', #22884 ) ;
#11799 = CARTESIAN_POINT ( 'NONE',  ( 105.6631189606246295, 114.1144967660473242, -50.80000000000000426 ) ) ;
#11800 = AXIS2_PLACEMENT_3D ( 'NONE', #5948, #3807, #7937 ) ;
#11801 = CARTESIAN_POINT ( 'NONE',  ( 97.92893218813459555, 94.68750000000001421, 5.000000000000046185 ) ) ;
#11802 = CARTESIAN_POINT ( 'NONE',  ( 103.5355339059327093, 79.50000000273119838, 3.535533905932726206 ) ) ;
#11803 = CARTESIAN_POINT ( 'NONE',  ( 97.92893218813452449, 94.31250000000001421, -4.999999999999997335 ) ) ;
#11804 = AXIS2_PLACEMENT_3D ( 'NONE', #23556, #21002, #27698 ) ;
#11805 = CARTESIAN_POINT ( 'NONE',  ( 51.42518405393695957, 38.76757812716787299, 5.622872871577880183 ) ) ;
#11806 = CARTESIAN_POINT ( 'NONE',  ( 97.50236033167490746, 117.6869444889999841, -46.02499999726882152 ) ) ;
#11807 = CARTESIAN_POINT ( 'NONE',  ( 181.8548138422181921, 32.56640625108394005, -5.444914386472297529 ) ) ;
#11808 = CARTESIAN_POINT ( 'NONE',  ( -5.622872871577873077, 40.15664062716787441, -13.57481594606304753 ) ) ;
#11809 = VERTEX_POINT ( 'NONE', #25567 ) ;
#11810 = CARTESIAN_POINT ( 'NONE',  ( 182.4334932752013287, 36.00000000000000000, -4.295155080288603600 ) ) ;
#11811 = VECTOR ( 'NONE', #18573, 1000.000000000000000 ) ;
#11812 = CARTESIAN_POINT ( 'NONE',  ( 103.5355339059327093, -3.535533905932726206, 11.37500000000000000 ) ) ;
#11813 = ORIENTED_EDGE ( 'NONE', *, *, #10331, .F. ) ;
#11814 = CARTESIAN_POINT ( 'NONE',  ( -5.444914386472297529, 36.63437500108393152, -13.14518615778179900 ) ) ;
#11815 = CARTESIAN_POINT ( 'NONE',  ( 208.5748159460630120, 31.92148437716787512, 5.622872871577869525 ) ) ;
#11816 = CARTESIAN_POINT ( 'NONE',  ( -13.14518615778179189, 32.66562500108393863, 5.444914386472304635 ) ) ;
#11817 = CARTESIAN_POINT ( 'NONE',  ( 103.5355339059327093, 3.535533905932755072, 0.7500000027311857220 ) ) ;
#11818 = DIRECTION ( 'NONE',  ( 0.000000000000000000, 1.000000000000000000, 0.000000000000000000 ) ) ;
#11819 = CARTESIAN_POINT ( 'NONE',  ( -13.14518615778179544, 32.02070312608393010, 0.000000000000000000 ) ) ;
#11820 = CARTESIAN_POINT ( 'NONE',  ( 120.7049497278729575, 32.71523437608393436, 9.295050272127047819 ) ) ;
#11821 = CARTESIAN_POINT ( 'NONE',  ( 95.54126587500000767, 90.81249999863440792, -7.484931351350258973E-15 ) ) ;
#11822 = CARTESIAN_POINT ( 'NONE',  ( 101.7677669529663547, 124.7000000000000028, -1.767766952966370209 ) ) ;
#11823 = CARTESIAN_POINT ( 'NONE',  ( 130.0000000000000000, 0.000000000000000000, 0.000000000000000000 ) ) ;
#11824 = CARTESIAN_POINT ( 'NONE',  ( 9.598844408820456309, 36.03906250216787299, -9.598844408820458085 ) ) ;
#11825 = CARTESIAN_POINT ( 'NONE',  ( 95.54126587499995082, 1.846868145590750077, 5.625000001365593860 ) ) ;
#11826 = CARTESIAN_POINT ( 'NONE',  ( 51.85481384221820633, 40.55351562608393579, 0.000000000000000000 ) ) ;
#11827 = CARTESIAN_POINT ( 'NONE',  ( 104.4587341249999781, -1.846868145590721655, 10.87500000136559208 ) ) ;
#11828 = CARTESIAN_POINT ( 'NONE',  ( 97.50236033167492167, 102.3130555110000159, -44.72500000273119980 ) ) ;
#11829 = CARTESIAN_POINT ( 'NONE',  ( 104.4587341249999923, 90.62499999863439371, -1.846868145590737198 ) ) ;
#11830 = CARTESIAN_POINT ( 'NONE',  ( 181.4251840539369596, 40.30546875216787583, 0.000000000000000000 ) ) ;
#11831 = CARTESIAN_POINT ( 'NONE',  ( 97.50236033167490746, 102.3130555110000159, -53.22499999726882436 ) ) ;
#11832 = CARTESIAN_POINT ( 'NONE',  ( 13.14518615778179900, 34.05468750108394005, -5.444914386472297529 ) ) ;
#11833 = ORIENTED_EDGE ( 'NONE', *, *, #12749, .T. ) ;
#11834 = CARTESIAN_POINT ( 'NONE',  ( 0.000000000000000000, 11.00000000000000355, 0.000000000000000000 ) ) ;
#11835 = CARTESIAN_POINT ( 'NONE',  ( 2.493653234604083739E-15, 39.71015625216787015, 13.57481594606304576 ) ) ;
#11836 = DIRECTION ( 'NONE',  ( -0.000000000000000000, -1.000000000000000000, -0.000000000000000000 ) ) ;
#11837 =( BOUNDED_CURVE ( )  B_SPLINE_CURVE ( 2, ( #22684, #3154, #11824, #20401, #27107, #25095, #1171, #11965, #7558 ),
 .UNSPECIFIED., .F., .F. ) 
 B_SPLINE_CURVE_WITH_KNOTS ( ( 3, 2, 2, 2, 3 ),
 ( 0.4375000000000003331, 0.4479166666666669627, 0.4583333333333335369, 0.4687500000000001665, 0.4791666666666667962 ),
 .UNSPECIFIED. ) 
 CURVE ( )  GEOMETRIC_REPRESENTATION_ITEM ( )  RATIONAL_B_SPLINE_CURVE ( ( 0.9999999999999975575, 0.9238795325112891810, 1.000000000000000000, 0.9238795325112867385, 1.000000000000000000, 0.9238795325112867385, 1.000000000000000000, 0.9238795325112859613, 1.000000000000000888 ) ) 
 REPRESENTATION_ITEM ( '' )  );
#11838 = CARTESIAN_POINT ( 'NONE',  ( 200.4449143864723055, 35.24531250108393010, 13.14518615778179189 ) ) ;
#11839 = VERTEX_POINT ( 'NONE', #19005 ) ;
#11840 = CARTESIAN_POINT ( 'NONE',  ( 194.2761280619777153, 53.51529642094860861, -15.00000000000000000 ) ) ;
#11841 = CARTESIAN_POINT ( 'NONE',  ( 103.1528011352953342, -3.152801135295355106, 11.06250000136559208 ) ) ;
#11842 = VECTOR ( 'NONE', #1689, 1000.000000000000000 ) ;
#11843 = EDGE_LOOP ( 'NONE', ( #22158, #26767, #5447, #24228, #16169, #10493, #1628 ) ) ;
#11844 = CARTESIAN_POINT ( 'NONE',  ( 108.0825317500000011, 112.6261737610028320, -50.27500000273119696 ) ) ;
#11845 = CARTESIAN_POINT ( 'NONE',  ( -13.14518615778179544, 37.37851562608393863, 0.000000000000000000 ) ) ;
#11846 = LINE ( 'NONE', #1465, #28165 ) ;
#11847 = CARTESIAN_POINT ( 'NONE',  ( 94.99999999999995737, 1.387778780781445676E-14, 14.12500000273118594 ) ) ;
#11848 = CARTESIAN_POINT ( 'NONE',  ( 130.0000000000000000, 37.18007812608393436, -13.14518615778179544 ) ) ;
#11849 = CARTESIAN_POINT ( 'NONE',  ( 13.14518615778179722, 38.71796875108393721, 5.444914386472293977 ) ) ;
#11850 = CARTESIAN_POINT ( 'NONE',  ( -5.444914386472297529, 35.64218750108392442, -13.14518615778179900 ) ) ;
#11851 = CARTESIAN_POINT ( 'NONE',  ( 99.99999999999998579, 91.31249999863440792, 4.458734124999981674 ) ) ;
#11852 = LINE ( 'NONE', #25540, #11811 ) ;
#11853 = CARTESIAN_POINT ( 'NONE',  ( 97.50236033167492167, 102.3130555110000159, -50.97500000273119980 ) ) ;
#11854 = DIRECTION ( 'NONE',  ( 0.000000000000000000, 0.000000000000000000, -1.000000000000000000 ) ) ;
#11855 = CARTESIAN_POINT ( 'NONE',  ( 13.14518615778179544, 36.38632812608393863, -1.609821015232357215E-15 ) ) ;
#11856 = CARTESIAN_POINT ( 'NONE',  ( 98.15313185440923860, 4.458734125000016313, 5.500000001365592972 ) ) ;
#11857 = CARTESIAN_POINT ( 'NONE',  ( 55.70494972787295751, 36.48554687608393721, -9.295050272127046043 ) ) ;
#11858 = DIRECTION ( 'NONE',  ( 1.000000000000000000, 0.000000000000000000, 0.000000000000000000 ) ) ;
#11859 = CARTESIAN_POINT ( 'NONE',  ( 59.37712712842216689, 38.76757812499998579, 13.57481594606308128 ) ) ;
#11860 = CARTESIAN_POINT ( 'NONE',  ( 208.1451861577818079, 36.13828125108393152, 5.444914386472293977 ) ) ;
#11861 = CARTESIAN_POINT ( 'NONE',  ( 2.414731522848535132E-15, 33.80664062608393294, 13.14518615778179544 ) ) ;
#11862 = CARTESIAN_POINT ( 'NONE',  ( 98.53841926354351699, 123.6500000010924794, -1.461580736456474794 ) ) ;
#11863 = CARTESIAN_POINT ( 'NONE',  ( 103.1528011352953484, 91.43749999863440792, 3.152801135295352886 ) ) ;
#11864 = CARTESIAN_POINT ( 'NONE',  ( 204.2950502721270425, 38.07304687608393579, -9.295050272127046043 ) ) ;
#11865 = CARTESIAN_POINT ( 'NONE',  ( 108.0825317500000011, 110.0000000000000000, -50.87499999726882294 ) ) ;
#11866 = EDGE_CURVE ( 'NONE', #27029, #3371, #14591, .T. ) ;
#11867 = CARTESIAN_POINT ( 'NONE',  ( 5.622872871577871301, 33.60820312499998863, -13.57481594606304753 ) ) ;
#11868 = CARTESIAN_POINT ( 'NONE',  ( 9.295050272127046043, 34.69960937608393436, -9.295050272127046043 ) ) ;
#11869 = ORIENTED_EDGE ( 'NONE', *, *, #25266, .T. ) ;
#11870 = CARTESIAN_POINT ( 'NONE',  ( 200.6228728715777834, 37.67617187716787441, -13.57481594606313990 ) ) ;
#11871 = CARTESIAN_POINT ( 'NONE',  ( 55.70494972787295751, 39.85898437608393152, -9.295050272127046043 ) ) ;
#11872 = CARTESIAN_POINT ( 'NONE',  ( 185.7049497278729575, 33.70742187608393436, 9.295050272127047819 ) ) ;
#11873 = VERTEX_POINT ( 'NONE', #6052 ) ;
#11874 = DIRECTION ( 'NONE',  ( -0.8660254037844418162, 0.4999999999999947264, -0.000000000000000000 ) ) ;
#11875 =( BOUNDED_CURVE ( )  B_SPLINE_CURVE ( 2, ( #19223, #6253, #21504, #14926, #23646, #28061, #21649, #1984, #10788 ),
 .UNSPECIFIED., .F., .F. ) 
 B_SPLINE_CURVE_WITH_KNOTS ( ( 3, 2, 2, 2, 3 ),
 ( 0.6428571428571427937, 0.6517857142857141906, 0.6607142857142855874, 0.6696428571428569843, 0.6785714285714284921 ),
 .UNSPECIFIED. ) 
 CURVE ( )  GEOMETRIC_REPRESENTATION_ITEM ( )  RATIONAL_B_SPLINE_CURVE ( ( 1.000000000000000888, 0.9238795325112857393, 1.000000000000000000, 0.9238795325112867385, 1.000000000000000000, 0.9238795325112867385, 1.000000000000000000, 0.9238795325112877377, 0.9999999999999990008 ) ) 
 REPRESENTATION_ITEM ( '' )  );
#11876 = CARTESIAN_POINT ( 'NONE',  ( 2.493653234604083739E-15, 34.05468749999999289, 13.57481594606304576 ) ) ;
#11877 = CARTESIAN_POINT ( 'NONE',  ( 120.4011555911795455, 38.81718750216787583, 9.598844408820459861 ) ) ;
#11878 = DIRECTION ( 'NONE',  ( 0.000000000000000000, -1.000000000000000000, -0.000000000000000000 ) ) ;
#11879 = CARTESIAN_POINT ( 'NONE',  ( -9.598844408820458085, 34.65000000216787868, -9.598844408820458085 ) ) ;
#11880 = CARTESIAN_POINT ( 'NONE',  ( 185.7049497278729575, 40.65273437608393436, -9.295050272127046043 ) ) ;
#11881 = ORIENTED_EDGE ( 'NONE', *, *, #8674, .T. ) ;
#11882 = CARTESIAN_POINT ( 'NONE',  ( 96.84719886470459471, 3.152801135295383084, 3.312500001365592972 ) ) ;
#11883 = ORIENTED_EDGE ( 'NONE', *, *, #19952, .F. ) ;
#11884 = CARTESIAN_POINT ( 'NONE',  ( 92.45873412499997812, 110.0000000000000000, -45.31249999863441502 ) ) ;
#11885 = CARTESIAN_POINT ( 'NONE',  ( 103.1528011352953342, -3.152801135295355106, 3.812500001365591640 ) ) ;
#11886 = DIRECTION ( 'NONE',  ( 0.000000000000000000, 0.000000000000000000, -1.000000000000000000 ) ) ;
#11887 = CARTESIAN_POINT ( 'NONE',  ( -8.125303917791546482, 36.00000000000000711, 10.34220695173551263 ) ) ;
#11888 = CARTESIAN_POINT ( 'NONE',  ( 78.57481594606305464, 37.47773437716787015, 5.622872871577868636 ) ) ;
#11889 = CARTESIAN_POINT ( 'NONE',  ( -18.00000000000000711, 78.00000000000000000, 2.081668171172169302E-15 ) ) ;
#11890 = ADVANCED_FACE ( 'NONE', ( #5496 ), #14716, .T. ) ;
#11891 = CARTESIAN_POINT ( 'NONE',  ( 91.91746824999998466, 107.3738262389971538, -47.02500000273118275 ) ) ;
#11892 = CARTESIAN_POINT ( 'NONE',  ( 101.0355339059327235, 123.1500000000000057, -2.500000000000001776 ) ) ;
#11893 = CARTESIAN_POINT ( 'NONE',  ( 219.9999999999999716, 50.00000000000000000, -10.00000000000000000 ) ) ;
#11894 = CARTESIAN_POINT ( 'NONE',  ( 6.412866676253258014, 50.00000000108448006, 11.99502265407631185 ) ) ;
#11895 = CARTESIAN_POINT ( 'NONE',  ( 139.5988444088204403, 40.70234374999999716, -9.598844408820458085 ) ) ;
#11896 = CARTESIAN_POINT ( 'NONE',  ( 139.5988444088204403, 32.76484374999999716, -9.598844408820458085 ) ) ;
#11897 = ORIENTED_EDGE ( 'NONE', *, *, #8245, .T. ) ;
#11898 = VERTEX_POINT ( 'NONE', #9893 ) ;
#11899 = CARTESIAN_POINT ( 'NONE',  ( 99.99999999999998579, 128.0000000000000000, 2.500000000000003553 ) ) ;
#11900 = CARTESIAN_POINT ( 'NONE',  ( -5.444914386472297529, 35.04687500108393294, -13.14518615778179900 ) ) ;
#11901 = CARTESIAN_POINT ( 'NONE',  ( -5.622872871577873077, 35.39414062716787157, -13.57481594606304753 ) ) ;
#11902 = CARTESIAN_POINT ( 'NONE',  ( 102.0710678118654329, -4.999999999999989342, 5.437500002731184168 ) ) ;
#11903 = CARTESIAN_POINT ( 'NONE',  ( 124.5550856135277087, 31.97109375108393436, 13.14518615778179722 ) ) ;
#11904 = EDGE_CURVE ( 'NONE', #26666, #8864, #17324, .T. ) ;
#11905 = CARTESIAN_POINT ( 'NONE',  ( 65.00000000000000000, 32.16953125216787157, -13.57481594606304576 ) ) ;
#11906 = EDGE_CURVE ( 'NONE', #18097, #6897, #27436, .T. ) ;
#11907 = CARTESIAN_POINT ( 'NONE',  ( 13.57481594606304753, 37.57695312716787583, -5.622872871577873966 ) ) ;
#11908 = CARTESIAN_POINT ( 'NONE',  ( 13.14518615778179900, 37.82500000108392868, -5.444914386472297529 ) ) ;
#11909 = EDGE_CURVE ( 'NONE', #3132, #15219, #23159, .T. ) ;
#11910 = DIRECTION ( 'NONE',  ( 0.000000000000000000, -1.000000000000000000, 0.000000000000000000 ) ) ;
#11911 = CARTESIAN_POINT ( 'NONE',  ( 182.2616098421445656, 36.00000000000000000, 3.273369733618571420 ) ) ;
#11912 = CARTESIAN_POINT ( 'NONE',  ( 93.46109445667489979, 105.2492070361643215, -51.67499999726882010 ) ) ;
#11913 = VERTEX_POINT ( 'NONE', #3909 ) ;
#11914 = CARTESIAN_POINT ( 'NONE',  ( -13.57481594606304576, 37.97382812716787726, 5.622872871577880183 ) ) ;
#11915 = CARTESIAN_POINT ( 'NONE',  ( 185.7049497278729575, 31.72304687608393081, -9.295050272127046043 ) ) ;
#11916 = CARTESIAN_POINT ( 'NONE',  ( 99.99999999999998579, 124.3999999999999915, 2.499999999999978684 ) ) ;
#11917 = CARTESIAN_POINT ( 'NONE',  ( 101.0355339059327378, 123.9569999999781515, -2.499999999999997780 ) ) ;
#11918 = EDGE_CURVE ( 'NONE', #444, #10301, #7900, .T. ) ;
#11919 = SURFACE_STYLE_FILL_AREA ( #3252 ) ;
#11920 = CARTESIAN_POINT ( 'NONE',  ( 185.4011555911795597, 39.51171874999999289, 9.598844408820459861 ) ) ;
#11921 = CARTESIAN_POINT ( 'NONE',  ( 112.9999999999999858, 97.00000000000000000, 12.99999999999999289 ) ) ;
#11922 = DIRECTION ( 'NONE',  ( 1.000000000000000000, 0.000000000000000000, -0.000000000000000000 ) ) ;
#11923 = CARTESIAN_POINT ( 'NONE',  ( -9.598844408820454532, 35.54296874999999289, 9.598844408820459861 ) ) ;
#11924 = CARTESIAN_POINT ( 'NONE',  ( -5.622872871578010745, 32.91367187499999858, -13.57481594606290898 ) ) ;
#11925 = CARTESIAN_POINT ( 'NONE',  ( 5.444914386472297529, 34.94765625108394147, -13.14518615778179900 ) ) ;
#11926 = CARTESIAN_POINT ( 'NONE',  ( -13.14518615778179900, 33.36015625108393579, -5.444914386472297529 ) ) ;
#11927 = CARTESIAN_POINT ( 'NONE',  ( -13.14518615778179722, 34.15390625108393863, -5.444914386472297529 ) ) ;
#11928 = CARTESIAN_POINT ( 'NONE',  ( -8.312177448680279460E-16, 35.34453125216787583, -13.57481594606304576 ) ) ;
#11929 = CARTESIAN_POINT ( 'NONE',  ( 195.0000000000000000, 36.03906250000000000, -13.57481594606304576 ) ) ;
#11930 = DIRECTION ( 'NONE',  ( 0.000000000000000000, 4.625929269271485914E-16, 1.000000000000000000 ) ) ;
#11931 = CARTESIAN_POINT ( 'NONE',  ( 78.14518615778179367, 33.01289062608393010, -1.609821015232357215E-15 ) ) ;
#11932 = LINE ( 'NONE', #5262, #16223 ) ;
#11933 = DIRECTION ( 'NONE',  ( 0.000000000000000000, 1.000000000000000000, 0.000000000000000000 ) ) ;
#11934 = ORIENTED_EDGE ( 'NONE', *, *, #4292, .T. ) ;
#11935 = CARTESIAN_POINT ( 'NONE',  ( 9.598844408820456309, 37.52734375000000000, -9.598844408820458085 ) ) ;
#11936 = CARTESIAN_POINT ( 'NONE',  ( -13.57481594606304753, 33.01289062500000426, -5.622872871577873077 ) ) ;
#11937 = CARTESIAN_POINT ( 'NONE',  ( 95.00472066334982912, 116.8754121666685393, -54.17499999726881299 ) ) ;
#11938 = CARTESIAN_POINT ( 'NONE',  ( 116.8548138422182205, 35.98945312608393721, 0.000000000000000000 ) ) ;
#11939 = ADVANCED_FACE ( 'NONE', ( #12570 ), #27718, .F. ) ;
#11940 = EDGE_LOOP ( 'NONE', ( #23039, #4612, #9169, #13434 ) ) ;
#11941 = CARTESIAN_POINT ( 'NONE',  ( 102.1631189606246295, 116.6573956140660897, -50.60000000000000853 ) ) ;
#11942 = CARTESIAN_POINT ( 'NONE',  ( 200.6228728715779255, 36.58476562716786873, 13.57481594606297115 ) ) ;
#11943 = CARTESIAN_POINT ( 'NONE',  ( 104.4587341249999781, 81.87500000136559208, 1.846868145590721655 ) ) ;
#11944 = CARTESIAN_POINT ( 'NONE',  ( 104.9999999999999716, 92.93749999999998579, 2.071067811865467956 ) ) ;
#11945 = CARTESIAN_POINT ( 'NONE',  ( 59.37712712842213136, 40.15664062716787441, -13.57481594606304753 ) ) ;
#11946 = CARTESIAN_POINT ( 'NONE',  ( 93.46109445667489979, 114.7507929638356785, -45.82499999726881867 ) ) ;
#11947 = CARTESIAN_POINT ( 'NONE',  ( 185.7049497278729575, 39.85898437608393152, -9.295050272127046043 ) ) ;
#11948 = CARTESIAN_POINT ( 'NONE',  ( -8.312177448680279460E-16, 39.31328125216787583, -13.57481594606304576 ) ) ;
#11949 = ORIENTED_EDGE ( 'NONE', *, *, #9027, .F. ) ;
#11950 = EDGE_CURVE ( 'NONE', #20336, #10673, #5637, .T. ) ;
#11951 = AXIS2_PLACEMENT_3D ( 'NONE', #6813, #15502, #4840 ) ;
#11952 = CARTESIAN_POINT ( 'NONE',  ( 103.5355339059327093, 3.535533905932755072, 9.624999999999998224 ) ) ;
#11953 = VERTEX_POINT ( 'NONE', #12155 ) ;
#11954 = CARTESIAN_POINT ( 'NONE',  ( -13.14518615778179544, 33.60820312608393579, 0.000000000000000000 ) ) ;
#11955 = CARTESIAN_POINT ( 'NONE',  ( 208.1451861577817795, 39.41250000108393436, -5.444914386472297529 ) ) ;
#11956 =( BOUNDED_CURVE ( )  B_SPLINE_CURVE ( 2, ( #27282, #7739, #25680, #25966, #2031, #12830, #14829, #12966, #27556 ),
 .UNSPECIFIED., .F., .F. ) 
 B_SPLINE_CURVE_WITH_KNOTS ( ( 3, 2, 2, 2, 3 ),
 ( 0.4285714285714285476, 0.4375000000000000000, 0.4464285714285713969, 0.4553571428571427937, 0.4642857142857142461 ),
 .UNSPECIFIED. ) 
 CURVE ( )  GEOMETRIC_REPRESENTATION_ITEM ( )  RATIONAL_B_SPLINE_CURVE ( ( 1.000000000000000000, 0.9238795325112867385, 1.000000000000000000, 0.9238795325112867385, 1.000000000000000000, 0.9238795325112867385, 1.000000000000000000, 0.9238795325112871826, 0.9999999999999995559 ) ) 
 REPRESENTATION_ITEM ( '' )  );
#11957 = CARTESIAN_POINT ( 'NONE',  ( 0.000000000000000000, -7.395377635281828788, 0.000000000000000000 ) ) ;
#11958 = CARTESIAN_POINT ( 'NONE',  ( 99.99999999999995737, 5.000000000000018652, 0.8750000027311858330 ) ) ;
#11959 = DIRECTION ( 'NONE',  ( 0.8660254037844392627, -0.000000000000000000, -0.4999999999999987788 ) ) ;
#11960 = CARTESIAN_POINT ( 'NONE',  ( 13.14518615778179544, 33.21132812608393436, -1.609821015232357215E-15 ) ) ;
#11961 = CARTESIAN_POINT ( 'NONE',  ( 99.99999999999995737, 5.000000000000018652, 11.87500000273118594 ) ) ;
#11962 = CARTESIAN_POINT ( 'NONE',  ( 65.00000000000000000, 32.07031249999999289, -13.57481594606304576 ) ) ;
#11963 = CARTESIAN_POINT ( 'NONE',  ( 97.50000000000000000, 124.1499999999999915, -1.035533905932742416 ) ) ;
#11964 = DIRECTION ( 'NONE',  ( 0.000000000000000000, 0.000000000000000000, 1.000000000000000000 ) ) ;
#11965 = CARTESIAN_POINT ( 'NONE',  ( 5.622872871577832221, 35.79101562716787299, 13.57481594606309194 ) ) ;
#11966 = CARTESIAN_POINT ( 'NONE',  ( 95.54126587499995082, -1.846868145590724986, 6.750000001365592972 ) ) ;
#11967 = LINE ( 'NONE', #20690, #17141 ) ;
#11968 = CARTESIAN_POINT ( 'NONE',  ( 101.8468681455907046, 4.458734125000016313, 11.12500000136559208 ) ) ;
#11969 = CARTESIAN_POINT ( 'NONE',  ( 105.6631189606246295, 105.8855032339526758, -49.70000000546237828 ) ) ;
#11970 = FACE_OUTER_BOUND ( 'NONE', #18695, .T. ) ;
#11971 = LINE ( 'NONE', #25235, #25742 ) ;
#11972 = CARTESIAN_POINT ( 'NONE',  ( 104.9952793366501567, 116.8754121666685393, -54.32499999726881867 ) ) ;
#11973 = CARTESIAN_POINT ( 'NONE',  ( 5.444914386472297529, 32.56640625108394005, -13.14518615778179900 ) ) ;
#11974 = CIRCLE ( 'NONE', #18800, 7.000000000000006217 ) ;
#11975 = ORIENTED_EDGE ( 'NONE', *, *, #7194, .F. ) ;
#11976 = CARTESIAN_POINT ( 'NONE',  ( 124.3771271284222877, 36.88242187499999858, -13.57481594606318254 ) ) ;
#11977 = DIRECTION ( 'NONE',  ( -1.000000000000000000, 0.000000000000000000, 7.228014483236696740E-18 ) ) ;
#11978 = ADVANCED_FACE ( 'NONE', ( #10157 ), #10444, .F. ) ;
#11979 = CARTESIAN_POINT ( 'NONE',  ( 208.1451861577817795, 32.96328125108393436, 5.444914386472293977 ) ) ;
#11980 = ORIENTED_EDGE ( 'NONE', *, *, #27445, .T. ) ;
#11981 = DIRECTION ( 'NONE',  ( -0.000000000000000000, -1.000000000000000000, -0.000000000000000000 ) ) ;
#11982 = CARTESIAN_POINT ( 'NONE',  ( 101.8468681455906903, -4.458734124999987891, 5.000000001365592972 ) ) ;
#11983 = ORIENTED_EDGE ( 'NONE', *, *, #24799, .F. ) ;
#11984 = CARTESIAN_POINT ( 'NONE',  ( 108.0825317500000011, 107.3738262389971538, -50.47500000273118559 ) ) ;
#11985 = CARTESIAN_POINT ( 'NONE',  ( 2.414731522848535132E-15, 36.78320312608393294, 13.14518615778179544 ) ) ;
#11986 = CARTESIAN_POINT ( 'NONE',  ( 181.4251840539369596, 39.46210937716787726, -5.622872871577873077 ) ) ;
#11987 = FACE_OUTER_BOUND ( 'NONE', #8546, .T. ) ;
#11988 = CARTESIAN_POINT ( 'NONE',  ( 116.8548138422182063, 37.32890625108393579, -5.444914386472297529 ) ) ;
#11989 = CARTESIAN_POINT ( 'NONE',  ( 5.444914386472297529, 38.12265625108393863, -13.14518615778179722 ) ) ;
#11990 = AXIS2_PLACEMENT_3D ( 'NONE', #15878, #4786, #24302 ) ;
#11991 = CARTESIAN_POINT ( 'NONE',  ( -9.295050272127044266, 32.71523437608393436, 9.295050272127047819 ) ) ;
#11992 = CARTESIAN_POINT ( 'NONE',  ( 95.54126587499999346, 91.12499999863439371, 1.846868145590722543 ) ) ;
#11993 = FACE_OUTER_BOUND ( 'NONE', #3056, .T. ) ;
#11994 = CARTESIAN_POINT ( 'NONE',  ( 96.46446609406721961, 3.535533905932755072, 4.000000002731185056 ) ) ;
#11995 = CARTESIAN_POINT ( 'NONE',  ( 104.4587341249999639, 1.442382525525748735E-14, 6.187500001365592084 ) ) ;
#11996 = CARTESIAN_POINT ( 'NONE',  ( 99.99999999999995737, 82.43750000136559208, -4.458734125000016313 ) ) ;
#11997 = CARTESIAN_POINT ( 'NONE',  ( 99.99999999999998579, 97.00000000000000000, -2.999999999999996447 ) ) ;
#11998 = DIRECTION ( 'NONE',  ( -0.000000000000000000, 1.000000000000000000, -0.000000000000000000 ) ) ;
#11999 = ORIENTED_EDGE ( 'NONE', *, *, #16443, .T. ) ;
#12000 = CARTESIAN_POINT ( 'NONE',  ( 9.295050272127047819, 36.28710937608393294, 9.295050272127046043 ) ) ;
#12001 =( BOUNDED_CURVE ( )  B_SPLINE_CURVE ( 2, ( #22503, #11643, #20219, #13500, #13645, #22360, #15924, #16218, #20651 ),
 .UNSPECIFIED., .F., .F. ) 
 B_SPLINE_CURVE_WITH_KNOTS ( ( 3, 2, 2, 2, 3 ),
 ( 0.4375000000000003331, 0.4479166666666669627, 0.4583333333333335369, 0.4687500000000001665, 0.4791666666666667962 ),
 .UNSPECIFIED. ) 
 CURVE ( )  GEOMETRIC_REPRESENTATION_ITEM ( )  RATIONAL_B_SPLINE_CURVE ( ( 0.9999999999999975575, 0.9238795325112891810, 1.000000000000000000, 0.9238795325112867385, 1.000000000000000000, 0.9238795325112867385, 1.000000000000000000, 0.9238795325112859613, 1.000000000000000888 ) ) 
 REPRESENTATION_ITEM ( '' )  );
#12002 = CARTESIAN_POINT ( 'NONE',  ( 99.14382582708707048, 122.8000000010924708, -2.066987299999999195 ) ) ;
#12003 = CARTESIAN_POINT ( 'NONE',  ( 96.84719886470463734, 92.93749999863440792, -3.152801135295366208 ) ) ;
#12004 = CARTESIAN_POINT ( 'NONE',  ( 13.57481594606304576, 31.97109375216787441, -1.662435489736055892E-15 ) ) ;
#12005 = CARTESIAN_POINT ( 'NONE',  ( 108.0825317500000011, 110.0000000000000000, -48.87499999726882294 ) ) ;
#12006 = CARTESIAN_POINT ( 'NONE',  ( 124.3771271284221172, 39.66054687716787441, 13.57481594606302444 ) ) ;
#12007 = CARTESIAN_POINT ( 'NONE',  ( 2.493653234604083739E-15, 33.26093749999999716, 13.57481594606304576 ) ) ;
#12008 = VERTEX_POINT ( 'NONE', #16734 ) ;
#12009 = CARTESIAN_POINT ( 'NONE',  ( 65.00000000000000000, 52.00000000000000711, -7.517135062566165128E-15 ) ) ;
#12010 = CARTESIAN_POINT ( 'NONE',  ( 102.0710678118654329, -4.999999999999989342, 0.4375000027311854445 ) ) ;
#12011 = CARTESIAN_POINT ( 'NONE',  ( 101.4615807364564546, 122.8500000010924680, -1.461580736456474794 ) ) ;
#12012 = CARTESIAN_POINT ( 'NONE',  ( 200.4449143864723055, 33.06250000108393294, 13.14518615778179189 ) ) ;
#12013 = ORIENTED_EDGE ( 'NONE', *, *, #24846, .F. ) ;
#12014 = LINE ( 'NONE', #8173, #6152 ) ;
#12015 = VECTOR ( 'NONE', #1869, 1000.000000000000000 ) ;
#12016 = CARTESIAN_POINT ( 'NONE',  ( 3.716534113787486771, 51.46663580899624435, -15.00000000000203215 ) ) ;
#12017 = CARTESIAN_POINT ( 'NONE',  ( 193.3947281234233913, 53.60388944777321285, 14.99999999999995559 ) ) ;
#12018 = CARTESIAN_POINT ( 'NONE',  ( 143.5748159460630688, 36.73359375216787015, -1.662435489736055892E-15 ) ) ;
#12019 = DIRECTION ( 'NONE',  ( -0.000000000000000000, 1.000000000000000000, -0.000000000000000000 ) ) ;
#12020 = DIRECTION ( 'NONE',  ( 0.000000000000000000, 0.000000000000000000, -1.000000000000000000 ) ) ;
#12021 = CARTESIAN_POINT ( 'NONE',  ( 200.4449143864723055, 38.61875000108393152, 13.14518615778179189 ) ) ;
#12022 = ORIENTED_EDGE ( 'NONE', *, *, #27964, .F. ) ;
#12023 = ADVANCED_FACE ( 'NONE', ( #25433, #3774 ), #27172, .F. ) ;
#12024 =( NAMED_UNIT ( * ) PLANE_ANGLE_UNIT ( ) SI_UNIT ( $, .RADIAN. ) );
#12025 = CARTESIAN_POINT ( 'NONE',  ( 99.99999999999995737, -4.458734124999988779, 2.687500001365592528 ) ) ;
#12026 = CARTESIAN_POINT ( 'NONE',  ( -10.54595693695916125, 36.00000000000001421, -8.172591659953413412 ) ) ;
#12027 = CARTESIAN_POINT ( 'NONE',  ( 97.92893218813455292, 92.56249999726880162, 5.000000000000003553 ) ) ;
#12028 = DIRECTION ( 'NONE',  ( 0.000000000000000000, -0.000000000000000000, 1.000000000000000000 ) ) ;
#12029 = CARTESIAN_POINT ( 'NONE',  ( 74.29505027212704249, 32.51679687608393721, -9.295050272127046043 ) ) ;
#12030 = CARTESIAN_POINT ( 'NONE',  ( 9.295050272127047819, 40.25585937608393294, 9.295050272127046043 ) ) ;
#12031 = CARTESIAN_POINT ( 'NONE',  ( -9.598844408820454532, 39.61093750216787868, 9.598844408820459861 ) ) ;
#12032 = CARTESIAN_POINT ( 'NONE',  ( 214.9999999999999716, 75.00000000000000000, 9.999999999999946709 ) ) ;
#12033 = CARTESIAN_POINT ( 'NONE',  ( 99.99999999999998579, 110.0000000000000000, -145.0000000000000284 ) ) ;
#12034 = CARTESIAN_POINT ( 'NONE',  ( 130.0000000000000000, 34.05468749999999289, 13.57481594606304576 ) ) ;
#12035 = ORIENTED_EDGE ( 'NONE', *, *, #18883, .F. ) ;
#12036 = CARTESIAN_POINT ( 'NONE',  ( 78.57481594606305464, 36.58476562499999574, 5.622872871577868636 ) ) ;
#12037 = CARTESIAN_POINT ( 'NONE',  ( 13.14518615778179544, 32.41757812608393863, -1.609821015232357215E-15 ) ) ;
#12038 = CARTESIAN_POINT ( 'NONE',  ( -5.622872871577873077, 33.80664062716786589, -13.57481594606304753 ) ) ;
#12039 = CARTESIAN_POINT ( 'NONE',  ( 103.5355339059327093, 3.535533905932755072, 3.750000002731185056 ) ) ;
#12040 = CARTESIAN_POINT ( 'NONE',  ( 130.0000000000000000, 40.15664062608393436, 13.14518615778179544 ) ) ;
#12041 = CARTESIAN_POINT ( 'NONE',  ( 55.70494972787295751, 40.45429687608393721, -9.295050272127046043 ) ) ;
#12042 = CARTESIAN_POINT ( 'NONE',  ( 53.73518119781812175, 35.99999999999999289, 6.828991891054477570 ) ) ;
#12043 = CARTESIAN_POINT ( 'NONE',  ( -8.049105076161786076E-16, 37.18007812608393436, -13.14518615778179544 ) ) ;
#12044 = CARTESIAN_POINT ( 'NONE',  ( -13.14518615778179544, 32.02070312608393010, 0.000000000000000000 ) ) ;
#12045 = CARTESIAN_POINT ( 'NONE',  ( 184.2131532318158804, 36.00000000000001421, 7.561388982944599491 ) ) ;
#12046 = CARTESIAN_POINT ( 'NONE',  ( 106.5389055433250860, 114.7507929638356785, -50.67499999726882010 ) ) ;
#12047 = VERTEX_POINT ( 'NONE', #6318 ) ;
#12048 = CARTESIAN_POINT ( 'NONE',  ( -9.598844408820458085, 33.75703124999999005, -9.598844408820458085 ) ) ;
#12049 = DIRECTION ( 'NONE',  ( 0.000000000000000000, 0.000000000000000000, 1.000000000000000000 ) ) ;
#12050 = CARTESIAN_POINT ( 'NONE',  ( 142.6678442549459191, 36.00000000000000711, 4.396229039743236200 ) ) ;
#12051 = CARTESIAN_POINT ( 'NONE',  ( 102.4999999999999716, 123.0500000000000114, -1.035533905932742638 ) ) ;
#12052 = CARTESIAN_POINT ( 'NONE',  ( 99.99999999999998579, 123.7500000010924737, -2.066987299999998751 ) ) ;
#12053 = CARTESIAN_POINT ( 'NONE',  ( 125.0271122604905116, 36.00000000000001421, -12.48139679469847252 ) ) ;
#12054 = CARTESIAN_POINT ( 'NONE',  ( 120.4011555911795455, 40.20625000216787726, -9.598844408820458085 ) ) ;
#12055 = CARTESIAN_POINT ( 'NONE',  ( 99.99999999999995737, 4.458734125000016313, 13.18750000136559208 ) ) ;
#12056 = CARTESIAN_POINT ( 'NONE',  ( 5.622872871577878406, 33.31054687499999289, 13.57481594606304576 ) ) ;
#12057 = VECTOR ( 'NONE', #4468, 1000.000000000000000 ) ;
#12058 = ORIENTED_EDGE ( 'NONE', *, *, #10172, .F. ) ;
#12059 = CARTESIAN_POINT ( 'NONE',  ( -13.09590655363597733, 36.00000000000000000, 1.137167824541468031 ) ) ;
#12060 = CARTESIAN_POINT ( 'NONE',  ( 5.622872871577878406, 40.45429687500001137, 13.57481594606304576 ) ) ;
#12061 = CARTESIAN_POINT ( 'NONE',  ( -8.049105076161786076E-16, 32.41757812608393863, -13.14518615778179544 ) ) ;
#12062 = CARTESIAN_POINT ( 'NONE',  ( 185.4011555911795313, 32.16953124999999147, -9.598844408820458085 ) ) ;
#12063 = CARTESIAN_POINT ( 'NONE',  ( 13.57481594606304576, 34.35234375216787583, -1.662435489736055892E-15 ) ) ;
#12064 = CARTESIAN_POINT ( 'NONE',  ( 65.00000000000000000, 39.31328125216787583, -13.57481594606304576 ) ) ;
#12065 = CARTESIAN_POINT ( 'NONE',  ( 103.1528011352953342, 82.81250000136560629, 3.152801135295355106 ) ) ;
#12066 = CARTESIAN_POINT ( 'NONE',  ( 55.70494972787295751, 32.51679687608393721, -9.295050272127046043 ) ) ;
#12067 = ADVANCED_FACE ( 'NONE', ( #6184 ), #1919, .F. ) ;
#12068 = CARTESIAN_POINT ( 'NONE',  ( 108.0825317500000011, 107.3738262389971538, -48.47500000273118559 ) ) ;
#12069 = CARTESIAN_POINT ( 'NONE',  ( 13.57481594606304576, 35.14609375216787157, -1.662435489736055892E-15 ) ) ;
#12070 = CARTESIAN_POINT ( 'NONE',  ( 102.0669872999999939, 123.4000000010924936, -0.8561741729129507261 ) ) ;
#12071 = CARTESIAN_POINT ( 'NONE',  ( -13.57481594606304576, 32.26874999999999716, 0.000000000000000000 ) ) ;
#12072 = CARTESIAN_POINT ( 'NONE',  ( 93.46109445667489979, 114.7507929638356785, -54.07499999726881867 ) ) ;
#12073 = CARTESIAN_POINT ( 'NONE',  ( 139.2950502721270425, 35.69179687608394147, -9.295050272127046043 ) ) ;
#12074 = ORIENTED_EDGE ( 'NONE', *, *, #10194, .F. ) ;
#12075 = CARTESIAN_POINT ( 'NONE',  ( 65.00000000000000000, 39.21406249999999716, -13.57481594606304576 ) ) ;
#12076 = AXIS2_PLACEMENT_3D ( 'NONE', #6436, #12827, #11114 ) ;
#12077 = FACE_OUTER_BOUND ( 'NONE', #2991, .T. ) ;
#12078 = CARTESIAN_POINT ( 'NONE',  ( 95.54126587499996504, 84.43750000136560629, -1.387778780781445676E-14 ) ) ;
#12079 = CARTESIAN_POINT ( 'NONE',  ( 116.8548138422182063, 38.91640625108393436, -5.444914386472297529 ) ) ;
#12080 = CARTESIAN_POINT ( 'NONE',  ( 116.4251840539369596, 38.56914062499999574, -5.622872871577872189 ) ) ;
#12081 = CARTESIAN_POINT ( 'NONE',  ( 106.5389055433250860, 114.7507929638356785, -48.42499999726882010 ) ) ;
#12082 = CARTESIAN_POINT ( 'NONE',  ( -13.57481594606304753, 38.66835937716786731, -5.622872871577873077 ) ) ;
#12083 = AXIS2_PLACEMENT_3D ( 'NONE', #11225, #15215, #4697 ) ;
#12084 = VERTEX_POINT ( 'NONE', #17568 ) ;
#12085 = CARTESIAN_POINT ( 'NONE',  ( 97.92893218813451028, -4.999999999999989342, 9.187500000000000000 ) ) ;
#12086 = ORIENTED_EDGE ( 'NONE', *, *, #23440, .F. ) ;
#12087 = CARTESIAN_POINT ( 'NONE',  ( -5.444914386472299306, 32.96328125108393436, 13.14518615778179722 ) ) ;
#12088 = CARTESIAN_POINT ( 'NONE',  ( 204.2950502721270425, 40.25585937608393294, -9.295050272127046043 ) ) ;
#12089 = CARTESIAN_POINT ( 'NONE',  ( 94.99999999999995737, -2.071067811865466624, 12.18750000273118950 ) ) ;
#12090 = CARTESIAN_POINT ( 'NONE',  ( 116.8548138422182205, 39.71015625108393010, -5.444914386472297529 ) ) ;
#12091 = CARTESIAN_POINT ( 'NONE',  ( 2.493653234604083739E-15, 35.74140625216787015, 13.57481594606304576 ) ) ;
#12092 = DIRECTION ( 'NONE',  ( -0.000000000000000000, 1.000000000000000000, -0.000000000000000000 ) ) ;
#12093 = CARTESIAN_POINT ( 'NONE',  ( 101.8468681455907330, 92.12499999863440792, 4.458734124999980786 ) ) ;
#12094 = CARTESIAN_POINT ( 'NONE',  ( 98.53841926354351699, 124.0500000010924708, 1.461580736456455920 ) ) ;
#12095 = EDGE_CURVE ( 'NONE', #19811, #747, #2052, .T. ) ;
#12096 = CARTESIAN_POINT ( 'NONE',  ( 181.8548138422181921, 31.97109375108393436, -5.444914386472297529 ) ) ;
#12097 = CARTESIAN_POINT ( 'NONE',  ( 122.2214956318786392, 36.00000000000002132, 10.60546543669468278 ) ) ;
#12098 = CARTESIAN_POINT ( 'NONE',  ( 99.99999999999995737, -4.458734124999988779, 8.937500001365592084 ) ) ;
#12099 = FACE_OUTER_BOUND ( 'NONE', #9456, .T. ) ;
#12100 = CARTESIAN_POINT ( 'NONE',  ( 103.1528011352953342, -3.152801135295355106, 10.81250000136559208 ) ) ;
#12101 = CARTESIAN_POINT ( 'NONE',  ( 105.6631189606246295, 114.1144967660473242, -51.30000000546237970 ) ) ;
#12102 = CARTESIAN_POINT ( 'NONE',  ( 103.1528011352953484, 95.43749999863440792, 3.152801135295352886 ) ) ;
#12103 = AXIS2_PLACEMENT_3D ( 'NONE', #12997, #19584, #15144 ) ;
#12104 = CARTESIAN_POINT ( 'NONE',  ( 102.0710678118654329, -4.999999999999989342, 9.312500000000000000 ) ) ;
#12105 = DIRECTION ( 'NONE',  ( 1.156482317317871478E-16, 0.000000000000000000, 1.000000000000000000 ) ) ;
#12106 = CARTESIAN_POINT ( 'NONE',  ( 9.295050272127046043, 34.10429687608393579, -9.295050272127046043 ) ) ;
#12107 = EDGE_CURVE ( 'NONE', #10223, #13527, #12901, .T. ) ;
#12108 = EDGE_LOOP ( 'NONE', ( #6597, #22609, #24010, #27440 ) ) ;
#12109 = CARTESIAN_POINT ( 'NONE',  ( 101.8468681455906903, 81.37500000136563472, -4.458734125000016313 ) ) ;
#12110 = CARTESIAN_POINT ( 'NONE',  ( -13.57481594606304398, 37.87460937499999147, 5.622872871577880183 ) ) ;
#12111 = ADVANCED_FACE ( 'NONE', ( #14994 ), #21724, .T. ) ;
#12112 = CARTESIAN_POINT ( 'NONE',  ( 195.0000000000000000, 33.60820312608392868, 13.14518615778179544 ) ) ;
#12113 =( BOUNDED_CURVE ( )  B_SPLINE_CURVE ( 2, ( #21402, #21534, #23673, #17243, #10543, #26230, #3867, #8838, #2299, #19669, #17098, #4151, #10679, #16962, #19110, #13084, #10815, #19250, #17528, #8409, #6420, #23394, #12811, #23950, #6278, #23808, #6144, #12529, #25801, #25661, #27818, #8554, #15089, #21823, #12943, #21678, #2153, #19530, #23534, #8696, #14809, #26085, #12, #6552, #4432, #6834, #16198, #25043, #3243, #20494, #7358, #13228, #9784, #2439, #3103, #3374, #18493, #14054, #5526, #20633, #26913, #9644, #13373, #19812, #13906, #15524, #24761, #21960, #16051, #18631, #11100, #24232, #14193, #15377, #17669, #1116, #9915, #977, #22912, #22634, #11625, #11769, #12044, #20769, #20349, #27053, #4713, #18348, #7504 ),
 .UNSPECIFIED., .F., .T. ) 
 B_SPLINE_CURVE_WITH_KNOTS ( ( 3, 2, 2, 2, 2, 2, 2, 2, 2, 2, 2, 2, 2, 2, 2, 2, 2, 2, 2, 2, 2, 2, 2, 2, 2, 2, 2, 2, 2, 2, 2, 2, 2, 2, 2, 2, 2, 2, 2, 2, 2, 2, 2, 2, 3 ),
 ( 0.4988304892921909817, 0.5000000000000000000, 0.5104166666666666297, 0.5208333333333333703, 0.5312500000000000000, 0.5416666666666666297, 0.5520833333333333703, 0.5625000000000000000, 0.5729166666666666297, 0.5833333333333333703, 0.5937500000000000000, 0.6041666666666666297, 0.6145833333333333703, 0.6250000000000000000, 0.6354166666666666297, 0.6458333333333333703, 0.6562500000000000000, 0.6666666666666666297, 0.6770833333333333703, 0.6875000000000000000, 0.6979166666666666297, 0.7083333333333333703, 0.7187500000000000000, 0.7291666666666666297, 0.7395833333333333703, 0.7500000000000000000, 0.7604166666666666297, 0.7708333333333333703, 0.7812500000000000000, 0.7916666666666666297, 0.8020833333333333703, 0.8125000000000000000, 0.8229166666666666297, 0.8333333333333333703, 0.8437500000000000000, 0.8541666666666666297, 0.8645833333333334814, 0.8750000000000000000, 0.8854166666666666297, 0.8958333333333333703, 0.9062500000000000000, 0.9166666666666666297, 0.9270833333333333703, 0.9375000000000000000, 0.9448587001587775980 ),
 .UNSPECIFIED. ) 
 CURVE ( )  GEOMETRIC_REPRESENTATION_ITEM ( )  RATIONAL_B_SPLINE_CURVE ( ( 0.9848264816800353927, 0.9914537246260980430, 1.000000000000000000, 0.9238795325112867385, 1.000000000000000000, 0.9238795325112867385, 1.000000000000000000, 0.9238795325112867385, 1.000000000000000000, 0.9238795325112867385, 1.000000000000000000, 0.9238795325112867385, 1.000000000000000000, 0.9238795325112867385, 1.000000000000000000, 0.9238795325112867385, 1.000000000000000000, 0.9238795325112867385, 1.000000000000000000, 0.9238795325112867385, 1.000000000000000000, 0.9238795325112867385, 1.000000000000000000, 0.9238795325112867385, 1.000000000000000000, 0.9238795325112867385, 1.000000000000000000, 0.9238795325112867385, 1.000000000000000000, 0.9238795325112867385, 1.000000000000000000, 0.9238795325112867385, 1.000000000000000000, 0.9238795325112867385, 1.000000000000000000, 0.9238795325112867385, 1.000000000000000000, 0.9238795325112867385, 1.000000000000000000, 0.9238795325112867385, 1.000000000000000000, 0.9238795325112867385, 1.000000000000000000, 0.9238795325112867385, 1.000000000000000000, 0.9238795325112867385, 1.000000000000000000, 0.9238795325112867385, 1.000000000000000000, 0.9238795325112867385, 1.000000000000000000, 0.9238795325112867385, 1.000000000000000000, 0.9238795325112867385, 1.000000000000000000, 0.9238795325112867385, 1.000000000000000000, 0.9238795325112867385, 1.000000000000000000, 0.9238795325112867385, 1.000000000000000000, 0.9238795325112867385, 1.000000000000000000, 0.9238795325112867385, 1.000000000000000000, 0.9238795325112867385, 1.000000000000000000, 0.9238795325112867385, 1.000000000000000000, 0.9238795325112867385, 1.000000000000000000, 0.9238795325112867385, 1.000000000000000000, 0.9238795325112867385, 1.000000000000000000, 0.9238795325112867385, 1.000000000000000000, 0.9238795325112867385, 1.000000000000000000, 0.9238795325112867385, 1.000000000000000000, 0.9238795325112867385, 1.000000000000000000, 0.9238795325112867385, 1.000000000000000000, 0.9238795325112867385, 1.000000000000000000, 0.9462258211652395667, 0.9684275895297407288 ) ) 
 REPRESENTATION_ITEM ( '' )  );
#12114 = VERTEX_POINT ( 'NONE', #12849 ) ;
#12115 = CARTESIAN_POINT ( 'NONE',  ( 194.6713997234275269, 53.49358765998905341, -15.00000000000000000 ) ) ;
#12116 = CARTESIAN_POINT ( 'NONE',  ( 96.84719886470459471, -3.152801135295355994, 6.812500001365592084 ) ) ;
#12117 = VERTEX_POINT ( 'NONE', #14854 ) ;
#12118 = CARTESIAN_POINT ( 'NONE',  ( 102.4976396683250925, 117.6869444889999841, -47.97500000273119269 ) ) ;
#12119 = CARTESIAN_POINT ( 'NONE',  ( 13.14518615778179900, 34.65000000108393152, -5.444914386472297529 ) ) ;
#12120 = DIRECTION ( 'NONE',  ( 5.782411586589357392E-17, -0.000000000000000000, 1.000000000000000000 ) ) ;
#12121 = CARTESIAN_POINT ( 'NONE',  ( -5.444914386472297529, 40.40468750108393436, -13.14518615778179722 ) ) ;
#12122 = VECTOR ( 'NONE', #20888, 1000.000000000000000 ) ;
#12123 = CARTESIAN_POINT ( 'NONE',  ( -9.295050272127044266, 38.46992187608393721, 9.295050272127047819 ) ) ;
#12124 = CARTESIAN_POINT ( 'NONE',  ( -5.444914386472297529, 33.26093750108393721, -13.14518615778179900 ) ) ;
#12125 = CARTESIAN_POINT ( 'NONE',  ( 101.8468681455907330, 92.74999999863439371, -4.458734124999994997 ) ) ;
#12126 = CARTESIAN_POINT ( 'NONE',  ( 0.000000000000000000, 23.00000000000000000, 0.000000000000000000 ) ) ;
#12127 = DIRECTION ( 'NONE',  ( 5.782411586589358625E-17, -0.000000000000000000, 1.000000000000000000 ) ) ;
#12128 = CARTESIAN_POINT ( 'NONE',  ( -9.295050272127046043, 31.92148437608393508, -9.295050272127046043 ) ) ;
#12129 = CARTESIAN_POINT ( 'NONE',  ( 95.54126587499996504, -1.846868145590724986, 2.750000001365592528 ) ) ;
#12130 = VECTOR ( 'NONE', #11998, 1000.000000000000000 ) ;
#12131 = CARTESIAN_POINT ( 'NONE',  ( 96.84719886470459471, 81.56250000136559208, -3.152801135295383084 ) ) ;
#12132 = CARTESIAN_POINT ( 'NONE',  ( -9.295050272127044266, 35.09648437608392868, 9.295050272127047819 ) ) ;
#12133 = CARTESIAN_POINT ( 'NONE',  ( -8.312177448680279460E-16, 38.51953125216787299, -13.57481594606304576 ) ) ;
#12134 = EDGE_CURVE ( 'NONE', #22508, #8637, #23674, .T. ) ;
#12135 = CARTESIAN_POINT ( 'NONE',  ( 189.3771271284220177, 38.46992187499999005, -13.57481594606295339 ) ) ;
#12136 = VERTEX_POINT ( 'NONE', #19710 ) ;
#12137 = CARTESIAN_POINT ( 'NONE',  ( -5.444914386472299306, 33.75703125108393721, 13.14518615778179722 ) ) ;
#12138 = CARTESIAN_POINT ( 'NONE',  ( 102.0669872999999797, 124.1500000010924794, -9.794112055954760458E-15 ) ) ;
#12139 = CARTESIAN_POINT ( 'NONE',  ( 99.99999999999998579, 93.81249999863440792, -4.458734124999994997 ) ) ;
#12140 = FACE_OUTER_BOUND ( 'NONE', #8881, .T. ) ;
#12141 = DIRECTION ( 'NONE',  ( -0.000000000000000000, -1.000000000000000000, -0.000000000000000000 ) ) ;
#12142 = CARTESIAN_POINT ( 'NONE',  ( 96.46446609406721961, -3.535533905932727539, 6.250000002731185056 ) ) ;
#12143 = CARTESIAN_POINT ( 'NONE',  ( 13.14518615778179900, 32.16953125108393152, 5.444914386472293977 ) ) ;
#12144 = EDGE_LOOP ( 'NONE', ( #20535, #25849, #4452, #26601 ) ) ;
#12145 = CARTESIAN_POINT ( 'NONE',  ( 55.70494972787295751, 36.88242187608393152, 9.295050272127047819 ) ) ;
#12146 = DIRECTION ( 'NONE',  ( 0.000000000000000000, 0.000000000000000000, -1.000000000000000000 ) ) ;
#12147 = CARTESIAN_POINT ( 'NONE',  ( 204.2950502721270425, 32.31835937608393294, 9.295050272127046043 ) ) ;
#12148 = B_SPLINE_CURVE_WITH_KNOTS ( 'NONE', 3,
 ( #23770, #11059, #12906, #400, #19631, #13336, #19770, #253, #10922, #8937, #4818, #19916, #22063, #17627, #22201, #17204, #13478, #6794, #8658, #23909, #15481, #17349, #4674, #21639, #2540, #10644, #26045, #13046, #19350, #28052, #21781 ),
 .UNSPECIFIED., .F., .F.,
 ( 4, 2, 2, 2, 2, 2, 2, 2, 2, 2, 1, 2, 2, 2, 2, 4 ),
 ( 1.033534235789917861E-15, 0.001647793485001597738, 0.003295586970002162015, 0.004943380455002727158, 0.005767277197503011682, 0.006591173940003295338, 0.008238967425003861783, 0.009886760910004429095, 0.01318234788000556545, 0.01483014136500612756, 0.01647793485000669314, 0.01812572833500725872, 0.01977352182000782083, 0.02306910879000895198, 0.02471690227500952103, 0.02636469576001009008 ),
 .UNSPECIFIED. ) ;
#12149 = ORIENTED_EDGE ( 'NONE', *, *, #5102, .T. ) ;
#12150 = CARTESIAN_POINT ( 'NONE',  ( 104.3262379212492590, 115.9545556584642867, -54.70000000000000995 ) ) ;
#12151 = CARTESIAN_POINT ( 'NONE',  ( -5.323790963956732902, 54.47170356488336296, -15.00000000000000000 ) ) ;
#12152 = CARTESIAN_POINT ( 'NONE',  ( 185.8198241863519797, 55.00000000000000000, 14.99999999999995204 ) ) ;
#12153 = CARTESIAN_POINT ( 'NONE',  ( 139.5988444088204687, 38.22187500216787015, 9.598844408820456309 ) ) ;
#12154 = CARTESIAN_POINT ( 'NONE',  ( 95.67376207875072680, 115.9545556584642867, -44.80000000546236549 ) ) ;
#12155 = CARTESIAN_POINT ( 'NONE',  ( 185.8198241863519797, 55.00000000000000000, 14.99999999999995204 ) ) ;
#12156 = CARTESIAN_POINT ( 'NONE',  ( 181.8548138422182205, 36.78320312608393294, 0.000000000000000000 ) ) ;
#12157 = VERTEX_POINT ( 'NONE', #27994 ) ;
#12158 =( BOUNDED_CURVE ( )  B_SPLINE_CURVE ( 2, ( #17479, #26179, #6645, #24469, #15623, #9075, #13615, #26760, #965 ),
 .UNSPECIFIED., .F., .F. ) 
 B_SPLINE_CURVE_WITH_KNOTS ( ( 3, 2, 2, 2, 3 ),
 ( 0.4642857142857142461, 0.4732142857142856429, 0.4821428571428570953, 0.4910714285714284366, 0.4999999999999998890 ),
 .UNSPECIFIED. ) 
 CURVE ( )  GEOMETRIC_REPRESENTATION_ITEM ( )  RATIONAL_B_SPLINE_CURVE ( ( 1.000000000000000444, 0.9238795325112862944, 1.000000000000000000, 0.9238795325112867385, 1.000000000000000000, 0.9238795325112867385, 1.000000000000000000, 0.9238795325112877377, 0.9999999999999990008 ) ) 
 REPRESENTATION_ITEM ( '' )  );
#12159 = ORIENTED_EDGE ( 'NONE', *, *, #1638, .F. ) ;
#12160 = CARTESIAN_POINT ( 'NONE',  ( 95.54126587499996504, 1.387778780781445676E-14, 0.4375000013655920839 ) ) ;
#12161 = CARTESIAN_POINT ( 'NONE',  ( -12.56650672479864461, 36.00000000000000000, -4.295155080288879823 ) ) ;
#12162 = CARTESIAN_POINT ( 'NONE',  ( 95.00000000000000000, 92.37499999726880162, -7.551217303480904118E-15 ) ) ;
#12163 = CARTESIAN_POINT ( 'NONE',  ( 1.662435489736055498E-15, -7.395377635281828788, -13.57481594606304398 ) ) ;
#12164 = FACE_OUTER_BOUND ( 'NONE', #25421, .T. ) ;
#12165 = CARTESIAN_POINT ( 'NONE',  ( -8.049105076161786076E-16, 39.75976562608394005, -13.14518615778179544 ) ) ;
#12166 = CARTESIAN_POINT ( 'NONE',  ( 13.57481594606304576, 40.60312499999999858, -1.662435489736055892E-15 ) ) ;
#12167 = CARTESIAN_POINT ( 'NONE',  ( 97.92893218813451028, -4.999999999999989342, 6.187499999999998224 ) ) ;
#12168 = CARTESIAN_POINT ( 'NONE',  ( 94.99999999999995737, 83.00000000000000000, -1.387778780781445676E-14 ) ) ;
#12169 = CARTESIAN_POINT ( 'NONE',  ( 139.5988444088204687, 35.74140624999999716, 9.598844408820456309 ) ) ;
#12170 = ORIENTED_EDGE ( 'NONE', *, *, #24323, .T. ) ;
#12171 = ORIENTED_EDGE ( 'NONE', *, *, #4782, .F. ) ;
#12172 = CARTESIAN_POINT ( 'NONE',  ( 65.00000000000000000, 36.83281249999999574, -13.57481594606304576 ) ) ;
#12173 = CARTESIAN_POINT ( 'NONE',  ( -8.312177448680279460E-16, 40.80156249999999574, -13.57481594606304576 ) ) ;
#12174 = CARTESIAN_POINT ( 'NONE',  ( -13.14518615778179189, 39.01562500108393294, 5.444914386472304635 ) ) ;
#12175 = CARTESIAN_POINT ( 'NONE',  ( 103.5355339059327093, -3.535533905932726206, 4.500000002731185944 ) ) ;
#12176 = CARTESIAN_POINT ( 'NONE',  ( 139.2950502721270425, 38.07304687608393579, -9.295050272127046043 ) ) ;
#12177 = CARTESIAN_POINT ( 'NONE',  ( 78.14518615778179367, 37.72578125108393721, 5.444914386472293977 ) ) ;
#12178 = ORIENTED_EDGE ( 'NONE', *, *, #26923, .F. ) ;
#12179 = ADVANCED_FACE ( 'NONE', ( #19431 ), #21577, .T. ) ;
#12180 = FACE_OUTER_BOUND ( 'NONE', #27704, .T. ) ;
#12181 = CARTESIAN_POINT ( 'NONE',  ( -5.444914386472299306, 39.11484375108394573, 13.14518615778179722 ) ) ;
#12182 = CARTESIAN_POINT ( 'NONE',  ( 102.4999999999999858, 123.9000000021849530, -9.847140817659276890E-15 ) ) ;
#12183 = CARTESIAN_POINT ( 'NONE',  ( 181.9040934463640156, 36.00000000000000000, 1.137167824541468031 ) ) ;
#12184 = CARTESIAN_POINT ( 'NONE',  ( 91.91746824999997045, 107.3738262389971680, -51.77499999726882152 ) ) ;
#12185 = CARTESIAN_POINT ( 'NONE',  ( 195.0000000000000000, 31.62382812608393579, -13.14518615778179544 ) ) ;
#12186 = CARTESIAN_POINT ( 'NONE',  ( 140.5630829503604673, 36.00000000000000711, 8.196709705857037065 ) ) ;
#12187 = CARTESIAN_POINT ( 'NONE',  ( 102.4999999999999858, 123.0069999999781487, -9.847140817659276890E-15 ) ) ;
#12188 = VECTOR ( 'NONE', #2277, 1000.000000000000000 ) ;
#12189 = CARTESIAN_POINT ( 'NONE',  ( 97.93301269999999192, 124.0000000010924879, 0.8561741729129329626 ) ) ;
#12190 = CARTESIAN_POINT ( 'NONE',  ( 119.4540428948962330, 35.99999999999999289, -8.172591786207229703 ) ) ;
#12191 = DIRECTION ( 'NONE',  ( -0.000000000000000000, -1.000000000000000000, -0.000000000000000000 ) ) ;
#12192 = CARTESIAN_POINT ( 'NONE',  ( 103.1528011352953342, 3.152801135295383084, 12.06250000136559208 ) ) ;
#12193 = CARTESIAN_POINT ( 'NONE',  ( -5.622872871577873077, 32.41757812499999858, 13.57481594606304753 ) ) ;
#12194 = VERTEX_POINT ( 'NONE', #12983 ) ;
#12195 = CARTESIAN_POINT ( 'NONE',  ( -11.93524237669063126, 36.00000000000001421, -5.809862729998008568 ) ) ;
#12196 =( BOUNDED_CURVE ( )  B_SPLINE_CURVE ( 2, ( #9745, #14154, #16303, #12010, #3061, #20593, #22448, #24435, #1219 ),
 .UNSPECIFIED., .F., .F. ) 
 B_SPLINE_CURVE_WITH_KNOTS ( ( 3, 2, 2, 2, 3 ),
 ( 0.9642857142857141906, 0.9732142857142855874, 0.9821428571428569843, 0.9910714285714286031, 1.000000000000000000 ),
 .UNSPECIFIED. ) 
 CURVE ( )  GEOMETRIC_REPRESENTATION_ITEM ( )  RATIONAL_B_SPLINE_CURVE ( ( 1.000000000000000888, 0.9238795325112857393, 1.000000000000000000, 0.9238795325112867385, 1.000000000000000000, 0.9238795325112867385, 1.000000000000000000, 0.9238795325112867385, 1.000000000000000000 ) ) 
 REPRESENTATION_ITEM ( '' )  );
#12197 = CARTESIAN_POINT ( 'NONE',  ( -9.598844408820458085, 39.31328124999999574, -9.598844408820458085 ) ) ;
#12198 = CARTESIAN_POINT ( 'NONE',  ( 3.755638265659908104, 31.58960998161716560, -13.14518615778179722 ) ) ;
#12199 = CARTESIAN_POINT ( 'NONE',  ( 9.598844408820456309, 34.45156250216787441, -9.598844408820458085 ) ) ;
#12200 = CARTESIAN_POINT ( 'NONE',  ( 104.9999999999999716, 2.071067811865491937, 2.687500002731185944 ) ) ;
#12201 = CARTESIAN_POINT ( 'NONE',  ( 95.54126587499995082, 83.75000000136560629, 1.846868145590724986 ) ) ;
#12202 = CARTESIAN_POINT ( 'NONE',  ( 65.00000000000000000, 39.36289062608393152, 13.14518615778179544 ) ) ;
#12203 = CARTESIAN_POINT ( 'NONE',  ( 93.46109445667491400, 105.2492070361643215, -49.17500000273119554 ) ) ;
#12204 = CARTESIAN_POINT ( 'NONE',  ( 9.598844408820459861, 35.04687500216787299, 9.598844408820456309 ) ) ;
#12205 = CARTESIAN_POINT ( 'NONE',  ( 99.14382582708707048, 123.0000000010925021, -2.066987299999999195 ) ) ;
#12206 = CARTESIAN_POINT ( 'NONE',  ( -13.57481594606304753, 40.95039062499999005, -5.622872871577872189 ) ) ;
#12207 = CARTESIAN_POINT ( 'NONE',  ( 104.3262379212492448, 115.9545556584642867, -53.19999999453762740 ) ) ;
#12208 = CARTESIAN_POINT ( 'NONE',  ( 116.8548138422182205, 34.40195312608393152, 0.000000000000000000 ) ) ;
#12209 = ORIENTED_EDGE ( 'NONE', *, *, #14702, .T. ) ;
#12210 = CARTESIAN_POINT ( 'NONE',  ( 143.5748159460630688, 37.47773437716787015, 5.622872871577868636 ) ) ;
#12211 = CARTESIAN_POINT ( 'NONE',  ( 9.295050272127047819, 40.25585937608393294, 9.295050272127046043 ) ) ;
#12212 = CARTESIAN_POINT ( 'NONE',  ( -9.598844408820458085, 39.41250000216787441, -9.598844408820458085 ) ) ;
#12213 = CARTESIAN_POINT ( 'NONE',  ( 143.1451861577818079, 38.51953125108393294, 5.444914386472293977 ) ) ;
#12214 = CARTESIAN_POINT ( 'NONE',  ( 78.57481594606304043, 39.85898437716787157, 5.622872871577869525 ) ) ;
#12215 = AXIS2_PLACEMENT_3D ( 'NONE', #3175, #24973, #1192 ) ;
#12216 = CARTESIAN_POINT ( 'NONE',  ( 93.46109445667489979, 105.2492070361643215, -55.42499999726882720 ) ) ;
#12217 = AXIS2_PLACEMENT_3D ( 'NONE', #26346, #23505, #28200 ) ;
#12218 = CARTESIAN_POINT ( 'NONE',  ( 5.622872871577878406, 39.75976562716787299, 13.57481594606304576 ) ) ;
#12219 = ORIENTED_EDGE ( 'NONE', *, *, #27950, .T. ) ;
#12220 = CARTESIAN_POINT ( 'NONE',  ( 94.99999999999995737, 1.387778780781445676E-14, 8.000000000000000000 ) ) ;
#12221 = ORIENTED_EDGE ( 'NONE', *, *, #6545, .F. ) ;
#12222 = CARTESIAN_POINT ( 'NONE',  ( 9.295050272127047819, 34.69960937608393436, 9.295050272127046043 ) ) ;
#12223 = CARTESIAN_POINT ( 'NONE',  ( 195.0000000000000000, 31.37578125216787583, -13.57481594606304576 ) ) ;
#12224 = CARTESIAN_POINT ( 'NONE',  ( 13.57481594606304576, 35.96878166419460143, -3.279908293447338696 ) ) ;
#12225 = CARTESIAN_POINT ( 'NONE',  ( 102.0710678118654329, 5.000000000000018652, 12.81250000273118950 ) ) ;
#12226 = CARTESIAN_POINT ( 'NONE',  ( 124.5550856135277087, 37.52734375108393294, 13.14518615778179722 ) ) ;
#12227 = CARTESIAN_POINT ( 'NONE',  ( 98.96446609406724804, 123.6500000021849672, 2.499999999999969802 ) ) ;
#12228 = CARTESIAN_POINT ( 'NONE',  ( 130.0000000000000000, -7.395377635281828788, -13.57481594606305997 ) ) ;
#12229 = CARTESIAN_POINT ( 'NONE',  ( 95.54126587499999346, 92.87499999863439371, 1.846868145590722543 ) ) ;
#12230 = CARTESIAN_POINT ( 'NONE',  ( 100.8561741729129153, 122.9000000010924936, -2.066987299999999195 ) ) ;
#12231 = CARTESIAN_POINT ( 'NONE',  ( 208.5748159460630688, 37.42812499999999432, -1.662435489736055892E-15 ) ) ;
#12232 = APPLICATION_PROTOCOL_DEFINITION ( 'draft international standard', 'automotive_design', 1998, #52 ) ;
#12233 = CARTESIAN_POINT ( 'NONE',  ( 130.2703369776646696, 35.99999999999998579, 13.14949859323919945 ) ) ;
#12234 = CARTESIAN_POINT ( 'NONE',  ( 98.15313185440925281, 4.458734125000016313, 1.500000001365592972 ) ) ;
#12235 = CARTESIAN_POINT ( 'NONE',  ( -8.312177448680279460E-16, 37.72578125216787726, -13.57481594606304576 ) ) ;
#12236 = CARTESIAN_POINT ( 'NONE',  ( 101.8468681455907046, 4.458734125000016313, 5.125000001365592972 ) ) ;
#12237 = CARTESIAN_POINT ( 'NONE',  ( 94.33688103937537051, 105.8855032339526758, -46.30000000546237970 ) ) ;
#12238 =( GEOMETRIC_REPRESENTATION_CONTEXT ( 3 ) GLOBAL_UNCERTAINTY_ASSIGNED_CONTEXT ( ( #14956 ) ) GLOBAL_UNIT_ASSIGNED_CONTEXT ( ( #13307, #228, #17752 ) ) REPRESENTATION_CONTEXT ( 'NONE', 'WORKASPACE' ) );
#12239 = CARTESIAN_POINT ( 'NONE',  ( 98.15313185440925281, 90.99999999863439371, 4.458734124999979898 ) ) ;
#12240 = CIRCLE ( 'NONE', #25911, 4.999999999999989342 ) ;
#12241 = DIRECTION ( 'NONE',  ( 0.000000000000000000, -0.000000000000000000, 1.000000000000000000 ) ) ;
#12242 = CARTESIAN_POINT ( 'NONE',  ( 9.598844408820456309, 40.70234374999999716, -9.598844408820458085 ) ) ;
#12243 = EDGE_LOOP ( 'NONE', ( #27189, #27506, #24159, #21542 ) ) ;
#12244 = CARTESIAN_POINT ( 'NONE',  ( 103.1528011352953342, 84.31250000136560629, -3.152801135295383084 ) ) ;
#12245 = ADVANCED_FACE ( 'NONE', ( #55 ), #19571, .T. ) ;
#12246 =( BOUNDED_CURVE ( )  B_SPLINE_CURVE ( 2, ( #21051, #27203, #28128, #3528, #9789, #7655, #7929, #14476, #7797 ),
 .UNSPECIFIED., .F., .F. ) 
 B_SPLINE_CURVE_WITH_KNOTS ( ( 3, 2, 2, 2, 3 ),
 ( 0.02083333333333358892, 0.03125000000000020123, 0.04166666666666681007, 0.05208333333333342585, 0.06250000000000004163 ),
 .UNSPECIFIED. ) 
 CURVE ( )  GEOMETRIC_REPRESENTATION_ITEM ( )  RATIONAL_B_SPLINE_CURVE ( ( 0.9999999999999981126, 0.9238795325112886259, 1.000000000000000000, 0.9238795325112867385, 1.000000000000000000, 0.9238795325112867385, 1.000000000000000000, 0.9238795325112864054, 1.000000000000000222 ) ) 
 REPRESENTATION_ITEM ( '' )  );
#12247 = CARTESIAN_POINT ( 'NONE',  ( 84.99999999999998579, 95.00000000000000000, 14.99999999999999467 ) ) ;
#12248 = VERTEX_POINT ( 'NONE', #194 ) ;
#12249 = ORIENTED_EDGE ( 'NONE', *, *, #2356, .T. ) ;
#12250 = EDGE_CURVE ( 'NONE', #24277, #8963, #8735, .T. ) ;
#12251 = CARTESIAN_POINT ( 'NONE',  ( 192.7238531554485803, 51.46995505939284499, -14.99999999999966072 ) ) ;
#12252 = CARTESIAN_POINT ( 'NONE',  ( 99.99999999999995737, 4.458734125000016313, 8.437500001365592084 ) ) ;
#12253 = EDGE_CURVE ( 'NONE', #4950, #11, #17428, .T. ) ;
#12254 = ORIENTED_EDGE ( 'NONE', *, *, #8613, .F. ) ;
#12255 = CARTESIAN_POINT ( 'NONE',  ( 91.91746824999999887, 110.0000000000000000, -47.37500000273119838 ) ) ;
#12256 = CARTESIAN_POINT ( 'NONE',  ( 2.414731522848535132E-15, 33.60820312608392868, 13.14518615778179544 ) ) ;
#12257 = CARTESIAN_POINT ( 'NONE',  ( 189.3771271284221314, 39.66054687716786731, 13.57481594606304753 ) ) ;
#12258 = CARTESIAN_POINT ( 'NONE',  ( 105.6631189606246153, 114.1144967660473242, -53.80000000000001137 ) ) ;
#12259 = VECTOR ( 'NONE', #20125, 1000.000000000000000 ) ;
#12260 = ADVANCED_FACE ( 'NONE', ( #8876 ), #14580, .T. ) ;
#12261 = CARTESIAN_POINT ( 'NONE',  ( 99.99999999999998579, 101.5015231886685712, -44.62500000273119838 ) ) ;
#12262 = CARTESIAN_POINT ( 'NONE',  ( 120.7049497278729575, 38.27148437608393294, -9.295050272127046043 ) ) ;
#12263 = CARTESIAN_POINT ( 'NONE',  ( -9.295050272127046043, 31.72304687608393081, -9.295050272127046043 ) ) ;
#12264 = CARTESIAN_POINT ( 'NONE',  ( 78.57481594606304043, 38.17226562499999432, 5.622872871577869525 ) ) ;
#12265 = DIRECTION ( 'NONE',  ( 0.000000000000000000, 0.000000000000000000, 1.000000000000000000 ) ) ;
#12266 = EDGE_CURVE ( 'NONE', #16468, #8963, #10009, .T. ) ;
#12267 = CARTESIAN_POINT ( 'NONE',  ( 99.99999999999997158, 102.6397644303321215, -50.50000000000000000 ) ) ;
#12268 = CARTESIAN_POINT ( 'NONE',  ( 5.444914386472297529, 33.36015625108393579, -13.14518615778179900 ) ) ;
#12269 = CARTESIAN_POINT ( 'NONE',  ( 98.15313185440923860, 4.458734125000016313, 3.500000001365592528 ) ) ;
#12270 = CARTESIAN_POINT ( 'NONE',  ( 99.99999999999995737, 81.43750000136559208, -4.458734125000016313 ) ) ;
#12271 = CARTESIAN_POINT ( 'NONE',  ( 9.295050272127046043, 37.08085937608393579, -9.295050272127046043 ) ) ;
#12272 = CARTESIAN_POINT ( 'NONE',  ( 6.944423797152706079, 31.55306878032414986, -11.16113333171310451 ) ) ;
#12273 = CARTESIAN_POINT ( 'NONE',  ( 72.61652532548083627, 54.91574374957784954, 14.99999999999997691 ) ) ;
#12274 = ORIENTED_EDGE ( 'NONE', *, *, #19255, .F. ) ;
#12275 = CARTESIAN_POINT ( 'NONE',  ( -5.444914386472297529, 31.87187500108393223, -13.14518615778179722 ) ) ;
#12276 =( BOUNDED_CURVE ( )  B_SPLINE_CURVE ( 2, ( #5065, #26588, #15873, #13439, #26731, #9749, #22166, #15734, #24868, #6903, #9188, #11731, #1081, #20309, #5349, #13729, #2785, #2644, #9464, #18459, #3066, #18167, #24438, #11589, #26879, #4925, #16013, #15591, #7324, #11448, #22451, #4779, #7176 ),
 .UNSPECIFIED., .F., .T. ) 
 B_SPLINE_CURVE_WITH_KNOTS ( ( 3, 2, 2, 2, 2, 2, 2, 2, 2, 2, 2, 2, 2, 2, 2, 2, 3 ),
 ( 0.000000000000000000, 0.04166666666666666435, 0.08333333333333332871, 0.1250000000000000000, 0.1666666666666666574, 0.2083333333333333426, 0.2500000000000000000, 0.2916666666666666852, 0.3333333333333333148, 0.3750000000000000000, 0.4166666666666666852, 0.4583333333333333148, 0.5000000000000000000, 0.5416666666666666297, 0.5833333333333333703, 0.6250000000000000000, 0.6458333337712076627 ),
 .UNSPECIFIED. ) 
 CURVE ( )  GEOMETRIC_REPRESENTATION_ITEM ( )  RATIONAL_B_SPLINE_CURVE ( ( 1.000000000000000000, 0.9238795325112867385, 1.000000000000000000, 0.9238795325112867385, 1.000000000000000000, 0.9238795325112867385, 1.000000000000000000, 0.9238795325112867385, 1.000000000000000000, 0.9238795325112867385, 1.000000000000000000, 0.9238795325112867385, 1.000000000000000000, 0.9238795325112867385, 1.000000000000000000, 0.9238795325112867385, 1.000000000000000000, 0.9238795325112867385, 1.000000000000000000, 0.9238795325112867385, 1.000000000000000000, 0.9238795325112867385, 1.000000000000000000, 0.9238795325112867385, 1.000000000000000000, 0.9238795325112867385, 1.000000000000000000, 0.9238795325112867385, 1.000000000000000000, 0.9238795325112867385, 1.000000000000000000, 0.9619397654556945954, 0.9619397662556433692 ) ) 
 REPRESENTATION_ITEM ( '' )  );
#12277 = DIRECTION ( 'NONE',  ( 0.000000000000000000, -1.000000000000000000, 0.000000000000000000 ) ) ;
#12278 = CARTESIAN_POINT ( 'NONE',  ( 101.8468681455907330, 94.37499999863440792, 4.458734124999980786 ) ) ;
#12279 = DIRECTION ( 'NONE',  ( -5.782411586589357392E-17, 0.000000000000000000, -1.000000000000000000 ) ) ;
#12280 = CARTESIAN_POINT ( 'NONE',  ( -13.57481594606304398, 40.25585937499999289, 5.622872871577880183 ) ) ;
#12281 = EDGE_CURVE ( 'NONE', #20557, #23148, #1296, .T. ) ;
#12282 = AXIS2_PLACEMENT_3D ( 'NONE', #26066, #25644, #19513 ) ;
#12283 = DIRECTION ( 'NONE',  ( -0.000000000000000000, -0.000000000000000000, -1.000000000000000000 ) ) ;
#12284 = CARTESIAN_POINT ( 'NONE',  ( 9.295050272127046043, 32.31835937608393294, -9.295050272127046043 ) ) ;
#12285 = ORIENTED_EDGE ( 'NONE', *, *, #3429, .F. ) ;
#12286 = CARTESIAN_POINT ( 'NONE',  ( 74.29505027212704249, 38.66835937608393436, 9.295050272127046043 ) ) ;
#12287 = CARTESIAN_POINT ( 'NONE',  ( 102.0669872999999797, 122.7500000010924737, -9.794112055954760458E-15 ) ) ;
#12288 = CARTESIAN_POINT ( 'NONE',  ( 5.622872871577961895, 35.19570312499999432, -13.57481594606295339 ) ) ;
#12289 = VERTEX_POINT ( 'NONE', #7870 ) ;
#12290 = CARTESIAN_POINT ( 'NONE',  ( 96.46446609406726225, 92.37500000000000000, -3.535533905932738197 ) ) ;
#12291 = AXIS2_PLACEMENT_3D ( 'NONE', #9063, #26025, #25891 ) ;
#12292 = EDGE_CURVE ( 'NONE', #17147, #23013, #11852, .T. ) ;
#12293 = CARTESIAN_POINT ( 'NONE',  ( 0.000000000000000000, -7.395377635281828788, 13.57481594606304398 ) ) ;
#12294 = CARTESIAN_POINT ( 'NONE',  ( 51.90409344636400846, 36.00000000000000000, 1.137167824541468031 ) ) ;
#12295 = ADVANCED_FACE ( 'NONE', ( #1611 ), #18978, .F. ) ;
#12296 = CARTESIAN_POINT ( 'NONE',  ( 116.4251840539369596, 34.79882812716787299, 5.622872871577880183 ) ) ;
#12297 = CARTESIAN_POINT ( 'NONE',  ( 99.99999999999998579, 128.0000000000000000, -5.204170427930421283E-15 ) ) ;
#12298 = DIRECTION ( 'NONE',  ( 1.156482317317871478E-16, 0.000000000000000000, 1.000000000000000000 ) ) ;
#12299 = CARTESIAN_POINT ( 'NONE',  ( 189.5550856135277229, 36.63437500108393152, -13.14518615778179900 ) ) ;
#12300 = EDGE_LOOP ( 'NONE', ( #6188, #17978, #10811, #5051 ) ) ;
#12301 = AXIS2_PLACEMENT_3D ( 'NONE', #26821, #592, #26965 ) ;
#12302 = ORIENTED_EDGE ( 'NONE', *, *, #16630, .T. ) ;
#12303 = CARTESIAN_POINT ( 'NONE',  ( 95.54126587499996504, -1.846868145590724986, 13.75000000136559386 ) ) ;
#12304 = ADVANCED_FACE ( 'NONE', ( #10269 ), #3182, .F. ) ;
#12305 = CARTESIAN_POINT ( 'NONE',  ( -8.312177448680279460E-16, 33.75703125216787726, -13.57481594606304576 ) ) ;
#12306 = CARTESIAN_POINT ( 'NONE',  ( 104.4587341249999639, 83.93750000136560629, -1.442382525525748735E-14 ) ) ;
#12307 = CARTESIAN_POINT ( 'NONE',  ( 9.295050272127046043, 40.45429687608393721, -9.295050272127046043 ) ) ;
#12308 = CARTESIAN_POINT ( 'NONE',  ( 13.14518615778179544, 40.35507812608393863, -1.609821015232357215E-15 ) ) ;
#12309 = VECTOR ( 'NONE', #7764, 1000.000000000000000 ) ;
#12310 = CARTESIAN_POINT ( 'NONE',  ( 107.0000000000000000, 110.0000000000000000, -145.0000000000000284 ) ) ;
#12311 = CARTESIAN_POINT ( 'NONE',  ( 102.0710678118654329, -4.999999999999989342, 6.312499999999998224 ) ) ;
#12312 = FACE_OUTER_BOUND ( 'NONE', #24253, .T. ) ;
#12313 = CARTESIAN_POINT ( 'NONE',  ( 95.00472066334982912, 116.8754121666685393, -45.92499999726882720 ) ) ;
#12314 = ORIENTED_EDGE ( 'NONE', *, *, #24484, .T. ) ;
#12315 = CARTESIAN_POINT ( 'NONE',  ( 99.99999999999995737, 84.25000000000000000, 4.999999999999990230 ) ) ;
#12316 = UNCERTAINTY_MEASURE_WITH_UNIT (LENGTH_MEASURE( 1.000000000000000082E-05 ), #10162, 'distance_accuracy_value', 'NONE');
#12317 = CARTESIAN_POINT ( 'NONE',  ( -13.57481594606304753, 38.56914062500000284, -5.622872871577873077 ) ) ;
#12318 = CARTESIAN_POINT ( 'NONE',  ( 13.14518615778179900, 39.31328125108392868, 5.444914386472293977 ) ) ;
#12319 = CARTESIAN_POINT ( 'NONE',  ( 96.46446609406721961, 3.535533905932755072, 7.000000002731185056 ) ) ;
#12320 = CARTESIAN_POINT ( 'NONE',  ( 139.2950502721270425, 38.86679687608393863, -9.295050272127046043 ) ) ;
#12321 = CARTESIAN_POINT ( 'NONE',  ( 65.00000000000000000, 35.59257812608393579, -13.14518615778179544 ) ) ;
#12322 = VECTOR ( 'NONE', #5674, 1000.000000000000000 ) ;
#12323 = ADVANCED_FACE ( 'NONE', ( #1333 ), #27826, .T. ) ;
#12324 = CARTESIAN_POINT ( 'NONE',  ( -18.00000000000000355, 78.00000000000000000, 13.00000000000000178 ) ) ;
#12325 = CARTESIAN_POINT ( 'NONE',  ( 9.295050272127046043, 35.49335937608393010, -9.295050272127046043 ) ) ;
#12326 = CARTESIAN_POINT ( 'NONE',  ( 99.99999999999995737, -4.999999999999990230, 9.375000002731184168 ) ) ;
#12327 = CARTESIAN_POINT ( 'NONE',  ( 102.4999999999999716, 123.8500000021849416, 1.035533905932722876 ) ) ;
#12328 = CARTESIAN_POINT ( 'NONE',  ( 142.0772764098356333, 36.00000000000000000, -6.197985357349214297 ) ) ;
#12329 = EDGE_CURVE ( 'NONE', #18468, #12537, #27138, .T. ) ;
#12330 = CARTESIAN_POINT ( 'NONE',  ( 120.4011555911795455, 40.10703124999999147, -9.598844408820458085 ) ) ;
#12331 = ORIENTED_EDGE ( 'NONE', *, *, #16454, .T. ) ;
#12332 = DIRECTION ( 'NONE',  ( 1.000000000000000000, 0.000000000000000000, 0.000000000000000000 ) ) ;
#12333 = CARTESIAN_POINT ( 'NONE',  ( -9.295050272127046043, 37.27929687608393294, -9.295050272127046043 ) ) ;
#12334 = CARTESIAN_POINT ( 'NONE',  ( 136.8311344573049553, 36.00000000000000000, 11.35217666745991671 ) ) ;
#12335 = CARTESIAN_POINT ( 'NONE',  ( 98.96446609406727646, 124.8500000000000085, -2.499999999999997780 ) ) ;
#12336 = CARTESIAN_POINT ( 'NONE',  ( 100.8561741729129295, 123.4000000010924794, 2.066987299999979211 ) ) ;
#12337 = CARTESIAN_POINT ( 'NONE',  ( 134.1572863549629062, 35.99999999999997868, -12.92256159328817411 ) ) ;
#12338 = LINE ( 'NONE', #10195, #28190 ) ;
#12339 = CARTESIAN_POINT ( 'NONE',  ( 104.4587341249999639, 1.442382525525748735E-14, 11.93750000136559208 ) ) ;
#12340 = CARTESIAN_POINT ( 'NONE',  ( 99.99999999999998579, 123.3000000021849587, -2.499999999999997780 ) ) ;
#12341 = ORIENTED_EDGE ( 'NONE', *, *, #12292, .F. ) ;
#12342 = CARTESIAN_POINT ( 'NONE',  ( 98.96446609406727646, 124.1500000021849672, -2.499999999999997780 ) ) ;
#12343 = CARTESIAN_POINT ( 'NONE',  ( 13.57481594606304931, 39.75976562499999289, 5.622872871577869525 ) ) ;
#12344 = CARTESIAN_POINT ( 'NONE',  ( 9.295050272127046043, 33.90585937608393152, -9.295050272127046043 ) ) ;
#12345 = CARTESIAN_POINT ( 'NONE',  ( -5.622872871577873077, 33.01289062716787726, -13.57481594606304753 ) ) ;
#12346 = CARTESIAN_POINT ( 'NONE',  ( 102.0710678118654329, 5.000000000000018652, 2.687499999999999112 ) ) ;
#12347 = CARTESIAN_POINT ( 'NONE',  ( 98.15313185440925281, 84.50000000136562051, -4.458734125000016313 ) ) ;
#12348 = CARTESIAN_POINT ( 'NONE',  ( 78.14518615778179367, 38.81718750108393579, -5.444914386472297529 ) ) ;
#12349 = CARTESIAN_POINT ( 'NONE',  ( 106.5389055433251002, 114.7507929638356785, -50.17500000273119554 ) ) ;
#12350 = CARTESIAN_POINT ( 'NONE',  ( 9.598844408820456309, 35.24531250216787726, -9.598844408820458085 ) ) ;
#12351 = CARTESIAN_POINT ( 'NONE',  ( -8.312177448680279460E-16, 39.21406249999999716, -13.57481594606304576 ) ) ;
#12352 = CYLINDRICAL_SURFACE ( 'NONE', #11296, 2.499999999999995115 ) ;
#12353 = CARTESIAN_POINT ( 'NONE',  ( 93.00000000000000000, 112.2744378736303332, -54.59999999453764019 ) ) ;
#12354 = CARTESIAN_POINT ( 'NONE',  ( 120.4011555911795455, 40.90078124999999432, -9.598844408820458085 ) ) ;
#12355 = ORIENTED_EDGE ( 'NONE', *, *, #16469, .T. ) ;
#12356 = CARTESIAN_POINT ( 'NONE',  ( 97.83688103937537051, 103.3426043859339103, -52.09999999453764019 ) ) ;
#12357 = CARTESIAN_POINT ( 'NONE',  ( -5.444914386472297529, 39.80937500108392868, -13.14518615778179900 ) ) ;
#12358 = CARTESIAN_POINT ( 'NONE',  ( 96.84719886470459471, 80.31250000136559208, -3.152801135295383084 ) ) ;
#12359 = CARTESIAN_POINT ( 'NONE',  ( 120.7049497278729575, 38.86679687608393863, -9.295050272127046043 ) ) ;
#12360 = CARTESIAN_POINT ( 'NONE',  ( 65.00000000000000000, 38.51953125216787299, -13.57481594606304576 ) ) ;
#12361 = CARTESIAN_POINT ( 'NONE',  ( 95.00472066334982912, 116.8754121666685393, -51.92499999726881299 ) ) ;
#12362 = CARTESIAN_POINT ( 'NONE',  ( -9.598844408820458085, 34.65000000216787868, -9.598844408820458085 ) ) ;
#12363 = ORIENTED_EDGE ( 'NONE', *, *, #12606, .T. ) ;
#12364 = CARTESIAN_POINT ( 'NONE',  ( 96.46446609406721961, 3.535533905932755072, 10.87500000000000000 ) ) ;
#12365 = CARTESIAN_POINT ( 'NONE',  ( 94.33688103937537051, 114.1144967660473242, -52.20000000000000995 ) ) ;
#12366 = CARTESIAN_POINT ( 'NONE',  ( -5.444914386472297529, 33.45937500108394147, -13.14518615778179900 ) ) ;
#12367 = CARTESIAN_POINT ( 'NONE',  ( 185.7049497278729575, 36.68398437608392726, 9.295050272127047819 ) ) ;
#12368 =( BOUNDED_SURFACE ( )  B_SPLINE_SURFACE ( 1, 2, ( 
 ( #11166, #17454, #9192, #17597, #15451, #11309, #2369, #10891, #26303, #4501, #19883, #20031, #13443, #11027, #19738, #22170, #6766, #24164, #2647, #511, #18462, #25145, #14300, #13874, #18315, #799, #16448, #26882, #27305, #22742, #11877, #9891, #16315, #7762, #5068, #24586, #5635, #23018, #27024, #9752, #3489, #16164, #12153, #7469, #20879, #1365, #10026, #13732, #27169, #5210, #20459, #24871, #5354, #3208, #7328, #15876, #9612, #9468, #18735, #7623, #27433, #22455, #1084, #20600, #25015, #5493, #14162, #3348, #2922, #22881, #22600, #11592, #12018, #20312, #20741, #18170, #16016, #1226, #941, #18602, #24730, #3069, #11734, #14019, #1917, #12431, #27715, #7897, #6049, #12566, #21020, #8453, #25700, #23157, #14714, #14849, #10583, #14992, #23709, #19003, #16867, #18864, #21294, #12714, #19148, #25565, #27992, #27853, #8310, #17140, #17000, #12296, #23432, #10720, #8177, #16591, #21437, #4185, #23570, #3906, #4051, #21151, #1777, #3632, #6316, #14442, #19291, #10442, #10296, #25285, #25841, #6182, #12846, #1500, #21575, #27576, #8034, #2050, #19427, #5771, #3772, #25431, #10154, #5914, #16732, #14579, #1637, #23298, #28127, #26268, #4603, #12982, #477, #17713, #15126, #6730, #6874, #2614, #7009, #15705, #10992, #8872, #10854, #13262, #4749, #11132, #17564, #19998, #19847, #333, #9160, #9020, #4324, #15416, #2756, #19705, #8592, #13409, #24407, #15558, #190, #24267, #13124 ),
 ( #22136, #21859, #24131, #11277, #6588, #17282, #2334, #21719, #21995, #17852, #2471, #15270, #11419, #4467, #26415, #23988, #26555, #4894, #13558, #22281, #25984, #6454, #23847, #2193, #19566, #50, #8731, #17424, #26122, #3032, #5176, #18284, #11559, #20712, #619, #11701, #24977, #7435, #20275, #24838, #9723, #13840, #16130, #1051, #26990, #22565, #7585, #3178, #7295, #5460, #910, #14129, #5321, #13701, #20426, #18425, #24554, #9580, #13980, #15984, #22418, #5035, #16278, #2889, #22708, #11988, #762, #9293, #11848, #22850, #20570, #3317, #18135, #1194, #20139, #17990, #26700, #27133, #9435, #7149, #26848, #15844, #24698, #10966, #164, #4577, #25812, #2589, #6560, #19821, #26387, #28100, #17397, #10824, #13091, #8564, #22110, #27961, #26095, #8991, #2309, #17254, #19678, #21969, #22, #8846, #13237, #21832, #8704, #305, #6698, #4296, #6842, #15240, #15532, #17536, #2019, #23960, #2446, #12820, #4439, #26240, #12954, #21544, #4160, #17681, #10688, #15385, #13382, #19395, #8418, #24099, #24240, #11107, #4722, #15097, #19261, #17107, #6286, #14963, #23818, #23683, #25955, #6428, #21687, #2162, #19540, #4868, #24671, #26963, #3002, #22252, #20397, #2729, #6984, #5010, #22823, #19968, #11820, #18396, #13675, #22681, #447, #2862, #3151, #7554, #16101, #24807, #11530, #20543, #5290, #20113, #9554, #15679, #11676, #11251, #590, #1025, #15819, #9696, #27103, #24380, #22391 ) ),
 .UNSPECIFIED., .F., .F., .F. ) 
 B_SPLINE_SURFACE_WITH_KNOTS ( ( 2, 2 ),
 ( 3, 2, 2, 2, 2, 2, 2, 2, 2, 2, 2, 2, 2, 2, 2, 2, 2, 2, 2, 2, 2, 2, 2, 2, 2, 2, 2, 2, 2, 2, 2, 2, 2, 2, 2, 2, 2, 2, 2, 2, 2, 2, 2, 2, 2, 2, 2, 2, 2, 2, 2, 2, 2, 2, 2, 2, 2, 2, 2, 2, 2, 2, 2, 2, 2, 2, 2, 2, 2, 2, 2, 2, 2, 2, 2, 2, 2, 2, 2, 2, 2, 2, 2, 2, 2, 2, 2, 2, 2, 2, 2, 3 ),
 ( 0.000000000000000000, 1.000000000000000000 ),
 ( 0.000000000000000000, 0.01041666666666666609, 0.02083333333333333218, 0.03125000000000000000, 0.04166666666666666435, 0.05208333333333333565, 0.06250000000000000000, 0.07291666666666667129, 0.08333333333333332871, 0.09375000000000000000, 0.1041666666666666713, 0.1145833333333333287, 0.1250000000000000000, 0.1354166666666666574, 0.1458333333333333426, 0.1562500000000000000, 0.1666666666666666574, 0.1770833333333333426, 0.1875000000000000000, 0.1979166666666666574, 0.2083333333333333426, 0.2187500000000000000, 0.2291666666666666574, 0.2395833333333333426, 0.2500000000000000000, 0.2604166666666666852, 0.2708333333333333148, 0.2812500000000000000, 0.2916666666666666852, 0.3020833333333333148, 0.3125000000000000000, 0.3229166666666666852, 0.3333333333333333148, 0.3437500000000000000, 0.3541666666666666852, 0.3645833333333333148, 0.3750000000000000000, 0.3854166666666666852, 0.3958333333333333148, 0.4062500000000000000, 0.4166666666666666852, 0.4270833333333333148, 0.4375000000000000000, 0.4479166666666666852, 0.4583333333333333148, 0.4687500000000000000, 0.4791666666666666852, 0.4895833333333333148, 0.5000000000000000000, 0.5104166666666666297, 0.5208333333333333703, 0.5312500000000000000, 0.5416666666666666297, 0.5520833333333333703, 0.5625000000000000000, 0.5729166666666666297, 0.5833333333333333703, 0.5937500000000000000, 0.6041666666666666297, 0.6145833333333333703, 0.6250000000000000000, 0.6354166666666666297, 0.6458333333333333703, 0.6562500000000000000, 0.6666666666666666297, 0.6770833333333333703, 0.6875000000000000000, 0.6979166666666666297, 0.7083333333333333703, 0.7187500000000000000, 0.7291666666666666297, 0.7395833333333333703, 0.7500000000000000000, 0.7604166666666666297, 0.7708333333333333703, 0.7812500000000000000, 0.7916666666666666297, 0.8020833333333333703, 0.8125000000000000000, 0.8229166666666666297, 0.8333333333333333703, 0.8437500000000000000, 0.8541666666666666297, 0.8645833333333333703, 0.8750000000000000000, 0.8854166666666666297, 0.8958333333333333703, 0.9062500000000000000, 0.9166666666666666297, 0.9270833333333333703, 0.9375000000000000000, 0.9448586970929392370 ),
 .UNSPECIFIED. ) 
 GEOMETRIC_REPRESENTATION_ITEM ( )  RATIONAL_B_SPLINE_SURFACE ( (
 ( 1.000000000000000000, 0.9238795325112867385, 1.000000000000000000, 0.9238795325112867385, 1.000000000000000000, 0.9238795325112867385, 1.000000000000000000, 0.9238795325112867385, 1.000000000000000000, 0.9238795325112867385, 1.000000000000000000, 0.9238795325112867385, 1.000000000000000000, 0.9238795325112867385, 1.000000000000000000, 0.9238795325112867385, 1.000000000000000000, 0.9238795325112867385, 1.000000000000000000, 0.9238795325112867385, 1.000000000000000000, 0.9238795325112867385, 1.000000000000000000, 0.9238795325112867385, 1.000000000000000000, 0.9238795325112867385, 1.000000000000000000, 0.9238795325112867385, 1.000000000000000000, 0.9238795325112867385, 1.000000000000000000, 0.9238795325112867385, 1.000000000000000000, 0.9238795325112867385, 1.000000000000000000, 0.9238795325112867385, 1.000000000000000000, 0.9238795325112867385, 1.000000000000000000, 0.9238795325112867385, 1.000000000000000000, 0.9238795325112867385, 1.000000000000000000, 0.9238795325112867385, 1.000000000000000000, 0.9238795325112867385, 1.000000000000000000, 0.9238795325112867385, 1.000000000000000000, 0.9238795325112867385, 1.000000000000000000, 0.9238795325112867385, 1.000000000000000000, 0.9238795325112867385, 1.000000000000000000, 0.9238795325112867385, 1.000000000000000000, 0.9238795325112867385, 1.000000000000000000, 0.9238795325112867385, 1.000000000000000000, 0.9238795325112867385, 1.000000000000000000, 0.9238795325112867385, 1.000000000000000000, 0.9238795325112867385, 1.000000000000000000, 0.9238795325112867385, 1.000000000000000000, 0.9238795325112867385, 1.000000000000000000, 0.9238795325112867385, 1.000000000000000000, 0.9238795325112867385, 1.000000000000000000, 0.9238795325112867385, 1.000000000000000000, 0.9238795325112867385, 1.000000000000000000, 0.9238795325112867385, 1.000000000000000000, 0.9238795325112867385, 1.000000000000000000, 0.9238795325112867385, 1.000000000000000000, 0.9238795325112867385, 1.000000000000000000, 0.9238795325112867385, 1.000000000000000000, 0.9238795325112867385, 1.000000000000000000, 0.9238795325112867385, 1.000000000000000000, 0.9238795325112867385, 1.000000000000000000, 0.9238795325112867385, 1.000000000000000000, 0.9238795325112867385, 1.000000000000000000, 0.9238795325112867385, 1.000000000000000000, 0.9238795325112867385, 1.000000000000000000, 0.9238795325112867385, 1.000000000000000000, 0.9238795325112867385, 1.000000000000000000, 0.9238795325112867385, 1.000000000000000000, 0.9238795325112867385, 1.000000000000000000, 0.9238795325112867385, 1.000000000000000000, 0.9238795325112867385, 1.000000000000000000, 0.9238795325112867385, 1.000000000000000000, 0.9238795325112867385, 1.000000000000000000, 0.9238795325112867385, 1.000000000000000000, 0.9238795325112867385, 1.000000000000000000, 0.9238795325112867385, 1.000000000000000000, 0.9238795325112867385, 1.000000000000000000, 0.9238795325112867385, 1.000000000000000000, 0.9238795325112867385, 1.000000000000000000, 0.9238795325112867385, 1.000000000000000000, 0.9238795325112867385, 1.000000000000000000, 0.9238795325112867385, 1.000000000000000000, 0.9238795325112867385, 1.000000000000000000, 0.9238795325112867385, 1.000000000000000000, 0.9238795325112867385, 1.000000000000000000, 0.9238795325112867385, 1.000000000000000000, 0.9238795325112867385, 1.000000000000000000, 0.9238795325112867385, 1.000000000000000000, 0.9238795325112867385, 1.000000000000000000, 0.9238795325112867385, 1.000000000000000000, 0.9238795325112867385, 1.000000000000000000, 0.9238795325112867385, 1.000000000000000000, 0.9238795325112867385, 1.000000000000000000, 0.9238795325112867385, 1.000000000000000000, 0.9238795325112867385, 1.000000000000000000, 0.9238795325112867385, 1.000000000000000000, 0.9238795325112867385, 1.000000000000000000, 0.9238795325112867385, 1.000000000000000000, 0.9238795325112867385, 1.000000000000000000, 0.9238795325112867385, 1.000000000000000000, 0.9238795325112867385, 1.000000000000000000, 0.9238795325112867385, 1.000000000000000000, 0.9238795325112867385, 1.000000000000000000, 0.9238795325112867385, 1.000000000000000000, 0.9462258435690522607, 0.9684275710300105366),
 ( 1.000000000000000000, 0.9238795325112867385, 1.000000000000000000, 0.9238795325112867385, 1.000000000000000000, 0.9238795325112867385, 1.000000000000000000, 0.9238795325112867385, 1.000000000000000000, 0.9238795325112867385, 1.000000000000000000, 0.9238795325112867385, 1.000000000000000000, 0.9238795325112867385, 1.000000000000000000, 0.9238795325112867385, 1.000000000000000000, 0.9238795325112867385, 1.000000000000000000, 0.9238795325112867385, 1.000000000000000000, 0.9238795325112867385, 1.000000000000000000, 0.9238795325112867385, 1.000000000000000000, 0.9238795325112867385, 1.000000000000000000, 0.9238795325112867385, 1.000000000000000000, 0.9238795325112867385, 1.000000000000000000, 0.9238795325112867385, 1.000000000000000000, 0.9238795325112867385, 1.000000000000000000, 0.9238795325112867385, 1.000000000000000000, 0.9238795325112867385, 1.000000000000000000, 0.9238795325112867385, 1.000000000000000000, 0.9238795325112867385, 1.000000000000000000, 0.9238795325112867385, 1.000000000000000000, 0.9238795325112867385, 1.000000000000000000, 0.9238795325112867385, 1.000000000000000000, 0.9238795325112867385, 1.000000000000000000, 0.9238795325112867385, 1.000000000000000000, 0.9238795325112867385, 1.000000000000000000, 0.9238795325112867385, 1.000000000000000000, 0.9238795325112867385, 1.000000000000000000, 0.9238795325112867385, 1.000000000000000000, 0.9238795325112867385, 1.000000000000000000, 0.9238795325112867385, 1.000000000000000000, 0.9238795325112867385, 1.000000000000000000, 0.9238795325112867385, 1.000000000000000000, 0.9238795325112867385, 1.000000000000000000, 0.9238795325112867385, 1.000000000000000000, 0.9238795325112867385, 1.000000000000000000, 0.9238795325112867385, 1.000000000000000000, 0.9238795325112867385, 1.000000000000000000, 0.9238795325112867385, 1.000000000000000000, 0.9238795325112867385, 1.000000000000000000, 0.9238795325112867385, 1.000000000000000000, 0.9238795325112867385, 1.000000000000000000, 0.9238795325112867385, 1.000000000000000000, 0.9238795325112867385, 1.000000000000000000, 0.9238795325112867385, 1.000000000000000000, 0.9238795325112867385, 1.000000000000000000, 0.9238795325112867385, 1.000000000000000000, 0.9238795325112867385, 1.000000000000000000, 0.9238795325112867385, 1.000000000000000000, 0.9238795325112867385, 1.000000000000000000, 0.9238795325112867385, 1.000000000000000000, 0.9238795325112867385, 1.000000000000000000, 0.9238795325112867385, 1.000000000000000000, 0.9238795325112867385, 1.000000000000000000, 0.9238795325112867385, 1.000000000000000000, 0.9238795325112867385, 1.000000000000000000, 0.9238795325112867385, 1.000000000000000000, 0.9238795325112867385, 1.000000000000000000, 0.9238795325112867385, 1.000000000000000000, 0.9238795325112867385, 1.000000000000000000, 0.9238795325112867385, 1.000000000000000000, 0.9238795325112867385, 1.000000000000000000, 0.9238795325112867385, 1.000000000000000000, 0.9238795325112867385, 1.000000000000000000, 0.9238795325112867385, 1.000000000000000000, 0.9238795325112867385, 1.000000000000000000, 0.9238795325112867385, 1.000000000000000000, 0.9238795325112867385, 1.000000000000000000, 0.9238795325112867385, 1.000000000000000000, 0.9238795325112867385, 1.000000000000000000, 0.9238795325112867385, 1.000000000000000000, 0.9238795325112867385, 1.000000000000000000, 0.9238795325112867385, 1.000000000000000000, 0.9238795325112867385, 1.000000000000000000, 0.9238795325112867385, 1.000000000000000000, 0.9238795325112867385, 1.000000000000000000, 0.9238795325112867385, 1.000000000000000000, 0.9238795325112867385, 1.000000000000000000, 0.9238795325112867385, 1.000000000000000000, 0.9238795325112867385, 1.000000000000000000, 0.9238795325112867385, 1.000000000000000000, 0.9238795325112867385, 1.000000000000000000, 0.9238795325112867385, 1.000000000000000000, 0.9238795325112867385, 1.000000000000000000, 0.9238795325112867385, 1.000000000000000000, 0.9238795325112867385, 1.000000000000000000, 0.9238795325112867385, 1.000000000000000000, 0.9238795325112867385, 1.000000000000000000, 0.9238795325112867385, 1.000000000000000000, 0.9462258435690522607, 0.9684275710300105366) ) ) 
 REPRESENTATION_ITEM ( '' )  SURFACE ( )  );
#12369 = DIRECTION ( 'NONE',  ( 0.000000000000000000, 1.000000000000000000, 0.000000000000000000 ) ) ;
#12370 = CARTESIAN_POINT ( 'NONE',  ( 143.1451861577818363, 38.61875000108392442, -5.444914386472297529 ) ) ;
#12371 = CARTESIAN_POINT ( 'NONE',  ( 13.14518615778179900, 32.46718750108393436, -5.444914386472297529 ) ) ;
#12372 = DIRECTION ( 'NONE',  ( -0.000000000000000000, -1.000000000000000000, -0.000000000000000000 ) ) ;
#12373 = DIRECTION ( 'NONE',  ( -0.000000000000000000, -1.000000000000000000, -0.000000000000000000 ) ) ;
#12374 = LINE ( 'NONE', #25921, #7979 ) ;
#12375 = CARTESIAN_POINT ( 'NONE',  ( 102.0669872999999939, 122.8000000010924708, -0.8561741729129507261 ) ) ;
#12376 = CARTESIAN_POINT ( 'NONE',  ( 185.4011555911795313, 39.31328124999999574, -9.598844408820458085 ) ) ;
#12377 = CARTESIAN_POINT ( 'NONE',  ( 65.00000000000000000, 39.61093749999999147, 13.57481594606304576 ) ) ;
#12378 = CARTESIAN_POINT ( 'NONE',  ( 95.54126587499995082, 1.846868145590750077, 4.625000001365592084 ) ) ;
#12379 = CARTESIAN_POINT ( 'NONE',  ( 65.00000000000000000, 37.57695312608392868, 13.14518615778179544 ) ) ;
#12380 = EDGE_CURVE ( 'NONE', #4040, #19447, #21450, .T. ) ;
#12381 = CARTESIAN_POINT ( 'NONE',  ( 95.54126587499996504, 1.846868145590750077, 7.375000001365592084 ) ) ;
#12382 = CARTESIAN_POINT ( 'NONE',  ( 107.0000000000000142, 107.7255621263696526, -47.60000000546237686 ) ) ;
#12383 = CARTESIAN_POINT ( 'NONE',  ( 96.84719886470463734, 93.93749999863440792, -3.152801135295366208 ) ) ;
#12384 = CARTESIAN_POINT ( 'NONE',  ( 9.598844408820459861, 39.71015624999999716, 9.598844408820456309 ) ) ;
#12385 = CARTESIAN_POINT ( 'NONE',  ( 124.3771271284221740, 39.26367187500000000, -13.57481594606310260 ) ) ;
#12386 = CARTESIAN_POINT ( 'NONE',  ( 13.57481594606304931, 38.96601562499999005, 5.622872871577869525 ) ) ;
#12387 = ORIENTED_EDGE ( 'NONE', *, *, #3399, .F. ) ;
#12388 = CARTESIAN_POINT ( 'NONE',  ( 3.061616997868384226E-15, 23.00000000000000000, 25.00000000000001066 ) ) ;
#12389 = ORIENTED_EDGE ( 'NONE', *, *, #27810, .F. ) ;
#12390 = VECTOR ( 'NONE', #11360, 1000.000000000000000 ) ;
#12391 = EDGE_LOOP ( 'NONE', ( #6508, #27570, #1038, #25618 ) ) ;
#12392 = CARTESIAN_POINT ( 'NONE',  ( 95.54126587499995082, 1.846868145590750077, 8.625000001365593860 ) ) ;
#12393 = ORIENTED_EDGE ( 'NONE', *, *, #19253, .F. ) ;
#12394 = CARTESIAN_POINT ( 'NONE',  ( 108.0825317500000011, 112.6261737610028320, -46.27500000273120406 ) ) ;
#12395 = CARTESIAN_POINT ( 'NONE',  ( 2.414731522848535132E-15, 34.40195312608393152, 13.14518615778179544 ) ) ;
#12396 = CARTESIAN_POINT ( 'NONE',  ( 181.4251840539369596, 40.30546875216787583, 0.000000000000000000 ) ) ;
#12397 = CARTESIAN_POINT ( 'NONE',  ( -5.444914386472299306, 39.11484375108393863, 13.14518615778179722 ) ) ;
#12398 = CARTESIAN_POINT ( 'NONE',  ( 99.99999999999998579, 118.4984768113314146, -49.62500000273118417 ) ) ;
#12399 = CARTESIAN_POINT ( 'NONE',  ( 130.0000000000000000, 38.17226562608394147, -13.14518615778179544 ) ) ;
#12400 = CARTESIAN_POINT ( 'NONE',  ( 5.444914386472302859, 32.07031250108393294, 13.14518615778179189 ) ) ;
#12401 = EDGE_LOOP ( 'NONE', ( #1046, #17570, #21566, #26277, #10144, #22144, #4984, #16525 ) ) ;
#12402 = CARTESIAN_POINT ( 'NONE',  ( 65.00000000000000000, 37.22968749999999716, 13.57481594606304576 ) ) ;
#12403 = CARTESIAN_POINT ( 'NONE',  ( 2.493653234604083739E-15, 34.15390625216787157, 13.57481594606304576 ) ) ;
#12404 = AXIS2_PLACEMENT_3D ( 'NONE', #2184, #26262, #15118 ) ;
#12405 = CARTESIAN_POINT ( 'NONE',  ( 107.0000000000000142, 112.2744378736303190, -46.90000000000001279 ) ) ;
#12406 =( BOUNDED_CURVE ( )  B_SPLINE_CURVE ( 2, ( #16767, #25737, #8211, #6221, #14614, #18904, #1540, #25598, #17034, #14889, #23331, #16900, #27751, #14748, #3805, #10192, #27615, #8071, #25468, #12465, #21334, #12608, #21190, #23470, #6082, #3948, #27887, #1676, #10333, #1813, #19040, #10477, #23607, #10146, #14573, #14011, #1077, #18309, #12011, #3201, #12287 ),
 .UNSPECIFIED., .F., .F. ) 
 B_SPLINE_CURVE_WITH_KNOTS ( ( 3, 2, 2, 2, 2, 2, 2, 2, 2, 2, 2, 2, 2, 2, 2, 2, 2, 2, 2, 2, 3 ),
 ( 0.000000000000000000, 0.04166666666666666435, 0.08333333333333332871, 0.1250000000000000000, 0.1666666666666666574, 0.2083333333333333426, 0.2500000000000000000, 0.2916666666666666852, 0.3333333333333333148, 0.3750000000000000000, 0.4166666666666666852, 0.4583333333333332593, 0.5000000000000000000, 0.5416666666666666297, 0.5833333333333333703, 0.6250000000000000000, 0.6666666666666666297, 0.7083333333333333703, 0.7500000000000000000, 0.7916666666666666297, 0.8333333333333333703 ),
 .UNSPECIFIED. ) 
 CURVE ( )  GEOMETRIC_REPRESENTATION_ITEM ( )  RATIONAL_B_SPLINE_CURVE ( ( 1.000000000000000000, 0.9238795325112867385, 1.000000000000000000, 0.9238795325112867385, 1.000000000000000000, 0.9238795325112867385, 1.000000000000000000, 0.9238795325112867385, 1.000000000000000000, 0.9238795325112867385, 1.000000000000000000, 0.9238795325112867385, 1.000000000000000000, 0.9238795325112867385, 1.000000000000000000, 0.9238795325112867385, 1.000000000000000000, 0.9238795325112867385, 1.000000000000000000, 0.9238795325112867385, 1.000000000000000000, 0.9238795325112867385, 1.000000000000000000, 0.9238795325112867385, 1.000000000000000000, 0.9238795325112867385, 1.000000000000000000, 0.9238795325112867385, 1.000000000000000000, 0.9238795325112867385, 1.000000000000000000, 0.9238795325112867385, 1.000000000000000000, 0.9238795325112867385, 1.000000000000000000, 0.9238795325112867385, 1.000000000000000000, 0.9238795325112867385, 1.000000000000000000, 0.9238795325112867385, 1.000000000000000000 ) ) 
 REPRESENTATION_ITEM ( '' )  );
#12407 = CARTESIAN_POINT ( 'NONE',  ( 101.8468681455906903, -4.458734124999987891, 5.750000001365591196 ) ) ;
#12408 = CARTESIAN_POINT ( 'NONE',  ( 9.295050272127047819, 33.11210937608393579, 9.295050272127046043 ) ) ;
#12409 = CARTESIAN_POINT ( 'NONE',  ( 104.4587341249999639, 1.442382525525748735E-14, 3.187500001365592972 ) ) ;
#12410 = EDGE_CURVE ( 'NONE', #21487, #27401, #20574, .T. ) ;
#12411 = CARTESIAN_POINT ( 'NONE',  ( 104.4587341249999639, 84.18750000136560629, -1.442382525525748735E-14 ) ) ;
#12412 = CARTESIAN_POINT ( 'NONE',  ( 5.444914386472297529, 33.95546875108393436, -13.14518615778179900 ) ) ;
#12413 = CARTESIAN_POINT ( 'NONE',  ( -13.14518615778179900, 39.11484375108394573, -5.444914386472297529 ) ) ;
#12414 = CARTESIAN_POINT ( 'NONE',  ( 74.18017581364799184, 55.00000000000000000, 14.99999999999997868 ) ) ;
#12415 = VERTEX_POINT ( 'NONE', #27276 ) ;
#12416 = ADVANCED_FACE ( 'NONE', ( #1055 ), #3743, .T. ) ;
#12417 = PRESENTATION_STYLE_ASSIGNMENT (( #27417 ) ) ;
#12418 = CARTESIAN_POINT ( 'NONE',  ( 106.9999999999999858, 107.7255621263696810, -53.59999999453763309 ) ) ;
#12419 = DIRECTION ( 'NONE',  ( 1.000000000000000000, 0.000000000000000000, -5.782411586589357392E-17 ) ) ;
#12420 = CYLINDRICAL_SURFACE ( 'NONE', #9089, 13.57481594606304398 ) ;
#12421 = CARTESIAN_POINT ( 'NONE',  ( 93.46109445667489979, 114.7507929638356785, -54.07499999726881867 ) ) ;
#12422 = CARTESIAN_POINT ( 'NONE',  ( 130.0000000000000000, 39.71015625216787015, 13.57481594606304576 ) ) ;
#12423 = VERTEX_POINT ( 'NONE', #12403 ) ;
#12424 = CARTESIAN_POINT ( 'NONE',  ( 65.00000000000000000, 39.75976562608394005, -13.14518615778179544 ) ) ;
#12425 = CARTESIAN_POINT ( 'NONE',  ( 5.622872871577924592, 32.61601562716786873, 13.57481594606299957 ) ) ;
#12426 = ADVANCED_FACE ( 'NONE', ( #5464 ), #14133, .T. ) ;
#12427 = ORIENTED_EDGE ( 'NONE', *, *, #3913, .T. ) ;
#12428 = CARTESIAN_POINT ( 'NONE',  ( 78.57481594606305464, 37.37851562499999858, 5.622872871577868636 ) ) ;
#12429 = CARTESIAN_POINT ( 'NONE',  ( 124.3771271284220319, 37.97382812499999716, 13.57481594606295161 ) ) ;
#12430 = DIRECTION ( 'NONE',  ( -1.000000000000000000, 0.000000000000000000, 0.000000000000000000 ) ) ;
#12431 = CARTESIAN_POINT ( 'NONE',  ( 135.6228728715778686, 36.08867187716787583, -13.57481594606304753 ) ) ;
#12432 = CARTESIAN_POINT ( 'NONE',  ( 102.1631189606246153, 116.6573956140660897, -47.09999999453764019 ) ) ;
#12433 = CARTESIAN_POINT ( 'NONE',  ( 204.2950502721270425, 36.48554687608393721, -9.295050272127046043 ) ) ;
#12434 = ORIENTED_EDGE ( 'NONE', *, *, #17480, .T. ) ;
#12435 = FACE_OUTER_BOUND ( 'NONE', #18045, .T. ) ;
#12436 = CARTESIAN_POINT ( 'NONE',  ( 102.0710678118654613, 90.81249999999995737, 4.999999999999974243 ) ) ;
#12437 = EDGE_CURVE ( 'NONE', #13724, #10805, #16843, .T. ) ;
#12438 = LINE ( 'NONE', #12163, #21994 ) ;
#12439 = CARTESIAN_POINT ( 'NONE',  ( -20.00000000000000355, 55.00000000000000000, -14.99999999999999822 ) ) ;
#12440 = CYLINDRICAL_SURFACE ( 'NONE', #28192, 5.000000000000000888 ) ;
#12441 = FACE_OUTER_BOUND ( 'NONE', #10248, .T. ) ;
#12442 = CARTESIAN_POINT ( 'NONE',  ( 12.53142549111993098, 36.00000000000000711, -5.200562670743043903 ) ) ;
#12443 = DIRECTION ( 'NONE',  ( -0.000000000000000000, 1.000000000000000000, -0.000000000000000000 ) ) ;
#12444 = CARTESIAN_POINT ( 'NONE',  ( 91.91746824999997045, 112.6261737610028320, -45.72499999726882436 ) ) ;
#12445 = ADVANCED_FACE ( 'NONE', ( #11993 ), #7731, .F. ) ;
#12446 = ORIENTED_EDGE ( 'NONE', *, *, #27435, .T. ) ;
#12447 = CARTESIAN_POINT ( 'NONE',  ( 9.598844408820459861, 39.71015624999999716, 9.598844408820456309 ) ) ;
#12448 = CARTESIAN_POINT ( 'NONE',  ( -8.312177448680279460E-16, 31.37578125216787583, -13.57481594606304576 ) ) ;
#12449 = ORIENTED_EDGE ( 'NONE', *, *, #23995, .T. ) ;
#12450 = CARTESIAN_POINT ( 'NONE',  ( 97.92893218813451028, 5.000000000000018652, 3.937500002731185056 ) ) ;
#12451 = CARTESIAN_POINT ( 'NONE',  ( 136.9444263933115167, 31.55306875057403104, -11.16113171639042356 ) ) ;
#12452 = CARTESIAN_POINT ( 'NONE',  ( 55.70494972787295751, 38.27148437608393294, 9.295050272127047819 ) ) ;
#12453 = EDGE_CURVE ( 'NONE', #26359, #6320, #26430, .T. ) ;
#12454 = CARTESIAN_POINT ( 'NONE',  ( 201.9444263933115167, 31.55306875057403104, -11.16113171639042356 ) ) ;
#12455 = CARTESIAN_POINT ( 'NONE',  ( 56.87469608220845174, 36.00000000000000000, 10.34220695173551441 ) ) ;
#12456 = CARTESIAN_POINT ( 'NONE',  ( -13.14518615778179544, 34.20351562608393436, 0.000000000000000000 ) ) ;
#12457 = CARTESIAN_POINT ( 'NONE',  ( 0.000000000000000000, 50.00000000000000000, 13.57481594606304398 ) ) ;
#12458 = CARTESIAN_POINT ( 'NONE',  ( 0.000000000000000000, 21.95886589889650509, -23.00000000000001421 ) ) ;
#12459 = CARTESIAN_POINT ( 'NONE',  ( 99.99999999999998579, 93.12499999726881583, -4.999999999999997335 ) ) ;
#12460 = DIRECTION ( 'NONE',  ( 0.000000000000000000, 0.000000000000000000, 1.000000000000000000 ) ) ;
#12461 = CARTESIAN_POINT ( 'NONE',  ( 5.444914386472297529, 37.13046875108393152, -13.14518615778179900 ) ) ;
#12462 = CARTESIAN_POINT ( 'NONE',  ( 195.0000000000000000, -7.395377635281828788, -2.255140518769849538E-14 ) ) ;
#12463 = CARTESIAN_POINT ( 'NONE',  ( 102.4999999999999716, 123.7500000000000142, 1.035533905932722876 ) ) ;
#12464 = DIRECTION ( 'NONE',  ( 0.000000000000000000, 0.7071067811865469066, 0.7071067811865482389 ) ) ;
#12465 = CARTESIAN_POINT ( 'NONE',  ( 99.14382582708708469, 123.8000000010924566, -2.066987299999998751 ) ) ;
#12466 = VECTOR ( 'NONE', #26545, 1000.000000000000000 ) ;
#12467 = CARTESIAN_POINT ( 'NONE',  ( 185.4011555911795313, 39.41250000216787441, -9.598844408820458085 ) ) ;
#12468 = CARTESIAN_POINT ( 'NONE',  ( 101.8468681455906903, 4.458734125000016313, 12.12500000136559208 ) ) ;
#12469 = CARTESIAN_POINT ( 'NONE',  ( -5.622872871577688336, 32.21914062716787441, -13.57481594606323050 ) ) ;
#12470 = ORIENTED_EDGE ( 'NONE', *, *, #22061, .T. ) ;
#12471 = DIRECTION ( 'NONE',  ( 1.000000000000000000, 0.000000000000000000, 0.000000000000000000 ) ) ;
#12472 = CARTESIAN_POINT ( 'NONE',  ( -9.295050272127046043, 32.71523437608393436, -9.295050272127046043 ) ) ;
#12473 = CARTESIAN_POINT ( 'NONE',  ( 13.14518615778179722, 33.85625000108393579, -5.444914386472297529 ) ) ;
#12474 = CARTESIAN_POINT ( 'NONE',  ( 9.598844408820456309, 32.86406250216787583, -9.598844408820458085 ) ) ;
#12475 = DIRECTION ( 'NONE',  ( -5.782411586589357392E-17, 0.000000000000000000, -1.000000000000000000 ) ) ;
#12476 = CARTESIAN_POINT ( 'NONE',  ( 98.15313185440925281, 81.25000000136560629, -4.458734125000016313 ) ) ;
#12477 = CARTESIAN_POINT ( 'NONE',  ( 51.85481384221820633, 39.16445312608393436, 0.000000000000000000 ) ) ;
#12478 = CARTESIAN_POINT ( 'NONE',  ( 99.99999999999998579, 101.5015231886685854, -48.87500000273119838 ) ) ;
#12479 = CARTESIAN_POINT ( 'NONE',  ( 99.99999999999995737, 5.000000000000018652, 11.75000000000000000 ) ) ;
#12480 = CARTESIAN_POINT ( 'NONE',  ( 99.14382582708707048, 123.8000000010924850, -2.066987299999999195 ) ) ;
#12481 = DIRECTION ( 'NONE',  ( 1.000000000000000000, 0.000000000000000000, 0.000000000000000000 ) ) ;
#12482 = CARTESIAN_POINT ( 'NONE',  ( 95.67376207875069838, 104.0454443415356991, -52.19999999453764872 ) ) ;
#12483 = CARTESIAN_POINT ( 'NONE',  ( 143.1451861577818079, 32.36796875108393579, 5.444914386472293977 ) ) ;
#12484 = EDGE_CURVE ( 'NONE', #20385, #9261, #3124, .T. ) ;
#12485 = ORIENTED_EDGE ( 'NONE', *, *, #16095, .T. ) ;
#12486 = CARTESIAN_POINT ( 'NONE',  ( 93.00000000000002842, 112.2744378736303759, -50.10000000000000853 ) ) ;
#12487 = CARTESIAN_POINT ( 'NONE',  ( 9.295050272127046043, 38.86679687608393863, -9.295050272127046043 ) ) ;
#12488 = CARTESIAN_POINT ( 'NONE',  ( 103.1528011352953342, 80.81250000136559208, 3.152801135295355106 ) ) ;
#12489 = DIRECTION ( 'NONE',  ( 0.000000000000000000, -1.000000000000000000, 0.000000000000000000 ) ) ;
#12490 = CARTESIAN_POINT ( 'NONE',  ( 78.57481594606304043, 37.57695312716787583, -5.622872871577873077 ) ) ;
#12491 = VECTOR ( 'NONE', #25455, 999.9999999999998863 ) ;
#12492 = CARTESIAN_POINT ( 'NONE',  ( 97.50236033167490746, 102.3130555110000159, -51.22499999726882436 ) ) ;
#12493 = CARTESIAN_POINT ( 'NONE',  ( -5.622872871577873077, 35.69179687716786731, 13.57481594606304753 ) ) ;
#12494 = VERTEX_POINT ( 'NONE', #15099 ) ;
#12495 = CARTESIAN_POINT ( 'NONE',  ( 99.99999999999995737, -4.999999999999990230, 8.250000000000000000 ) ) ;
#12496 = ORIENTED_EDGE ( 'NONE', *, *, #24272, .T. ) ;
#12497 = CARTESIAN_POINT ( 'NONE',  ( 204.2950502721270425, 36.28710937608393294, -9.295050272127046043 ) ) ;
#12498 = CARTESIAN_POINT ( 'NONE',  ( -20.00000000000000000, 80.00000000000000000, 10.00000000000000000 ) ) ;
#12499 = CARTESIAN_POINT ( 'NONE',  ( 139.2950502721270425, 38.46992187608393010, 9.295050272127046043 ) ) ;
#12500 = CYLINDRICAL_SURFACE ( 'NONE', #7327, 2.499999999999995115 ) ;
#12501 = CARTESIAN_POINT ( 'NONE',  ( 96.46446609406721961, 3.535533905932755072, 12.00000000273118594 ) ) ;
#12502 = CARTESIAN_POINT ( 'NONE',  ( 103.1528011352953484, 93.18749999863440792, 3.152801135295352886 ) ) ;
#12503 = DIRECTION ( 'NONE',  ( 0.000000000000000000, 0.000000000000000000, 1.000000000000000000 ) ) ;
#12504 = CARTESIAN_POINT ( 'NONE',  ( 9.295050272127046043, 40.25585937608393294, -9.295050272127046043 ) ) ;
#12505 = CARTESIAN_POINT ( 'NONE',  ( 208.5748159460630688, 36.63437499999999858, -1.662435489736055892E-15 ) ) ;
#12506 = APPLICATION_PROTOCOL_DEFINITION ( 'draft international standard', 'automotive_design', 1998, #20076 ) ;
#12507 = CARTESIAN_POINT ( 'NONE',  ( 13.57481594606304931, 35.79101562499999289, 5.622872871577868636 ) ) ;
#12508 = CARTESIAN_POINT ( 'NONE',  ( 103.1528011352953342, -3.152801135295355106, 4.062500001365592084 ) ) ;
#12509 = CARTESIAN_POINT ( 'NONE',  ( 78.14518615778179367, 40.20625000108393010, -5.444914386472297529 ) ) ;
#12510 = CIRCLE ( 'NONE', #26655, 5.000000000000000888 ) ;
#12511 = CARTESIAN_POINT ( 'NONE',  ( 98.15313185440923860, 4.458734125000016313, 6.250000001365592084 ) ) ;
#12512 = CARTESIAN_POINT ( 'NONE',  ( 99.99999999999998579, 90.00000000000000000, -4.999999999999996447 ) ) ;
#12513 = CARTESIAN_POINT ( 'NONE',  ( 98.15313185440925281, 94.24999999863439371, 4.458734124999979898 ) ) ;
#12514 = CARTESIAN_POINT ( 'NONE',  ( 130.0000000000000000, 39.61093749999999147, 13.57481594606304576 ) ) ;
#12515 = CARTESIAN_POINT ( 'NONE',  ( -5.622872871577873077, 39.26367187499999289, -13.57481594606304753 ) ) ;
#12516 = ORIENTED_EDGE ( 'NONE', *, *, #20742, .F. ) ;
#12517 = CARTESIAN_POINT ( 'NONE',  ( 99.99999999999995737, 81.93750000136559208, 4.458734124999988779 ) ) ;
#12518 = CIRCLE ( 'NONE', #20740, 5.000000000000000888 ) ;
#12519 = AXIS2_PLACEMENT_3D ( 'NONE', #20258, #744, #17693 ) ;
#12520 = DIRECTION ( 'NONE',  ( 0.000000000000000000, 1.000000000000000000, 0.000000000000000000 ) ) ;
#12521 = ORIENTED_EDGE ( 'NONE', *, *, #11267, .T. ) ;
#12522 = CARTESIAN_POINT ( 'NONE',  ( 204.5988444088204687, 37.42812500216787441, 9.598844408820456309 ) ) ;
#12523 = EDGE_LOOP ( 'NONE', ( #3753, #5091, #8553, #9757 ) ) ;
#12524 =( BOUNDED_CURVE ( )  B_SPLINE_CURVE ( 2, ( #27082, #20378, #20231, #18235, #714, #18085, #9536, #26944, #5270, #13935, #14910 ),
 .UNSPECIFIED., .F., .F. ) 
 B_SPLINE_CURVE_WITH_KNOTS ( ( 3, 2, 2, 2, 2, 3 ),
 ( 0.2000000000000001776, 0.2200000000000001676, 0.2400000000000001854, 0.2600000000000002309, 0.2800000000000002487, 0.3000000000000002109 ),
 .UNSPECIFIED. ) 
 CURVE ( )  GEOMETRIC_REPRESENTATION_ITEM ( )  RATIONAL_B_SPLINE_CURVE ( ( 0.9999999999999995559, 0.9510565162951539753, 1.000000000000000000, 0.9510565162951535312, 1.000000000000000000, 0.9510565162951535312, 1.000000000000000000, 0.9510565162951535312, 1.000000000000000000, 0.9510565162951529761, 1.000000000000000444 ) ) 
 REPRESENTATION_ITEM ( '' )  );
#12525 = CARTESIAN_POINT ( 'NONE',  ( 99.99999999999995737, 78.00000000000000000, -1.387778780781445676E-14 ) ) ;
#12526 = CARTESIAN_POINT ( 'NONE',  ( 103.1528011352953342, 3.152801135295383084, 6.312500001365592084 ) ) ;
#12527 = EDGE_CURVE ( 'NONE', #487, #16572, #10415, .T. ) ;
#12528 = ORIENTED_EDGE ( 'NONE', *, *, #2192, .T. ) ;
#12529 = CARTESIAN_POINT ( 'NONE',  ( 13.14518615778179722, 34.74921875108395142, 5.444914386472293977 ) ) ;
#12530 = CARTESIAN_POINT ( 'NONE',  ( 13.14518615778179900, 32.96328125108393436, 5.444914386472293977 ) ) ;
#12531 = CARTESIAN_POINT ( 'NONE',  ( 189.3771271284221314, 38.56914062716788294, -13.57481594606304753 ) ) ;
#12532 = CARTESIAN_POINT ( 'NONE',  ( 95.67376207875072680, 115.9545556584642867, -53.30000000000000426 ) ) ;
#12533 = DIRECTION ( 'NONE',  ( 0.000000000000000000, 0.000000000000000000, 1.000000000000000000 ) ) ;
#12534 = CARTESIAN_POINT ( 'NONE',  ( 196.5054921815576563, 53.60078691996476152, 14.99999999999994671 ) ) ;
#12535 = CARTESIAN_POINT ( 'NONE',  ( 2.414731522848535132E-15, 36.18789062608393436, 13.14518615778179544 ) ) ;
#12536 = CARTESIAN_POINT ( 'NONE',  ( -13.14518615778179189, 39.21406250108392300, 5.444914386472304635 ) ) ;
#12537 = VERTEX_POINT ( 'NONE', #4020 ) ;
#12538 = CARTESIAN_POINT ( 'NONE',  ( 51.42518405393695957, 39.36289062499999858, -5.622872871577873077 ) ) ;
#12539 = TOROIDAL_SURFACE ( 'NONE', #743, 23.26794919243112858, 1.000000000000000000 ) ;
#12540 = CARTESIAN_POINT ( 'NONE',  ( 5.622872871577928144, 38.46992187716787726, -13.57481594606299247 ) ) ;
#12541 = DIRECTION ( 'NONE',  ( 1.000000000000000000, 0.000000000000000000, 0.000000000000000000 ) ) ;
#12542 = CARTESIAN_POINT ( 'NONE',  ( 95.54126587499995082, -1.846868145590724986, 3.500000001365591196 ) ) ;
#12543 = CARTESIAN_POINT ( 'NONE',  ( -13.14518615778179900, 32.76484375108393010, -5.444914386472297529 ) ) ;
#12544 = CARTESIAN_POINT ( 'NONE',  ( 95.54126587499996504, -1.846868145590724986, 1.750000001365591862 ) ) ;
#12545 = DIRECTION ( 'NONE',  ( 0.000000000000000000, 0.000000000000000000, -1.000000000000000000 ) ) ;
#12546 = CARTESIAN_POINT ( 'NONE',  ( -13.14518615778179544, 31.82226562608393650, 0.000000000000000000 ) ) ;
#12547 = CARTESIAN_POINT ( 'NONE',  ( -9.295050272127044266, 38.46992187608393721, 9.295050272127047819 ) ) ;
#12548 = CARTESIAN_POINT ( 'NONE',  ( 73.39221529163837943, 54.99999999999997158, 14.99999999999997158 ) ) ;
#12549 = VERTEX_POINT ( 'NONE', #28102 ) ;
#12550 = CARTESIAN_POINT ( 'NONE',  ( 99.99999999999998579, 90.00000000000000000, 4.999999999999983125 ) ) ;
#12551 = CIRCLE ( 'NONE', #299, 13.57481594606304398 ) ;
#12552 = CARTESIAN_POINT ( 'NONE',  ( 107.0000000000000000, 110.0000000000000000, -53.49999999453763877 ) ) ;
#12553 = CARTESIAN_POINT ( 'NONE',  ( 98.15313185440923860, 94.87499999863440792, -4.458734124999994997 ) ) ;
#12554 = CARTESIAN_POINT ( 'NONE',  ( 103.5355339059327093, -3.535533905932726206, 3.500000002731184612 ) ) ;
#12555 = CARTESIAN_POINT ( 'NONE',  ( 95.00472066334982912, 116.8754121666685393, -54.17499999726881299 ) ) ;
#12556 = CARTESIAN_POINT ( 'NONE',  ( 99.99999999999998579, 93.75000000000000000, 4.999999999999984013 ) ) ;
#12557 = AXIS2_PLACEMENT_3D ( 'NONE', #7535, #16372, #20664 ) ;
#12558 = ORIENTED_EDGE ( 'NONE', *, *, #5141, .F. ) ;
#12559 = CARTESIAN_POINT ( 'NONE',  ( 55.70494972787295751, 37.67617187608393436, 9.295050272127047819 ) ) ;
#12560 = DIRECTION ( 'NONE',  ( 0.000000000000000000, 0.000000000000000000, -1.000000000000000000 ) ) ;
#12561 = PLANE ( 'NONE',  #17581 ) ;
#12562 = EDGE_LOOP ( 'NONE', ( #26114, #5542, #17197, #11380, #5060 ) ) ;
#12563 = CARTESIAN_POINT ( 'NONE',  ( 99.99999999999998579, 128.0000000000000000, -5.204170427930421283E-15 ) ) ;
#12564 = DIRECTION ( 'NONE',  ( 0.000000000000000000, 1.000000000000000000, 0.000000000000000000 ) ) ;
#12565 = CARTESIAN_POINT ( 'NONE',  ( 99.14382582708707048, 123.8000000010924850, -2.066987299999999195 ) ) ;
#12566 = CARTESIAN_POINT ( 'NONE',  ( 143.5748159460630404, 35.89023437716787868, 5.622872871577869525 ) ) ;
#12567 = ADVANCED_FACE ( 'NONE', ( #12686 ), #21546, .F. ) ;
#12568 =( BOUNDED_SURFACE ( )  B_SPLINE_SURFACE ( 1, 2, ( 
 ( #550, #9512, #7365, #11633, #2688, #11778, #22493, #1124, #26778, #20640, #16352, #2958, #694, #9367, #22782, #9651, #18062, #5249, #841, #18212, #16060, #24768, #7512, #25051, #16206, #13914, #17924, #22641, #3109, #24910, #5393, #14337, #3674, #1260, #14481, #25736, #9922, #3532, #12607, #22922, #25185 ),
 ( #8070, #21333, #21055, #18772, #3381, #8210, #18903, #5673, #18638, #16899, #6220, #1539, #20918, #25597, #27342, #12189, #16631, #1400, #10476, #27477, #12052, #7801, #5810, #17033, #27750, #23198, #6081, #12336, #10060, #3804, #10191, #27886, #27614, #7934, #19184, #25323, #10332, #14747, #16490, #23055, #1812 ) ),
 .UNSPECIFIED., .F., .F., .F. ) 
 B_SPLINE_SURFACE_WITH_KNOTS ( ( 2, 2 ),
 ( 3, 2, 2, 2, 2, 2, 2, 2, 2, 2, 2, 2, 2, 2, 2, 2, 2, 2, 2, 2, 3 ),
 ( 0.000000000000000000, 1.000000000000000000 ),
 ( 0.000000000000000000, 0.04166666666666666435, 0.08333333333333332871, 0.1250000000000000000, 0.1666666666666666574, 0.2083333333333333426, 0.2500000000000000000, 0.2916666666666666852, 0.3333333333333333148, 0.3750000000000000000, 0.4166666666666666852, 0.4583333333333333148, 0.5000000000000000000, 0.5416666666666666297, 0.5833333333333333703, 0.6250000000000000000, 0.6666666666666666297, 0.7083333333333333703, 0.7500000000000000000, 0.7916666666666666297, 0.8333333333333333703 ),
 .UNSPECIFIED. ) 
 GEOMETRIC_REPRESENTATION_ITEM ( )  RATIONAL_B_SPLINE_SURFACE ( (
 ( 1.000000000000000000, 0.9238795325112867385, 1.000000000000000000, 0.9238795325112867385, 1.000000000000000000, 0.9238795325112867385, 1.000000000000000000, 0.9238795325112867385, 1.000000000000000000, 0.9238795325112867385, 1.000000000000000000, 0.9238795325112867385, 1.000000000000000000, 0.9238795325112867385, 1.000000000000000000, 0.9238795325112867385, 1.000000000000000000, 0.9238795325112867385, 1.000000000000000000, 0.9238795325112867385, 1.000000000000000000, 0.9238795325112867385, 1.000000000000000000, 0.9238795325112867385, 1.000000000000000000, 0.9238795325112867385, 1.000000000000000000, 0.9238795325112867385, 1.000000000000000000, 0.9238795325112867385, 1.000000000000000000, 0.9238795325112867385, 1.000000000000000000, 0.9238795325112867385, 1.000000000000000000, 0.9238795325112867385, 1.000000000000000000, 0.9238795325112867385, 1.000000000000000000, 0.9238795325112867385, 1.000000000000000000),
 ( 1.000000000000000000, 0.9238795325112867385, 1.000000000000000000, 0.9238795325112867385, 1.000000000000000000, 0.9238795325112867385, 1.000000000000000000, 0.9238795325112867385, 1.000000000000000000, 0.9238795325112867385, 1.000000000000000000, 0.9238795325112867385, 1.000000000000000000, 0.9238795325112867385, 1.000000000000000000, 0.9238795325112867385, 1.000000000000000000, 0.9238795325112867385, 1.000000000000000000, 0.9238795325112867385, 1.000000000000000000, 0.9238795325112867385, 1.000000000000000000, 0.9238795325112867385, 1.000000000000000000, 0.9238795325112867385, 1.000000000000000000, 0.9238795325112867385, 1.000000000000000000, 0.9238795325112867385, 1.000000000000000000, 0.9238795325112867385, 1.000000000000000000, 0.9238795325112867385, 1.000000000000000000, 0.9238795325112867385, 1.000000000000000000, 0.9238795325112867385, 1.000000000000000000, 0.9238795325112867385, 1.000000000000000000) ) ) 
 REPRESENTATION_ITEM ( '' )  SURFACE ( )  );
#12569 = CARTESIAN_POINT ( 'NONE',  ( 51.85481384221820633, 39.95820312608393010, 0.000000000000000000 ) ) ;
#12570 = FACE_OUTER_BOUND ( 'NONE', #16407, .T. ) ;
#12571 = CARTESIAN_POINT ( 'NONE',  ( 189.5550856135277229, 37.42812500108394147, -13.14518615778179900 ) ) ;
#12572 = ORIENTED_EDGE ( 'NONE', *, *, #23954, .F. ) ;
#12573 = VERTEX_POINT ( 'NONE', #16973 ) ;
#12574 = CARTESIAN_POINT ( 'NONE',  ( 13.14518615778179544, 34.60039062608392868, -1.609821015232357215E-15 ) ) ;
#12575 = SURFACE_STYLE_USAGE ( .BOTH. , #21582 ) ;
#12576 = DIRECTION ( 'NONE',  ( 0.000000000000000000, 0.000000000000000000, 1.000000000000000000 ) ) ;
#12577 = CARTESIAN_POINT ( 'NONE',  ( 99.99999999999995737, 85.00000000000000000, -5.000000000000018652 ) ) ;
#12578 = CARTESIAN_POINT ( 'NONE',  ( 104.9999999999999716, 2.071067811865496822, 13.56250000000000000 ) ) ;
#12579 = CARTESIAN_POINT ( 'NONE',  ( 102.0669872999999797, 122.6166666677591337, -9.794112055954758880E-15 ) ) ;
#12580 = FACE_OUTER_BOUND ( 'NONE', #11087, .T. ) ;
#12581 = DIRECTION ( 'NONE',  ( 0.000000000000000000, -1.000000000000000000, 0.000000000000000000 ) ) ;
#12582 = CARTESIAN_POINT ( 'NONE',  ( 4.859977269581191806, 36.00000000000002132, 12.29462155906313292 ) ) ;
#12583 = CARTESIAN_POINT ( 'NONE',  ( 99.99999999999998579, 94.12499999726881583, -4.999999999999997335 ) ) ;
#12584 = DIRECTION ( 'NONE',  ( -0.000000000000000000, 1.000000000000000000, -0.000000000000000000 ) ) ;
#12585 = VERTEX_POINT ( 'NONE', #10690 ) ;
#12586 = UNCERTAINTY_MEASURE_WITH_UNIT (LENGTH_MEASURE( 1.000000000000000082E-05 ), #16738, 'distance_accuracy_value', 'NONE');
#12587 = EDGE_CURVE ( 'NONE', #8895, #15376, #14822, .T. ) ;
#12588 = CARTESIAN_POINT ( 'NONE',  ( 2.493653234604083739E-15, 40.40468749999999432, 13.57481594606304576 ) ) ;
#12589 = CARTESIAN_POINT ( 'NONE',  ( 13.14518615778179900, 39.41250000108393436, -5.444914386472297529 ) ) ;
#12590 = CLOSED_SHELL ( 'NONE', ( #21509, #4815, #13873, #11621, #27947, #25196, #11759, #18865, #11376, #14861, #4828, #16459, #15246, #18601, #19344, #15768, #15016, #27792, #12957, #21215, #8422, #25684, #28071, #1132, #14362, #27097, #632, #16780, #11978, #15060, #4665, #26009, #23725, #4997, #4912, #17348, #21673, #24684, #1169 ) ) ;
#12591 = CARTESIAN_POINT ( 'NONE',  ( 102.0710678118654329, -4.999999999999989342, 2.437500002731185944 ) ) ;
#12592 = CARTESIAN_POINT ( 'NONE',  ( 143.1451861577818079, 40.40468750108393436, -5.444914386472297529 ) ) ;
#12593 = CARTESIAN_POINT ( 'NONE',  ( 51.85481384221819923, 38.12265625108393152, -5.444914386472297529 ) ) ;
#12594 = CARTESIAN_POINT ( 'NONE',  ( 208.1451861577817795, 40.30546875108393579, 5.444914386472293977 ) ) ;
#12595 = ADVANCED_FACE ( 'NONE', ( #2164 ), #13093, .F. ) ;
#12596 = CARTESIAN_POINT ( 'NONE',  ( 51.90409344636400846, 36.00000000000000000, 1.137167824541468031 ) ) ;
#12597 = CARTESIAN_POINT ( 'NONE',  ( 13.14518615778179900, 37.03125000108393294, -5.444914386472297529 ) ) ;
#12598 = CARTESIAN_POINT ( 'NONE',  ( 193.7288612287583476, 36.00000000000000711, -13.43002483374373135 ) ) ;
#12599 = EDGE_CURVE ( 'NONE', #5426, #18529, #10826, .T. ) ;
#12600 = CARTESIAN_POINT ( 'NONE',  ( 103.5355339059327093, 3.535533905932755072, 9.750000002731184168 ) ) ;
#12601 = CARTESIAN_POINT ( 'NONE',  ( 116.4251840539369596, 40.15664062499999432, -5.622872871577872189 ) ) ;
#12602 = EDGE_CURVE ( 'NONE', #23799, #20591, #8420, .T. ) ;
#12603 = CARTESIAN_POINT ( 'NONE',  ( -9.295050272127046043, 38.86679687608393863, -9.295050272127046043 ) ) ;
#12604 = CARTESIAN_POINT ( 'NONE',  ( 1.501019124304962427, 53.60014735326989666, 15.00000000000000000 ) ) ;
#12605 = CARTESIAN_POINT ( 'NONE',  ( 97.50000000000000000, 124.2500000000000000, 1.035533905932725096 ) ) ;
#12606 = EDGE_CURVE ( 'NONE', #3171, #4458, #25337, .T. ) ;
#12607 = CARTESIAN_POINT ( 'NONE',  ( 101.4615807364564546, 122.6500000010924794, -1.461580736456474794 ) ) ;
#12608 = CARTESIAN_POINT ( 'NONE',  ( 100.8561741729129295, 123.7000000010924765, -2.066987299999998751 ) ) ;
#12609 = CARTESIAN_POINT ( 'NONE',  ( 181.9040934463640156, 36.00000000000000000, 1.137167824541468031 ) ) ;
#12610 = CARTESIAN_POINT ( 'NONE',  ( 98.15313185440925281, -4.458734124999987891, 12.62500000136559208 ) ) ;
#12611 = ORIENTED_EDGE ( 'NONE', *, *, #25541, .F. ) ;
#12612 = CARTESIAN_POINT ( 'NONE',  ( 116.4251840539369596, 40.99999999999999289, 0.000000000000000000 ) ) ;
#12613 = CARTESIAN_POINT ( 'NONE',  ( -8.312177448680279460E-16, 40.00781250000000000, -13.57481594606304576 ) ) ;
#12614 = VECTOR ( 'NONE', #1514, 1000.000000000000000 ) ;
#12615 = CARTESIAN_POINT ( 'NONE',  ( -8.049105076161786076E-16, 31.62382812608393579, -13.14518615778179544 ) ) ;
#12616 = ADVANCED_FACE ( 'NONE', ( #23404 ), #6155, .T. ) ;
#12617 = CARTESIAN_POINT ( 'NONE',  ( 5.622872871577878406, 31.82226562716787654, 13.57481594606304576 ) ) ;
#12618 = CYLINDRICAL_SURFACE ( 'NONE', #1310, 13.57481594606304576 ) ;
#12619 = CARTESIAN_POINT ( 'NONE',  ( 103.1528011352953342, 80.06250000136559208, -3.152801135295383084 ) ) ;
#12620 = CARTESIAN_POINT ( 'NONE',  ( 74.29505027212704249, 39.46210937608393721, 9.295050272127046043 ) ) ;
#12621 = CARTESIAN_POINT ( 'NONE',  ( 99.99999999999998579, 118.4984768113314004, -49.87500000273118417 ) ) ;
#12622 = CARTESIAN_POINT ( 'NONE',  ( 9.295050272127046043, 40.25585937608393294, -9.295050272127046043 ) ) ;
#12623 = VERTEX_POINT ( 'NONE', #6430 ) ;
#12624 = CARTESIAN_POINT ( 'NONE',  ( 99.99999999999998579, 124.1500000010924651, 2.066987299999980099 ) ) ;
#12625 = CARTESIAN_POINT ( 'NONE',  ( 139.5988444088204403, 39.11484374999999858, -9.598844408820458085 ) ) ;
#12626 = CARTESIAN_POINT ( 'NONE',  ( 94.33688103937535629, 105.8855032339526758, -50.29999999453763593 ) ) ;
#12627 = CARTESIAN_POINT ( 'NONE',  ( 116.8548138422182063, 31.97109375108393436, -5.444914386472297529 ) ) ;
#12628 = EDGE_LOOP ( 'NONE', ( #24231, #196 ) ) ;
#12629 = CARTESIAN_POINT ( 'NONE',  ( 99.99999999999995737, 5.000000000000018652, 7.749999999999999112 ) ) ;
#12630 = PLANE ( 'NONE',  #14407 ) ;
#12631 = CARTESIAN_POINT ( 'NONE',  ( 99.99999999999995737, 80.68750000136559208, 4.458734124999988779 ) ) ;
#12632 = CARTESIAN_POINT ( 'NONE',  ( 130.0000000000000000, 39.95820312608393010, 13.14518615778179544 ) ) ;
#12633 = CARTESIAN_POINT ( 'NONE',  ( 74.59884440882045453, 36.03906250216787299, -9.598844408820458085 ) ) ;
#12634 = CARTESIAN_POINT ( 'NONE',  ( 91.91746824999997045, 112.6261737610028320, -53.72499999726881725 ) ) ;
#12635 = CARTESIAN_POINT ( 'NONE',  ( -13.57481594606304576, 35.59257812716788294, 5.622872871577880183 ) ) ;
#12636 = ORIENTED_EDGE ( 'NONE', *, *, #6900, .T. ) ;
#12637 = VECTOR ( 'NONE', #4095, 1000.000000000000000 ) ;
#12638 = CARTESIAN_POINT ( 'NONE',  ( 94.99999999999995737, -2.071067811865466624, 6.062499999999999112 ) ) ;
#12639 = DIRECTION ( 'NONE',  ( 0.000000000000000000, -1.000000000000000000, 0.000000000000000000 ) ) ;
#12640 = EDGE_CURVE ( 'NONE', #26108, #11, #19122, .T. ) ;
#12641 = COLOUR_RGB ( '', 0.09019608, 0.27058824, 0.51372549) ;
#12642 = CARTESIAN_POINT ( 'NONE',  ( 189.5550856135277229, 35.93984375108392726, 13.14518615778179722 ) ) ;
#12643 = CARTESIAN_POINT ( 'NONE',  ( -9.598844408820454532, 38.71796874999999716, 9.598844408820459861 ) ) ;
#12644 = EDGE_CURVE ( 'NONE', #613, #2287, #4298, .T. ) ;
#12645 = CARTESIAN_POINT ( 'NONE',  ( 130.0000000000000000, 39.16445312608392726, 13.14518615778179544 ) ) ;
#12646 = LINE ( 'NONE', #16805, #14140 ) ;
#12647 = LINE ( 'NONE', #13200, #25444 ) ;
#12648 = CARTESIAN_POINT ( 'NONE',  ( 104.9999999999999858, 95.87499999726881583, -6.938893903907228378E-15 ) ) ;
#12649 = DIRECTION ( 'NONE',  ( -0.000000000000000000, 1.000000000000000000, -0.000000000000000000 ) ) ;
#12650 = B_SPLINE_CURVE_WITH_KNOTS ( 'NONE', 3,
 ( #22538, #18543, #14246, #3006, #20688, #737, #15822, #7703, #26677, #5581, #24528, #22968, #12097, #593, #17968, #11678, #25640, #3716, #10522, #16539, #14524, #1301, #12233, #1584, #27385 ),
 .UNSPECIFIED., .F., .F.,
 ( 4, 2, 2, 2, 2, 2, 2, 1, 2, 2, 2, 2, 4 ),
 ( 0.000000000000000000, 0.001301161269048871838, 0.002602322538097743675, 0.005204645076195476075, 0.007806967614293208041, 0.01040929015239094001, 0.01171045142143980686, 0.01301161269048867371, 0.01431277395953754229, 0.01561393522858640914, 0.01821625776668406999, 0.01951741903573289694, 0.02081858030478172389 ),
 .UNSPECIFIED. ) ;
#12651 = CARTESIAN_POINT ( 'NONE',  ( 13.14518615778179900, 38.61875000108393152, -5.444914386472297529 ) ) ;
#12652 = CARTESIAN_POINT ( 'NONE',  ( 185.4011555911795597, 38.71796874999999716, 9.598844408820459861 ) ) ;
#12653 = APPLICATION_PROTOCOL_DEFINITION ( 'draft international standard', 'automotive_design', 1998, #6415 ) ;
#12654 = CARTESIAN_POINT ( 'NONE',  ( 103.5355339059327093, -3.535533905932726206, 8.500000002731185944 ) ) ;
#12655 = CARTESIAN_POINT ( 'NONE',  ( 98.15313185440925281, -4.458734124999987891, 4.875000001365592084 ) ) ;
#12656 = CARTESIAN_POINT ( 'NONE',  ( 51.85481384221820633, 38.96601562608393721, 0.000000000000000000 ) ) ;
#12657 = CARTESIAN_POINT ( 'NONE',  ( 104.4587341249999639, 1.442382525525748735E-14, 7.937500001365592084 ) ) ;
#12658 = PLANE ( 'NONE',  #25046 ) ;
#12659 = CARTESIAN_POINT ( 'NONE',  ( 101.8468681455907330, 93.37499999863439371, 4.458734124999979898 ) ) ;
#12660 = CARTESIAN_POINT ( 'NONE',  ( 116.4251840539369596, 39.36289062499999858, -5.622872871577872189 ) ) ;
#12661 = CARTESIAN_POINT ( 'NONE',  ( -13.57481594606304753, 40.95039062499999005, -5.622872871577873077 ) ) ;
#12662 = CARTESIAN_POINT ( 'NONE',  ( 94.99999999999995737, 1.387778780781445676E-14, 13.99999999999999822 ) ) ;
#12663 = AXIS2_PLACEMENT_3D ( 'NONE', #20998, #26607, #17760 ) ;
#12664 = AXIS2_PLACEMENT_3D ( 'NONE', #22241, #6831, #580 ) ;
#12665 = ORIENTED_EDGE ( 'NONE', *, *, #23597, .F. ) ;
#12666 = CARTESIAN_POINT ( 'NONE',  ( 99.99999999999995737, 83.43750000136560629, -4.458734125000016313 ) ) ;
#12667 = AXIS2_PLACEMENT_3D ( 'NONE', #1126, #21056, #1262 ) ;
#12668 = CARTESIAN_POINT ( 'NONE',  ( -9.598844408820454532, 31.67343750216787512, 9.598844408820459861 ) ) ;
#12669 = ORIENTED_EDGE ( 'NONE', *, *, #21706, .F. ) ;
#12670 = CARTESIAN_POINT ( 'NONE',  ( 102.1631189606246295, 103.3426043859339103, -46.40000000000001279 ) ) ;
#12671 = CARTESIAN_POINT ( 'NONE',  ( 70.44491438647230552, 36.23750000108393721, 13.14518615778179189 ) ) ;
#12672 = ORIENTED_EDGE ( 'NONE', *, *, #16925, .F. ) ;
#12673 = CARTESIAN_POINT ( 'NONE',  ( -5.622872871577873966, 33.01289062716787726, -13.57481594606304753 ) ) ;
#12674 = CARTESIAN_POINT ( 'NONE',  ( 98.15313185440925281, -4.458734124999987891, 4.875000001365592084 ) ) ;
#12675 = ORIENTED_EDGE ( 'NONE', *, *, #25532, .F. ) ;
#12676 = CARTESIAN_POINT ( 'NONE',  ( 97.92893218813452449, 81.93750000273118417, -5.000000000000043521 ) ) ;
#12677 = CARTESIAN_POINT ( 'NONE',  ( 13.14518615778179900, 33.06250000108393294, -5.444914386472297529 ) ) ;
#12678 = CARTESIAN_POINT ( 'NONE',  ( 208.5748159460630120, 36.78320312716786589, -5.622872871577873077 ) ) ;
#12679 = CARTESIAN_POINT ( 'NONE',  ( 2.414731522848535132E-15, 38.37070312608393152, 13.14518615778179544 ) ) ;
#12680 = DIRECTION ( 'NONE',  ( -0.8660254037844407060, 0.4999999999999963363, 0.000000000000000000 ) ) ;
#12681 = CARTESIAN_POINT ( 'NONE',  ( 200.3237909639438215, 54.47170356488064868, 14.99999999999994671 ) ) ;
#12682 = CARTESIAN_POINT ( 'NONE',  ( 130.0000000000000000, 38.96601562608393721, -13.14518615778179544 ) ) ;
#12683 = CARTESIAN_POINT ( 'NONE',  ( -9.295050272127044266, 37.67617187608393436, 9.295050272127047819 ) ) ;
#12684 = ORIENTED_EDGE ( 'NONE', *, *, #14192, .T. ) ;
#12685 = CARTESIAN_POINT ( 'NONE',  ( 78.57481594606305464, 36.63437499999999858, -1.662435489736055892E-15 ) ) ;
#12686 = FACE_OUTER_BOUND ( 'NONE', #15970, .T. ) ;
#12687 = CIRCLE ( 'NONE', #19543, 5.000000000000004441 ) ;
#12688 = CARTESIAN_POINT ( 'NONE',  ( 99.99999999999995737, 4.458734125000016313, 2.187500001365592084 ) ) ;
#12689 = CARTESIAN_POINT ( 'NONE',  ( 2.493653234604083739E-15, 36.43593749999999432, 13.57481594606304576 ) ) ;
#12690 = CARTESIAN_POINT ( 'NONE',  ( 104.4587341249999781, -1.846868145590721655, 4.875000001365592084 ) ) ;
#12691 = CARTESIAN_POINT ( 'NONE',  ( 104.9952793366501851, 116.8754121666685393, -51.82500000273120122 ) ) ;
#12692 = CARTESIAN_POINT ( 'NONE',  ( 99.99999999999995737, -4.458734124999988779, 2.937500001365592528 ) ) ;
#12693 = CARTESIAN_POINT ( 'NONE',  ( 0.000000000000000000, 10.00000000000000178, 16.91709623134523000 ) ) ;
#12694 = CARTESIAN_POINT ( 'NONE',  ( 91.91746824999997045, 112.6261737610028320, -45.72499999726882436 ) ) ;
#12695 = CARTESIAN_POINT ( 'NONE',  ( -13.14518615778179544, 39.95820312608393010, 0.000000000000000000 ) ) ;
#12696 = DIRECTION ( 'NONE',  ( -0.000000000000000000, 1.000000000000000000, -0.000000000000000000 ) ) ;
#12697 = ORIENTED_EDGE ( 'NONE', *, *, #1829, .F. ) ;
#12698 = CARTESIAN_POINT ( 'NONE',  ( 104.9999999999999716, 1.449011120738813565E-14, 1.499999999999999556 ) ) ;
#12699 =( BOUNDED_CURVE ( )  B_SPLINE_CURVE ( 2, ( #16002, #13427, #6891, #15577, #15722, #26719, #18299, #3192, #22155, #22297, #26432, #20157, #638, #2907, #11863, #2633, #4765, #9311, #20586, #20445, #7165, #11576, #20296, #7313, #783, #5337, #9453, #7454, #18153, #13858, #27007, #16148, #14003, #16720, #18583, #21005, #16575, #10012, #12003, #3618, #5899, #18446, #25268, #23143, #3333, #18991, #18721, #10282, #14699, #14146, #1211, #27153, #12139, #20727, #5758, #23418, #22865, #7605, #9877, #3891, #14568, #12278, #27419, #1762, #27560, #23002, #16855, #14286, #27700, #12553, #7882, #27288, #7745, #8163, #25417, #16433, #1485, #14426, #10140, #25131, #18852 ),
 .UNSPECIFIED., .F., .F. ) 
 B_SPLINE_CURVE_WITH_KNOTS ( ( 3, 2, 2, 2, 2, 2, 2, 2, 2, 2, 2, 2, 2, 2, 2, 2, 2, 2, 2, 2, 2, 2, 2, 2, 2, 2, 2, 2, 2, 2, 2, 2, 2, 2, 2, 2, 2, 2, 2, 2, 3 ),
 ( 0.000000000000000000, 0.02500000000000000139, 0.05000000000000000278, 0.07499999999999999722, 0.1000000000000000056, 0.1250000000000000000, 0.1499999999999999944, 0.1749999999999999889, 0.2000000000000000111, 0.2250000000000000056, 0.2500000000000000000, 0.2750000000000000222, 0.2999999999999999889, 0.3250000000000000111, 0.3499999999999999778, 0.3750000000000000000, 0.4000000000000000222, 0.4249999999999999889, 0.4500000000000000111, 0.4749999999999999778, 0.5000000000000000000, 0.5250000000000000222, 0.5500000000000000444, 0.5749999999999999556, 0.5999999999999999778, 0.6250000000000000000, 0.6500000000000000222, 0.6750000000000000444, 0.6999999999999999556, 0.7249999999999999778, 0.7500000000000000000, 0.7750000000000000222, 0.8000000000000000444, 0.8249999999999999556, 0.8499999999999999778, 0.8750000000000000000, 0.9000000000000000222, 0.9250000000000000444, 0.9499999999999999556, 0.9749999999999999778, 1.000000000000000000 ),
 .UNSPECIFIED. ) 
 CURVE ( )  GEOMETRIC_REPRESENTATION_ITEM ( )  RATIONAL_B_SPLINE_CURVE ( ( 1.000000000000000000, 0.9238795325112867385, 1.000000000000000000, 0.9238795325112867385, 1.000000000000000000, 0.9238795325112867385, 1.000000000000000000, 0.9238795325112867385, 1.000000000000000000, 0.9238795325112867385, 1.000000000000000000, 0.9238795325112867385, 1.000000000000000000, 0.9238795325112867385, 1.000000000000000000, 0.9238795325112867385, 1.000000000000000000, 0.9238795325112867385, 1.000000000000000000, 0.9238795325112867385, 1.000000000000000000, 0.9238795325112867385, 1.000000000000000000, 0.9238795325112867385, 1.000000000000000000, 0.9238795325112867385, 1.000000000000000000, 0.9238795325112867385, 1.000000000000000000, 0.9238795325112867385, 1.000000000000000000, 0.9238795325112867385, 1.000000000000000000, 0.9238795325112867385, 1.000000000000000000, 0.9238795325112867385, 1.000000000000000000, 0.9238795325112867385, 1.000000000000000000, 0.9238795325112867385, 1.000000000000000000, 0.9238795325112867385, 1.000000000000000000, 0.9238795325112867385, 1.000000000000000000, 0.9238795325112867385, 1.000000000000000000, 0.9238795325112867385, 1.000000000000000000, 0.9238795325112867385, 1.000000000000000000, 0.9238795325112867385, 1.000000000000000000, 0.9238795325112867385, 1.000000000000000000, 0.9238795325112867385, 1.000000000000000000, 0.9238795325112867385, 1.000000000000000000, 0.9238795325112867385, 1.000000000000000000, 0.9238795325112867385, 1.000000000000000000, 0.9238795325112867385, 1.000000000000000000, 0.9238795325112867385, 1.000000000000000000, 0.9238795325112867385, 1.000000000000000000, 0.9238795325112867385, 1.000000000000000000, 0.9238795325112867385, 1.000000000000000000, 0.9238795325112867385, 1.000000000000000000, 0.9238795325112867385, 1.000000000000000000, 0.9238795325112867385, 1.000000000000000000, 0.9238795325112867385, 1.000000000000000000 ) ) 
 REPRESENTATION_ITEM ( '' )  );
#12700 = CARTESIAN_POINT ( 'NONE',  ( 94.99999999999995737, 1.387778780781445676E-14, 5.999999999999998224 ) ) ;
#12701 = CARTESIAN_POINT ( 'NONE',  ( 99.99999999999995737, 83.37500000273119838, 4.999999999999990230 ) ) ;
#12702 = CARTESIAN_POINT ( 'NONE',  ( -5.622872871577890841, 40.35507812499999147, 13.57481594606302444 ) ) ;
#12703 = CARTESIAN_POINT ( 'NONE',  ( 195.0000000000000000, 39.56132812608393579, -13.14518615778179544 ) ) ;
#12704 = ORIENTED_EDGE ( 'NONE', *, *, #3565, .T. ) ;
#12705 = CARTESIAN_POINT ( 'NONE',  ( 59.55508561352770158, 39.01562500108394005, -13.14518615778179722 ) ) ;
#12706 = AXIS2_PLACEMENT_3D ( 'NONE', #5268, #15800, #22661 ) ;
#12707 = DIRECTION ( 'NONE',  ( 0.000000000000000000, 0.000000000000000000, 1.000000000000000000 ) ) ;
#12708 = DIRECTION ( 'NONE',  ( -0.000000000000000000, -0.000000000000000000, -1.000000000000000000 ) ) ;
#12709 = ORIENTED_EDGE ( 'NONE', *, *, #5162, .T. ) ;
#12710 = CARTESIAN_POINT ( 'NONE',  ( 107.0000000000000142, 112.2744378736303332, -50.90000000000001279 ) ) ;
#12711 = CARTESIAN_POINT ( 'NONE',  ( -1.814355354584118674, 51.46618445021835697, -14.99999999999999467 ) ) ;
#12712 = CARTESIAN_POINT ( 'NONE',  ( 97.92893218813455292, 80.93750000273118417, -5.000000000000053291 ) ) ;
#12713 = CIRCLE ( 'NONE', #20025, 15.57481594606304576 ) ;
#12714 = CARTESIAN_POINT ( 'NONE',  ( 143.5748159460630404, 35.19570312716788152, -5.622872871577873077 ) ) ;
#12715 = CARTESIAN_POINT ( 'NONE',  ( 105.6631189606246295, 105.8855032339526758, -43.70000000546238539 ) ) ;
#12716 = CARTESIAN_POINT ( 'NONE',  ( 181.8548138422181921, 35.14609375108393152, -5.444914386472297529 ) ) ;
#12717 = ORIENTED_EDGE ( 'NONE', *, *, #15545, .F. ) ;
#12718 = ORIENTED_EDGE ( 'NONE', *, *, #3440, .T. ) ;
#12719 = CARTESIAN_POINT ( 'NONE',  ( 13.14518615778179900, 40.30546875108393579, 5.444914386472293977 ) ) ;
#12720 = CARTESIAN_POINT ( 'NONE',  ( 98.15313185440923860, 4.458734125000016313, 14.50000000136559208 ) ) ;
#12721 = CARTESIAN_POINT ( 'NONE',  ( 55.70494972787295751, 39.85898437608393152, 9.295050272127047819 ) ) ;
#12722 = CARTESIAN_POINT ( 'NONE',  ( 99.99999999999995737, 80.68750000136559208, 4.458734124999988779 ) ) ;
#12723 = DIRECTION ( 'NONE',  ( -0.000000000000000000, 1.000000000000000000, -0.000000000000000000 ) ) ;
#12724 = VECTOR ( 'NONE', #564, 1000.000000000000000 ) ;
#12725 = CARTESIAN_POINT ( 'NONE',  ( 5.444914386472297529, 40.50390625108394005, -13.14518615778179722 ) ) ;
#12726 = EDGE_CURVE ( 'NONE', #7831, #11228, #20766, .T. ) ;
#12727 = DIRECTION ( 'NONE',  ( -0.000000000000000000, 1.000000000000000000, -0.000000000000000000 ) ) ;
#12728 = CARTESIAN_POINT ( 'NONE',  ( -5.622872871577965448, 37.97382812499999716, 13.57481594606295161 ) ) ;
#12729 = CARTESIAN_POINT ( 'NONE',  ( 181.8548138422182205, 39.95820312608393010, 0.000000000000000000 ) ) ;
#12730 = CARTESIAN_POINT ( 'NONE',  ( 91.91746824999998466, 110.0000000000000000, -47.62499999726882294 ) ) ;
#12731 = ORIENTED_EDGE ( 'NONE', *, *, #22243, .F. ) ;
#12732 = CARTESIAN_POINT ( 'NONE',  ( 13.57481594606304753, 40.65273437499998721, -5.622872871577873077 ) ) ;
#12733 = CARTESIAN_POINT ( 'NONE',  ( 13.14518615778179900, 40.10703125108393152, 5.444914386472293977 ) ) ;
#12734 = CARTESIAN_POINT ( 'NONE',  ( 96.46446609406721961, -3.535533905932727539, 1.250000002731184390 ) ) ;
#12735 = CARTESIAN_POINT ( 'NONE',  ( 143.1451861577818079, 36.33671875108394289, 5.444914386472293977 ) ) ;
#12736 = CARTESIAN_POINT ( 'NONE',  ( 59.55508561352770158, 36.73359375108393010, 13.14518615778179722 ) ) ;
#12737 = CARTESIAN_POINT ( 'NONE',  ( 195.0000000000000000, 40.55351562608393579, -13.14518615778179544 ) ) ;
#12738 =( BOUNDED_CURVE ( )  B_SPLINE_CURVE ( 2, ( #9572, #26983, #1187, #27399, #9854, #27948, #1735, #28088, #2007 ),
 .UNSPECIFIED., .F., .T. ) 
 B_SPLINE_CURVE_WITH_KNOTS ( ( 3, 2, 2, 2, 3 ),
 ( 0.3958333333333331483, 0.4062499999999999445, 0.4166666666666667407, 0.4270833333333335369, 0.4375000000000003331 ),
 .UNSPECIFIED. ) 
 CURVE ( )  GEOMETRIC_REPRESENTATION_ITEM ( )  RATIONAL_B_SPLINE_CURVE ( ( 1.000000000000001110, 0.9238795325112855172, 1.000000000000000000, 0.9238795325112867385, 1.000000000000000000, 0.9238795325112867385, 1.000000000000000000, 0.9238795325112842960, 1.000000000000002442 ) ) 
 REPRESENTATION_ITEM ( '' )  );
#12739 = CARTESIAN_POINT ( 'NONE',  ( 95.27063293749995410, 1.387778780781445676E-14, 14.84375000068279604 ) ) ;
#12740 = CARTESIAN_POINT ( 'NONE',  ( -13.14518615778179544, 35.79101562608393294, 0.000000000000000000 ) ) ;
#12741 = CARTESIAN_POINT ( 'NONE',  ( 127.7238531554433791, 51.46995505939418791, -15.00000000000033751 ) ) ;
#12742 = CARTESIAN_POINT ( 'NONE',  ( 97.92893218813451028, 5.000000000000018652, 9.937500002731184168 ) ) ;
#12743 = FACE_OUTER_BOUND ( 'NONE', #6299, .T. ) ;
#12744 = VECTOR ( 'NONE', #19397, 1000.000000000000000 ) ;
#12745 = CARTESIAN_POINT ( 'NONE',  ( 13.14518615778179900, 37.72578125108393721, 5.444914386472293977 ) ) ;
#12746 = DIRECTION ( 'NONE',  ( -0.000000000000000000, -0.000000000000000000, -1.000000000000000000 ) ) ;
#12747 = CARTESIAN_POINT ( 'NONE',  ( 98.96446609406727646, 123.3500000021849701, -2.499999999999997780 ) ) ;
#12748 = CARTESIAN_POINT ( 'NONE',  ( 99.99999999999998579, 124.0000000000000000, -2.499999999999997780 ) ) ;
#12749 = EDGE_CURVE ( 'NONE', #25694, #4172, #24620, .T. ) ;
#12750 = CARTESIAN_POINT ( 'NONE',  ( -13.57481594606304398, 37.08085937499999574, 5.622872871577880183 ) ) ;
#12751 = CARTESIAN_POINT ( 'NONE',  ( 96.84719886470459471, 3.152801135295383084, 8.312500001365592084 ) ) ;
#12752 = CARTESIAN_POINT ( 'NONE',  ( 97.83688103937537051, 103.3426043859339103, -48.10000000546237686 ) ) ;
#12753 = ORIENTED_EDGE ( 'NONE', *, *, #18211, .F. ) ;
#12754 = CARTESIAN_POINT ( 'NONE',  ( 97.50000000000000000, 123.5000000021849615, -9.540979117872439019E-15 ) ) ;
#12755 = CARTESIAN_POINT ( 'NONE',  ( 96.84719886470459471, 3.152801135295383084, 10.31250000136559208 ) ) ;
#12756 = CARTESIAN_POINT ( 'NONE',  ( -8.049105076161786076E-16, 34.00507812608393721, -13.14518615778179544 ) ) ;
#12757 = CARTESIAN_POINT ( 'NONE',  ( -13.14518615778179544, 40.55351562608393579, 0.000000000000000000 ) ) ;
#12758 = CARTESIAN_POINT ( 'NONE',  ( 92.99999999999995737, 1.387778780781445676E-14, 15.00000000000000000 ) ) ;
#12759 = CARTESIAN_POINT ( 'NONE',  ( 104.4587341249999639, 81.93750000136559208, -1.442382525525748735E-14 ) ) ;
#12760 = CARTESIAN_POINT ( 'NONE',  ( 78.14518615778179367, 37.92421875108392726, 5.444914386472293977 ) ) ;
#12761 = CARTESIAN_POINT ( 'NONE',  ( 99.99999999999998579, 101.5015231886685854, -44.87500000273119838 ) ) ;
#12762 = CARTESIAN_POINT ( 'NONE',  ( 9.295050272127047819, 40.05742187608392868, 9.295050272127046043 ) ) ;
#12763 = APPLICATION_CONTEXT ( 'automotive_design' ) ;
#12764 = ADVANCED_FACE ( 'NONE', ( #9556 ), #13535, .F. ) ;
#12765 = CARTESIAN_POINT ( 'NONE',  ( 102.0669872999999939, 124.4000000010924651, -0.8561741729129507261 ) ) ;
#12766 = CARTESIAN_POINT ( 'NONE',  ( 5.622872871577870413, 33.60820312499999574, -13.57481594606304753 ) ) ;
#12767 = CARTESIAN_POINT ( 'NONE',  ( 99.99999999999997158, 117.3602355696678501, -48.99999999453763877 ) ) ;
#12768 = CARTESIAN_POINT ( 'NONE',  ( 130.0000000000000000, 39.61093749999999147, 13.57481594606304576 ) ) ;
#12769 = EDGE_LOOP ( 'NONE', ( #9336, #16301, #20834, #26587 ) ) ;
#12770 = DIRECTION ( 'NONE',  ( 0.000000000000000000, 0.000000000000000000, 1.000000000000000000 ) ) ;
#12771 = ADVANCED_FACE ( 'NONE', ( #2448 ), #24382, .T. ) ;
#12772 = CARTESIAN_POINT ( 'NONE',  ( -13.14518615778179189, 39.21406250108392300, 5.444914386472304635 ) ) ;
#12773 = CARTESIAN_POINT ( 'NONE',  ( 103.1528011352953342, 80.06250000136559208, -3.152801135295383084 ) ) ;
#12774 = ADVANCED_FACE ( 'NONE', ( #9408 ), #3004, .T. ) ;
#12775 = CARTESIAN_POINT ( 'NONE',  ( 139.2950502721270425, 37.87460937608393152, -9.295050272127046043 ) ) ;
#12776 = CARTESIAN_POINT ( 'NONE',  ( 70.62287287157786864, 36.08867187716787583, -13.57481594606304753 ) ) ;
#12777 = CARTESIAN_POINT ( 'NONE',  ( 108.0825317499999869, 107.3738262389971538, -52.72499999726881015 ) ) ;
#12778 = CARTESIAN_POINT ( 'NONE',  ( -9.598844408820454532, 36.43593750216787441, 9.598844408820459861 ) ) ;
#12779 = CARTESIAN_POINT ( 'NONE',  ( 104.9999999999999716, 1.449011120738813565E-14, 3.499999999999999556 ) ) ;
#12780 = EDGE_CURVE ( 'NONE', #20388, #21081, #21503, .T. ) ;
#12781 = CARTESIAN_POINT ( 'NONE',  ( 105.6631189606246295, 114.1144967660473242, -52.80000000000000426 ) ) ;
#12782 = CARTESIAN_POINT ( 'NONE',  ( 204.2950502721270425, 38.46992187608393010, 9.295050272127046043 ) ) ;
#12783 = CARTESIAN_POINT ( 'NONE',  ( 65.00000000000000000, 39.21406249999999716, -13.57481594606304576 ) ) ;
#12784 = CARTESIAN_POINT ( 'NONE',  ( 116.8548138422182205, 38.96601562608393721, 0.000000000000000000 ) ) ;
#12785 = CARTESIAN_POINT ( 'NONE',  ( 102.4999999999999858, 122.3000000021849587, -9.847140817659276890E-15 ) ) ;
#12786 = CYLINDRICAL_SURFACE ( 'NONE', #6315, 13.57481594606304398 ) ;
#12787 = CARTESIAN_POINT ( 'NONE',  ( 103.1528011352953484, 95.18749999863440792, 3.152801135295352886 ) ) ;
#12788 = CARTESIAN_POINT ( 'NONE',  ( 94.33688103937535629, 105.8855032339526758, -48.80000000000001137 ) ) ;
#12789 = CARTESIAN_POINT ( 'NONE',  ( -5.444914386472297529, 37.42812500108394147, -13.14518615778179900 ) ) ;
#12790 = CARTESIAN_POINT ( 'NONE',  ( -8.049105076161786076E-16, 38.76757812608393294, -13.14518615778179544 ) ) ;
#12791 = CARTESIAN_POINT ( 'NONE',  ( 185.4011555911795313, 36.93203124999999432, -9.598844408820458085 ) ) ;
#12792 = EDGE_CURVE ( 'NONE', #25689, #14731, #17776, .T. ) ;
#12793 = CARTESIAN_POINT ( 'NONE',  ( 93.46109445667491400, 105.2492070361643215, -47.17500000273119554 ) ) ;
#12794 = CARTESIAN_POINT ( 'NONE',  ( 101.8468681455906903, 4.458734125000016313, 2.375000001365592084 ) ) ;
#12795 = CARTESIAN_POINT ( 'NONE',  ( 55.70494972787295751, 37.47773437608393010, 9.295050272127047819 ) ) ;
#12796 = CARTESIAN_POINT ( 'NONE',  ( 95.54126587499996504, -1.846868145590724986, 7.500000001365592084 ) ) ;
#12797 = CARTESIAN_POINT ( 'NONE',  ( 104.4587341249999923, 95.24999999863437949, 1.846868145590726318 ) ) ;
#12798 = CARTESIAN_POINT ( 'NONE',  ( -13.57481594606304576, 40.25585937499999289, 5.622872871577880183 ) ) ;
#12799 = CARTESIAN_POINT ( 'NONE',  ( 143.1451861577818079, 40.30546875108393579, 5.444914386472293977 ) ) ;
#12800 = ORIENTED_EDGE ( 'NONE', *, *, #19932, .F. ) ;
#12801 = CARTESIAN_POINT ( 'NONE',  ( 99.99999999999995737, 84.25000000000000000, 4.999999999999990230 ) ) ;
#12802 = DIRECTION ( 'NONE',  ( 0.000000000000000000, 0.000000000000000000, 1.000000000000000000 ) ) ;
#12803 = ORIENTED_EDGE ( 'NONE', *, *, #11558, .F. ) ;
#12804 = ADVANCED_FACE ( 'NONE', ( #20249 ), #11396, .F. ) ;
#12805 = DIRECTION ( 'NONE',  ( 0.000000000000000000, 1.000000000000000000, 0.000000000000000000 ) ) ;
#12806 = CARTESIAN_POINT ( 'NONE',  ( 55.70494972787295751, 33.70742187608393436, 9.295050272127047819 ) ) ;
#12807 = ORIENTED_EDGE ( 'NONE', *, *, #25863, .T. ) ;
#12808 = CARTESIAN_POINT ( 'NONE',  ( 128.4989808756949969, 53.60014735326987534, -14.99999999999999822 ) ) ;
#12809 = CARTESIAN_POINT ( 'NONE',  ( 98.15313185440925281, 4.458734125000016313, 1.500000001365592972 ) ) ;
#12810 = VERTEX_POINT ( 'NONE', #7124 ) ;
#12811 = CARTESIAN_POINT ( 'NONE',  ( -8.049105076161786076E-16, 34.99726562608393721, -13.14518615778179544 ) ) ;
#12812 = CARTESIAN_POINT ( 'NONE',  ( -13.14518615778179544, 31.82226562608393650, 0.000000000000000000 ) ) ;
#12813 = CARTESIAN_POINT ( 'NONE',  ( 208.5748159460630120, 37.47773437716787726, 5.622872871577869525 ) ) ;
#12814 = CARTESIAN_POINT ( 'NONE',  ( -5.444914386472299306, 36.73359375108393010, 13.14518615778179722 ) ) ;
#12815 = PRODUCT ( 'connector', 'connector', '', ( #19857 ) ) ;
#12816 = DIRECTION ( 'NONE',  ( -0.000000000000000000, -0.000000000000000000, 1.000000000000000000 ) ) ;
#12817 = CARTESIAN_POINT ( 'NONE',  ( 97.83688103937537051, 103.3426043859339103, -51.60000000000000853 ) ) ;
#12818 = CARTESIAN_POINT ( 'NONE',  ( 124.5550856135277087, 40.10703125108393152, 13.14518615778179722 ) ) ;
#12819 = CARTESIAN_POINT ( 'NONE',  ( 13.14518615778179544, 38.76757812608393294, -1.609821015232357215E-15 ) ) ;
#12820 = CARTESIAN_POINT ( 'NONE',  ( 143.1451861577818079, 34.65000000108393152, -5.444914386472297529 ) ) ;
#12821 = CARTESIAN_POINT ( 'NONE',  ( 78.57481594606304043, 36.58476562499999574, 5.622872871577869525 ) ) ;
#12822 = CARTESIAN_POINT ( 'NONE',  ( 102.0710678118654329, 5.000000000000018652, 9.687499999999998224 ) ) ;
#12823 = CARTESIAN_POINT ( 'NONE',  ( 98.15313185440925281, 4.458734125000016313, 14.50000000136559208 ) ) ;
#12824 = DIRECTION ( 'NONE',  ( 5.782411586589357392E-17, -0.000000000000000000, 1.000000000000000000 ) ) ;
#12825 = CARTESIAN_POINT ( 'NONE',  ( 101.8468681455906903, 4.458734125000016313, 4.125000001365592084 ) ) ;
#12826 = CARTESIAN_POINT ( 'NONE',  ( 97.50236033167492167, 117.6869444889999841, -53.52500000273118985 ) ) ;
#12827 = DIRECTION ( 'NONE',  ( -0.000000000000000000, -1.000000000000000000, -0.000000000000000000 ) ) ;
#12828 = CARTESIAN_POINT ( 'NONE',  ( 214.9999999999999716, 55.00000000000000000, -10.00000000000000000 ) ) ;
#12829 = CARTESIAN_POINT ( 'NONE',  ( -9.295050272127046043, 32.51679687608393721, -9.295050272127046043 ) ) ;
#12830 = CARTESIAN_POINT ( 'NONE',  ( 102.0710678118654329, 5.000000000000018652, 7.812500002731185056 ) ) ;
#12831 = AXIS2_PLACEMENT_3D ( 'NONE', #27307, #12019, #11736 ) ;
#12832 = CARTESIAN_POINT ( 'NONE',  ( 108.0825317499999869, 107.3738262389971538, -48.97499999726881015 ) ) ;
#12833 = VERTEX_POINT ( 'NONE', #13239 ) ;
#12834 = CARTESIAN_POINT ( 'NONE',  ( 5.444914386472302859, 32.26875000108393721, 13.14518615778179189 ) ) ;
#12835 = CARTESIAN_POINT ( 'NONE',  ( -13.14518615778179544, 40.55351562608393579, 0.000000000000000000 ) ) ;
#12836 = CARTESIAN_POINT ( 'NONE',  ( 101.7677669209684552, 123.0000000000000000, 1.767766984964258992 ) ) ;
#12837 = CARTESIAN_POINT ( 'NONE',  ( 99.92084351319844870, 123.0000000000000142, -2.153125375274123510 ) ) ;
#12838 = CARTESIAN_POINT ( 'NONE',  ( 204.2950502721270425, 38.66835937608393436, -9.295050272127046043 ) ) ;
#12839 = VERTEX_POINT ( 'NONE', #15958 ) ;
#12840 = CYLINDRICAL_SURFACE ( 'NONE', #145, 11.57481594606304398 ) ;
#12841 = CARTESIAN_POINT ( 'NONE',  ( 94.33688103937535629, 105.8855032339526758, -54.80000000000001847 ) ) ;
#12842 = CARTESIAN_POINT ( 'NONE',  ( 64.28023940389081758, 53.51499872091923038, -15.00000000000000000 ) ) ;
#12843 = VERTEX_POINT ( 'NONE', #15821 ) ;
#12844 = CARTESIAN_POINT ( 'NONE',  ( 107.0000000000000142, 110.0000000000000000, -51.00000000000000711 ) ) ;
#12845 = CARTESIAN_POINT ( 'NONE',  ( 99.14382582708707048, 123.3000000010924708, 2.066987299999979211 ) ) ;
#12846 = CARTESIAN_POINT ( 'NONE',  ( 130.0000000000000000, 33.75703125216787726, -13.57481594606304576 ) ) ;
#12847 =( BOUNDED_CURVE ( )  B_SPLINE_CURVE ( 2, ( #16357, #14206, #22927, #1548, #23203, #8215, #14486, #10623, #3678, #3953, #4226 ),
 .UNSPECIFIED., .F., .T. ) 
 B_SPLINE_CURVE_WITH_KNOTS ( ( 3, 2, 2, 2, 2, 3 ),
 ( 0.3000000000000002109, 0.3200000000000001177, 0.3400000000000000244, 0.3599999999999998757, 0.3799999999999997824, 0.3999999999999996891 ),
 .UNSPECIFIED. ) 
 CURVE ( )  GEOMETRIC_REPRESENTATION_ITEM ( )  RATIONAL_B_SPLINE_CURVE ( ( 0.9999999999999994449, 0.9510565162951540863, 1.000000000000000000, 0.9510565162951535312, 1.000000000000000000, 0.9510565162951535312, 1.000000000000000000, 0.9510565162951535312, 1.000000000000000000, 0.9510565162951543083, 0.9999999999999992228 ) ) 
 REPRESENTATION_ITEM ( '' )  );
#12848 = CARTESIAN_POINT ( 'NONE',  ( 78.14518615778179367, 40.35507812608393863, -1.609821015232357215E-15 ) ) ;
#12849 = CARTESIAN_POINT ( 'NONE',  ( -8.312177448680279460E-16, 31.37578125216787583, -13.57481594606304576 ) ) ;
#12850 = CARTESIAN_POINT ( 'NONE',  ( 195.0000000000000000, 34.20351562608394147, -13.14518615778179544 ) ) ;
#12851 = ORIENTED_EDGE ( 'NONE', *, *, #21718, .T. ) ;
#12852 = ORIENTED_EDGE ( 'NONE', *, *, #21874, .F. ) ;
#12853 = CARTESIAN_POINT ( 'NONE',  ( -5.444914386472297529, 40.60312500108393863, -13.14518615778179900 ) ) ;
#12854 = CARTESIAN_POINT ( 'NONE',  ( 95.54126587499996504, 1.387778780781445676E-14, 11.68750000136559208 ) ) ;
#12855 = CARTESIAN_POINT ( 'NONE',  ( 102.4999999999999858, 124.5500000000000256, 1.035533905932722876 ) ) ;
#12856 = CARTESIAN_POINT ( 'NONE',  ( 104.4587341249999639, 80.93750000136559208, -1.442382525525748735E-14 ) ) ;
#12857 = CARTESIAN_POINT ( 'NONE',  ( 185.7049497278729575, 39.85898437608393152, 9.295050272127047819 ) ) ;
#12858 = CARTESIAN_POINT ( 'NONE',  ( 135.6228728715778971, 39.75976562716787299, 13.57481594606306174 ) ) ;
#12859 = FACE_OUTER_BOUND ( 'NONE', #15041, .T. ) ;
#12860 = CARTESIAN_POINT ( 'NONE',  ( 214.9999999999999716, 55.00000000000000000, -10.00000000000000000 ) ) ;
#12861 = DIRECTION ( 'NONE',  ( 5.782411586589357392E-17, -0.000000000000000000, 1.000000000000000000 ) ) ;
#12862 = CARTESIAN_POINT ( 'NONE',  ( 95.00472066334982912, 103.1245878333314323, -47.32499999726881157 ) ) ;
#12863 = ORIENTED_EDGE ( 'NONE', *, *, #2573, .F. ) ;
#12864 = CARTESIAN_POINT ( 'NONE',  ( 13.57481594606304931, 35.79101562499999289, 5.622872871577869525 ) ) ;
#12865 = CARTESIAN_POINT ( 'NONE',  ( 5.444914386472297529, 38.71796875108393721, -13.14518615778179900 ) ) ;
#12866 = CARTESIAN_POINT ( 'NONE',  ( 104.9999999999999574, -2.071067811865462627, 2.562500002731185500 ) ) ;
#12867 = CARTESIAN_POINT ( 'NONE',  ( 124.5550856135277087, 35.04687500108393294, -13.14518615778179900 ) ) ;
#12868 = CARTESIAN_POINT ( 'NONE',  ( 51.85481384221820633, 34.20351562608393436, 0.000000000000000000 ) ) ;
#12869 = CARTESIAN_POINT ( 'NONE',  ( 181.8548138422181921, 37.62656250108393863, 5.444914386472304635 ) ) ;
#12870 = CARTESIAN_POINT ( 'NONE',  ( 95.67376207875072680, 104.0454443415356991, -46.20000000546237118 ) ) ;
#12871 = CARTESIAN_POINT ( 'NONE',  ( 13.14518615778179900, 36.93203125108394147, 5.444914386472293977 ) ) ;
#12872 = CARTESIAN_POINT ( 'NONE',  ( 138.7726092461284679, 50.37415326812335792, -15.00000000000000000 ) ) ;
#12873 = CARTESIAN_POINT ( 'NONE',  ( -13.57481594606304576, 38.71796875216787726, 0.000000000000000000 ) ) ;
#12874 = CARTESIAN_POINT ( 'NONE',  ( 9.295050272127046043, 33.31054687608394005, -9.295050272127046043 ) ) ;
#12875 = CARTESIAN_POINT ( 'NONE',  ( 99.99999999999998579, 95.00000000000000000, -6.938893903907228378E-15 ) ) ;
#12876 = EDGE_CURVE ( 'NONE', #6997, #17432, #26422, .T. ) ;
#12877 = CARTESIAN_POINT ( 'NONE',  ( -9.295050272127046043, 38.07304687608393579, -9.295050272127046043 ) ) ;
#12878 = CARTESIAN_POINT ( 'NONE',  ( 5.317351577475893265, 54.47013368152371982, 15.00000000000000533 ) ) ;
#12879 = CARTESIAN_POINT ( 'NONE',  ( 97.50000000000000000, 124.2500000021849758, -1.035533905932742416 ) ) ;
#12880 = CARTESIAN_POINT ( 'NONE',  ( -13.57481594606304576, 36.33671875216787583, 0.000000000000000000 ) ) ;
#12881 = VECTOR ( 'NONE', #3530, 1000.000000000000000 ) ;
#12882 = CARTESIAN_POINT ( 'NONE',  ( 103.1528011352953342, -3.152801135295355106, 8.812500001365592084 ) ) ;
#12883 = CARTESIAN_POINT ( 'NONE',  ( 101.7677669209684552, 123.0000000000000000, 1.767766984964258992 ) ) ;
#12884 = EDGE_LOOP ( 'NONE', ( #15453, #4330, #6761, #276, #20225, #25135, #2004, #7442, #18963, #17698, #10844, #1952, #19769, #12978, #12675 ) ) ;
#12885 = DIRECTION ( 'NONE',  ( 0.000000000000000000, 1.000000000000000000, -0.000000000000000000 ) ) ;
#12886 = CARTESIAN_POINT ( 'NONE',  ( 101.8468681455906903, 4.458734125000016313, 10.12500000136559208 ) ) ;
#12887 = CARTESIAN_POINT ( 'NONE',  ( 122.3637589320068884, 54.91786508990715276, 14.99999999999996625 ) ) ;
#12888 = CARTESIAN_POINT ( 'NONE',  ( 13.14518615778179544, 39.36289062608393152, -1.609821015232357215E-15 ) ) ;
#12889 = LINE ( 'NONE', #26169, #26315 ) ;
#12890 = CARTESIAN_POINT ( 'NONE',  ( 103.1528011352953342, 81.06250000136559208, 3.152801135295355106 ) ) ;
#12891 = CARTESIAN_POINT ( 'NONE',  ( 51.85481384221820633, 34.45156250108394147, 5.444914386472304635 ) ) ;
#12892 = CARTESIAN_POINT ( 'NONE',  ( 108.0825317500000011, 112.6261737610028320, -54.02500000273118275 ) ) ;
#12893 = CARTESIAN_POINT ( 'NONE',  ( 5.444914386472297529, 39.51171875108393294, -13.14518615778179722 ) ) ;
#12894 = ORIENTED_EDGE ( 'NONE', *, *, #11311, .T. ) ;
#12895 = CARTESIAN_POINT ( 'NONE',  ( -13.57481594606304576, 39.41249999999999432, 0.000000000000000000 ) ) ;
#12896 = DIRECTION ( 'NONE',  ( 5.782411586589358625E-17, -0.000000000000000000, 1.000000000000000000 ) ) ;
#12897 = CARTESIAN_POINT ( 'NONE',  ( 107.0000000000000000, 112.2744378736303332, -55.39999999453763735 ) ) ;
#12898 = CARTESIAN_POINT ( 'NONE',  ( 116.8548138422182063, 32.07031250108393294, 5.444914386472304635 ) ) ;
#12899 = EDGE_LOOP ( 'NONE', ( #24726, #18322, #14360, #27684 ) ) ;
#12900 = CARTESIAN_POINT ( 'NONE',  ( 92.99999999999998579, 110.0000000000000000, -56.49999999453763877 ) ) ;
#12901 =( BOUNDED_CURVE ( )  B_SPLINE_CURVE ( 2, ( #17286, #17143, #21999, #10859, #2475, #6734, #25844, #23712, #19151 ),
 .UNSPECIFIED., .F., .F. ) 
 B_SPLINE_CURVE_WITH_KNOTS ( ( 3, 2, 2, 2, 3 ),
 ( 0.3541666666666666852, 0.3645833333333332593, 0.3749999999999998890, 0.3854166666666665741, 0.3958333333333331483 ),
 .UNSPECIFIED. ) 
 CURVE ( )  GEOMETRIC_REPRESENTATION_ITEM ( )  RATIONAL_B_SPLINE_CURVE ( ( 1.000000000000000000, 0.9238795325112867385, 1.000000000000000000, 0.9238795325112867385, 1.000000000000000000, 0.9238795325112867385, 1.000000000000000000, 0.9238795325112879597, 0.9999999999999987788 ) ) 
 REPRESENTATION_ITEM ( '' )  );
#12902 = CARTESIAN_POINT ( 'NONE',  ( 13.14518615778179900, 36.43593750108392726, -5.444914386472297529 ) ) ;
#12903 = CARTESIAN_POINT ( 'NONE',  ( -13.57481594606304576, 36.33671875216787583, 0.000000000000000000 ) ) ;
#12904 = CARTESIAN_POINT ( 'NONE',  ( 135.4449143864723055, 35.24531250108393010, 13.14518615778179189 ) ) ;
#12905 = CARTESIAN_POINT ( 'NONE',  ( 51.42518405393695957, 37.92421875216787441, 0.000000000000000000 ) ) ;
#12906 = CARTESIAN_POINT ( 'NONE',  ( 2.232327155338130975, 36.00000000000002132, 12.98409812936875696 ) ) ;
#12907 = CARTESIAN_POINT ( 'NONE',  ( 5.622872871577871301, 36.08867187716787583, -13.57481594606304753 ) ) ;
#12908 = CARTESIAN_POINT ( 'NONE',  ( 104.9999999999999716, 1.449011120738813565E-14, 4.499999999999999112 ) ) ;
#12909 = CARTESIAN_POINT ( 'NONE',  ( 112.9999999999999858, 118.0000000000000000, -13.00000000000000888 ) ) ;
#12910 = VECTOR ( 'NONE', #22126, 1000.000000000000000 ) ;
#12911 = CARTESIAN_POINT ( 'NONE',  ( 204.2950502721270425, 37.87460937608393152, -9.295050272127046043 ) ) ;
#12912 = CARTESIAN_POINT ( 'NONE',  ( -13.57481594606304576, 33.95546875216787441, 0.000000000000000000 ) ) ;
#12913 = CARTESIAN_POINT ( 'NONE',  ( 103.5355339059327235, 92.87500000000000000, 3.535533905932724874 ) ) ;
#12914 = CARTESIAN_POINT ( 'NONE',  ( 94.99999999999998579, 110.0000000000000000, -145.0000000000000284 ) ) ;
#12915 = ADVANCED_FACE ( 'NONE', ( #22393 ), #13828, .T. ) ;
#12916 = DIRECTION ( 'NONE',  ( 0.000000000000000000, 0.000000000000000000, 1.000000000000000000 ) ) ;
#12917 = CARTESIAN_POINT ( 'NONE',  ( -9.598844408820454532, 32.46718750216787441, 9.598844408820459861 ) ) ;
#12918 = CARTESIAN_POINT ( 'NONE',  ( -9.598844408820458085, 38.51953124999999289, -9.598844408820458085 ) ) ;
#12919 = LINE ( 'NONE', #10234, #22561 ) ;
#12920 = CARTESIAN_POINT ( 'NONE',  ( 13.14518615778179900, 38.71796875108393721, 5.444914386472293977 ) ) ;
#12921 = CARTESIAN_POINT ( 'NONE',  ( 102.4999999999999716, 123.0500000000000114, -1.035533905932742638 ) ) ;
#12922 = CARTESIAN_POINT ( 'NONE',  ( 208.5748159460630120, 34.30273437500000000, -5.622872871577873077 ) ) ;
#12923 = CARTESIAN_POINT ( 'NONE',  ( 93.46109445667491400, 114.7507929638356785, -45.57500000273119412 ) ) ;
#12924 = CARTESIAN_POINT ( 'NONE',  ( 84.99999999999998579, 95.00000000000000000, -15.00000000000000533 ) ) ;
#12925 = CARTESIAN_POINT ( 'NONE',  ( 55.70494972787295751, 37.27929687608393294, -9.295050272127046043 ) ) ;
#12926 = CARTESIAN_POINT ( 'NONE',  ( 98.15313185440923860, -4.458734124999987891, 0.6250000013655921949 ) ) ;
#12927 = DIRECTION ( 'NONE',  ( 5.782411586589358625E-17, -0.000000000000000000, 1.000000000000000000 ) ) ;
#12928 = CARTESIAN_POINT ( 'NONE',  ( 103.1528011352953484, 91.43749999863440792, -3.152801135295366208 ) ) ;
#12929 = CARTESIAN_POINT ( 'NONE',  ( 95.00000000000000000, 93.31249999726880162, -2.071067811865479058 ) ) ;
#12930 = CARTESIAN_POINT ( 'NONE',  ( -13.57481594606304576, 37.03124999999999289, 0.000000000000000000 ) ) ;
#12931 = CARTESIAN_POINT ( 'NONE',  ( 107.0000000000000000, 110.0000000000000000, -53.49999999453763877 ) ) ;
#12932 = ORIENTED_EDGE ( 'NONE', *, *, #6660, .F. ) ;
#12933 = CARTESIAN_POINT ( 'NONE',  ( 104.4587341249999781, 80.12500000136560629, 1.846868145590721655 ) ) ;
#12934 = AXIS2_PLACEMENT_3D ( 'NONE', #8266, #16954, #5626 ) ;
#12935 = CARTESIAN_POINT ( 'NONE',  ( 104.4587341249999923, 95.24999999863437949, 1.846868145590726318 ) ) ;
#12936 = ORIENTED_EDGE ( 'NONE', *, *, #20813, .T. ) ;
#12937 = CARTESIAN_POINT ( 'NONE',  ( 105.6631189606246295, 105.8855032339526758, -48.20000000000001705 ) ) ;
#12938 = CARTESIAN_POINT ( 'NONE',  ( 51.85481384221820633, 34.40195312608393152, 0.000000000000000000 ) ) ;
#12939 = ORIENTED_EDGE ( 'NONE', *, *, #21200, .T. ) ;
#12940 = CARTESIAN_POINT ( 'NONE',  ( 130.8421075954646540, 53.50112910130381749, -15.00000000000000000 ) ) ;
#12941 = CARTESIAN_POINT ( 'NONE',  ( 95.54126587499995082, -1.846868145590724986, 2.750000001365592084 ) ) ;
#12942 = ORIENTED_EDGE ( 'NONE', *, *, #12644, .T. ) ;
#12943 = CARTESIAN_POINT ( 'NONE',  ( -13.14518615778179544, 34.40195312608393152, 0.000000000000000000 ) ) ;
#12944 = CARTESIAN_POINT ( 'NONE',  ( -9.295050272127046043, 40.65273437608393436, -9.295050272127046043 ) ) ;
#12945 = UNCERTAINTY_MEASURE_WITH_UNIT (LENGTH_MEASURE( 1.000000000000000082E-05 ), #13881, 'distance_accuracy_value', 'NONE');
#12946 = CARTESIAN_POINT ( 'NONE',  ( 189.3771271284221314, 38.07304687716787583, 13.57481594606304753 ) ) ;
#12947 = ADVANCED_FACE ( 'NONE', ( #3844 ), #6032, .F. ) ;
#12948 = CARTESIAN_POINT ( 'NONE',  ( 9.295050272127047819, 36.08867187608392868, 9.295050272127046043 ) ) ;
#12949 = CARTESIAN_POINT ( 'NONE',  ( 7.171390501253594785, 31.30502191632583830, -11.52591802191987114 ) ) ;
#12950 = CARTESIAN_POINT ( 'NONE',  ( 191.8853022544570592, 53.90847045361017109, 14.99999999999995026 ) ) ;
#12951 = CARTESIAN_POINT ( 'NONE',  ( 139.2950502721270425, 37.27929687608394005, -9.295050272127046043 ) ) ;
#12952 = CARTESIAN_POINT ( 'NONE',  ( 5.444914386472297529, 38.12265625108393152, -13.14518615778179900 ) ) ;
#12953 = VECTOR ( 'NONE', #14306, 999.9999999999998863 ) ;
#12954 = CARTESIAN_POINT ( 'NONE',  ( 139.2950502721270425, 34.50117187608393010, 9.295050272127046043 ) ) ;
#12955 = CARTESIAN_POINT ( 'NONE',  ( 78.57481594606304043, 33.40976562499999858, 5.622872871577869525 ) ) ;
#12956 = CARTESIAN_POINT ( 'NONE',  ( 0.000000000000000000, 0.000000000000000000, 25.00000000000000711 ) ) ;
#12957 = ADVANCED_FACE ( 'NONE', ( #7873 ), #5467, .F. ) ;
#12958 = CARTESIAN_POINT ( 'NONE',  ( 101.8468681455906903, 4.458734125000016313, 2.125000001365591640 ) ) ;
#12959 = CARTESIAN_POINT ( 'NONE',  ( 65.00000000000000000, -7.395377635281828788, -7.517135062566165128E-15 ) ) ;
#12960 = CARTESIAN_POINT ( 'NONE',  ( 103.1528011352953342, 3.152801135295383084, 13.06250000136559208 ) ) ;
#12961 = CARTESIAN_POINT ( 'NONE',  ( 99.99999999999998579, 101.5015231886685854, -52.62500000273118417 ) ) ;
#12962 = CARTESIAN_POINT ( 'NONE',  ( 116.8548138422182205, 40.65273437608393436, 0.000000000000000000 ) ) ;
#12963 = AXIS2_PLACEMENT_3D ( 'NONE', #7277, #894, #18117 ) ;
#12964 = CARTESIAN_POINT ( 'NONE',  ( 0.000000000000000000, 40.99999999999999289, 0.000000000000000000 ) ) ;
#12965 = CARTESIAN_POINT ( 'NONE',  ( 13.14518615778179544, 33.01289062608393010, -1.609821015232357215E-15 ) ) ;
#12966 = CARTESIAN_POINT ( 'NONE',  ( 104.9999999999999574, 2.071067811865501263, 7.687500002731186832 ) ) ;
#12967 = EDGE_CURVE ( 'NONE', #5815, #12008, #4954, .T. ) ;
#12968 = CARTESIAN_POINT ( 'NONE',  ( 99.99999999999997158, 101.5015231886685854, -47.37499999726882294 ) ) ;
#12969 = ORIENTED_EDGE ( 'NONE', *, *, #27913, .F. ) ;
#12970 = CARTESIAN_POINT ( 'NONE',  ( 98.82914575430085335, 123.0259891538152743, -1.752307227213801832 ) ) ;
#12971 = CARTESIAN_POINT ( 'NONE',  ( 98.53841926354351699, 122.8500000010924680, -1.461580736456474794 ) ) ;
#12972 = CARTESIAN_POINT ( 'NONE',  ( 181.4251840539369596, 36.23749999999999005, 0.000000000000000000 ) ) ;
#12973 = CARTESIAN_POINT ( 'NONE',  ( 200.4449143864723055, 37.62656250108393863, 13.14518615778179189 ) ) ;
#12974 = EDGE_LOOP ( 'NONE', ( #17836, #22942, #15345, #14256 ) ) ;
#12975 = FACE_OUTER_BOUND ( 'NONE', #17300, .T. ) ;
#12976 = CARTESIAN_POINT ( 'NONE',  ( 107.0000000000000000, 107.7255621263696668, -54.10000000000000853 ) ) ;
#12977 = CARTESIAN_POINT ( 'NONE',  ( 103.1528011352953342, 3.152801135295383084, 14.31250000136559208 ) ) ;
#12978 = ORIENTED_EDGE ( 'NONE', *, *, #26612, .F. ) ;
#12979 = CARTESIAN_POINT ( 'NONE',  ( 95.67376207875072680, 104.0454443415356991, -49.70000000000000995 ) ) ;
#12980 = CARTESIAN_POINT ( 'NONE',  ( -9.295050272127044266, 38.27148437608393294, 9.295050272127047819 ) ) ;
#12981 = CARTESIAN_POINT ( 'NONE',  ( 92.99999999999998579, 110.0000000000000000, -56.49999999453763877 ) ) ;
#12982 = CARTESIAN_POINT ( 'NONE',  ( 143.5748159460630404, 32.81445312716787299, -5.622872871577873077 ) ) ;
#12983 = CARTESIAN_POINT ( 'NONE',  ( 107.0000000000000000, 110.0000000000000000, -55.49999999453763877 ) ) ;
#12984 = EDGE_CURVE ( 'NONE', #21530, #7430, #2315, .T. ) ;
#12985 = CARTESIAN_POINT ( 'NONE',  ( 208.1451861577818079, 35.59257812608393579, -1.609821015232357215E-15 ) ) ;
#12986 = VERTEX_POINT ( 'NONE', #13098 ) ;
#12987 = ORIENTED_EDGE ( 'NONE', *, *, #7591, .F. ) ;
#12988 = VERTEX_POINT ( 'NONE', #26102 ) ;
#12989 = CARTESIAN_POINT ( 'NONE',  ( -5.444914386472299306, 39.31328125108394289, 13.14518615778179722 ) ) ;
#12990 = CARTESIAN_POINT ( 'NONE',  ( 95.54126587499996504, 1.846868145590750077, 10.62500000136559208 ) ) ;
#12991 = CARTESIAN_POINT ( 'NONE',  ( 102.0710678118654329, 91.18749999999997158, -5.000000000000011546 ) ) ;
#12992 = CARTESIAN_POINT ( 'NONE',  ( 104.4587341249999781, 80.00000000136560629, -1.846868145590750521 ) ) ;
#12993 = CARTESIAN_POINT ( 'NONE',  ( 189.5550856135277229, 38.81718750108393579, -13.14518615778179722 ) ) ;
#12994 = CARTESIAN_POINT ( 'NONE',  ( -13.14518615778179544, 39.16445312608393436, 0.000000000000000000 ) ) ;
#12995 = CARTESIAN_POINT ( 'NONE',  ( 187.3637589319962160, 54.91786508990981730, 14.99999999999995026 ) ) ;
#12996 = VECTOR ( 'NONE', #1148, 1000.000000000000000 ) ;
#12997 = CARTESIAN_POINT ( 'NONE',  ( 99.99999999999995737, 85.00000000000000000, -1.387778780781445676E-14 ) ) ;
#12998 = CARTESIAN_POINT ( 'NONE',  ( 195.0000000000000000, -7.395377635281828788, -2.255140518769849538E-14 ) ) ;
#12999 = CARTESIAN_POINT ( 'NONE',  ( 102.4976396683250783, 102.3130555110000159, -51.02499999726882152 ) ) ;
#13000 = ORIENTED_EDGE ( 'NONE', *, *, #5180, .T. ) ;
#13001 = CARTESIAN_POINT ( 'NONE',  ( 13.57481594606304753, 36.68398437499999432, -5.622872871577873077 ) ) ;
#13002 = CARTESIAN_POINT ( 'NONE',  ( 13.14518615778179900, 36.23750000108393010, -5.444914386472297529 ) ) ;
#13003 = CARTESIAN_POINT ( 'NONE',  ( 96.46446609406721961, -3.535533905932727539, 2.250000002731185500 ) ) ;
#13004 = CARTESIAN_POINT ( 'NONE',  ( 135.4449143864723055, 37.82500000108392868, 13.14518615778179189 ) ) ;
#13005 = CARTESIAN_POINT ( 'NONE',  ( 78.14518615778179367, 32.21914062608393436, -1.609821015232357215E-15 ) ) ;
#13006 = CARTESIAN_POINT ( 'NONE',  ( 189.5550856135277229, 37.72578125108395142, 13.14518615778179722 ) ) ;
#13007 = DIRECTION ( 'NONE',  ( -1.000000000000000000, 0.000000000000000000, 0.000000000000000000 ) ) ;
#13008 = FILL_AREA_STYLE_COLOUR ( '', #2873 ) ;
#13009 =( BOUNDED_CURVE ( )  B_SPLINE_CURVE ( 2, ( #10166, #18875, #2485, #23723, #24004, #24282, #11145, #6744, #26429, #13278, #19580, #6889, #2350, #6467, #12857, #6602, #28139, #17437, #15001, #64, #11291, #26136, #15286, #23859, #20012, #19441, #8606, #10870, #19861, #4763, #8746, #4481, #8466, #17154, #13137, #12993, #19718, #17294, #21873, #203, #25996, #11006, #15141, #8888, #9035, #348, #4337, #17578, #17727, #13423, #26284, #22008, #15429, #15574, #24143, #21733, #4620, #22149, #2630, #25856, #2207, #6327, #4198, #21586, #10732, #2062, #5333, #20582, #16290, #20440, #1065, #24992, #5472, #13998, #22723, #11434, #9450, #3189, #22294, #18149, #15996, #11573, #24713, #27149, #26863, #18006, #7309, #3047, #634, #11860, #3328, #5190, #13853 ),
 .UNSPECIFIED., .F., .T. ) 
 B_SPLINE_CURVE_WITH_KNOTS ( ( 3, 2, 2, 2, 2, 2, 2, 2, 2, 2, 2, 2, 2, 2, 2, 2, 2, 2, 2, 2, 2, 2, 2, 2, 2, 2, 2, 2, 2, 2, 2, 2, 2, 2, 2, 2, 2, 2, 2, 2, 2, 2, 2, 2, 2, 2, 3 ),
 ( 0.000000000000000000, 0.01041666666666666609, 0.02083333333333333218, 0.03125000000000000000, 0.04166666666666666435, 0.05208333333333333565, 0.06250000000000000000, 0.07291666666666667129, 0.08333333333333332871, 0.09374999999999998612, 0.1041666666666666713, 0.1145833333333333287, 0.1250000000000000000, 0.1354166666666666574, 0.1458333333333333426, 0.1562500000000000000, 0.1666666666666666574, 0.1770833333333333426, 0.1874999999999999722, 0.1979166666666666574, 0.2083333333333333426, 0.2187500000000000000, 0.2291666666666666574, 0.2395833333333333426, 0.2500000000000000000, 0.2604166666666666852, 0.2708333333333333148, 0.2812500000000000000, 0.2916666666666666852, 0.3020833333333333148, 0.3125000000000000000, 0.3229166666666666852, 0.3333333333333333148, 0.3437500000000000000, 0.3541666666666666852, 0.3645833333333333148, 0.3749999999999999445, 0.3854166666666666852, 0.3958333333333333148, 0.4062500000000000000, 0.4166666666666666852, 0.4270833333333333148, 0.4375000000000000000, 0.4479166666666666852, 0.4583333333333333148, 0.4687500000000000000, 0.4779971559588570562 ),
 .UNSPECIFIED. ) 
 CURVE ( )  GEOMETRIC_REPRESENTATION_ITEM ( )  RATIONAL_B_SPLINE_CURVE ( ( 1.000000000000000000, 0.9238795325112867385, 1.000000000000000000, 0.9238795325112867385, 1.000000000000000000, 0.9238795325112867385, 1.000000000000000000, 0.9238795325112867385, 1.000000000000000000, 0.9238795325112867385, 1.000000000000000000, 0.9238795325112867385, 1.000000000000000000, 0.9238795325112867385, 1.000000000000000000, 0.9238795325112867385, 1.000000000000000000, 0.9238795325112867385, 1.000000000000000000, 0.9238795325112867385, 1.000000000000000000, 0.9238795325112867385, 1.000000000000000000, 0.9238795325112867385, 1.000000000000000000, 0.9238795325112867385, 1.000000000000000000, 0.9238795325112867385, 1.000000000000000000, 0.9238795325112867385, 1.000000000000000000, 0.9238795325112867385, 1.000000000000000000, 0.9238795325112867385, 1.000000000000000000, 0.9238795325112867385, 1.000000000000000000, 0.9238795325112867385, 1.000000000000000000, 0.9238795325112867385, 1.000000000000000000, 0.9238795325112867385, 1.000000000000000000, 0.9238795325112867385, 1.000000000000000000, 0.9238795325112867385, 1.000000000000000000, 0.9238795325112867385, 1.000000000000000000, 0.9238795325112867385, 1.000000000000000000, 0.9238795325112867385, 1.000000000000000000, 0.9238795325112867385, 1.000000000000000000, 0.9238795325112867385, 1.000000000000000000, 0.9238795325112867385, 1.000000000000000000, 0.9238795325112867385, 1.000000000000000000, 0.9238795325112867385, 1.000000000000000000, 0.9238795325112867385, 1.000000000000000000, 0.9238795325112867385, 1.000000000000000000, 0.9238795325112867385, 1.000000000000000000, 0.9238795325112867385, 1.000000000000000000, 0.9238795325112867385, 1.000000000000000000, 0.9238795325112867385, 1.000000000000000000, 0.9238795325112867385, 1.000000000000000000, 0.9238795325112867385, 1.000000000000000000, 0.9238795325112867385, 1.000000000000000000, 0.9238795325112867385, 1.000000000000000000, 0.9238795325112867385, 1.000000000000000000, 0.9238795325112867385, 1.000000000000000000, 0.9238795325112867385, 1.000000000000000000, 0.9238795325112867385, 1.000000000000000000, 0.9324258078851931364, 0.9848264816800285093 ) ) 
 REPRESENTATION_ITEM ( '' )  );
#13010 = CARTESIAN_POINT ( 'NONE',  ( 129.6713997234275269, 53.49358765998905341, -15.00000000000000000 ) ) ;
#13011 = AXIS2_PLACEMENT_3D ( 'NONE', #21538, #27822, #12533 ) ;
#13012 = CARTESIAN_POINT ( 'NONE',  ( -5.622872871577816234, 38.56914062716787583, -13.57481594606310260 ) ) ;
#13013 = CARTESIAN_POINT ( 'NONE',  ( 214.9999999999999716, 55.00000000000000000, 9.999999999999946709 ) ) ;
#13014 = CARTESIAN_POINT ( 'NONE',  ( 95.00472066334981491, 116.8754121666685393, -51.42500000273118843 ) ) ;
#13015 = CARTESIAN_POINT ( 'NONE',  ( -9.295050272127044266, 35.09648437608392868, 9.295050272127047819 ) ) ;
#13016 = CIRCLE ( 'NONE', #25351, 25.00000000000000711 ) ;
#13017 = CARTESIAN_POINT ( 'NONE',  ( 2.493653234604083739E-15, 34.84843749999999574, 13.57481594606304576 ) ) ;
#13018 = CARTESIAN_POINT ( 'NONE',  ( 97.50000000000000000, 124.3000000021849587, -9.540979117872439019E-15 ) ) ;
#13019 = AXIS2_PLACEMENT_3D ( 'NONE', #7630, #16322, #25023 ) ;
#13020 = CARTESIAN_POINT ( 'NONE',  ( 55.81982418635199394, 55.00000000000000711, 14.99999999999998224 ) ) ;
#13021 = LINE ( 'NONE', #10619, #15432 ) ;
#13022 = CARTESIAN_POINT ( 'NONE',  ( 99.99999999999995737, -4.458734124999988779, 7.687500001365592084 ) ) ;
#13023 = VERTEX_POINT ( 'NONE', #11113 ) ;
#13024 = CARTESIAN_POINT ( 'NONE',  ( 101.4615807364564546, 123.2500000010924879, 1.461580736456455476 ) ) ;
#13025 = CARTESIAN_POINT ( 'NONE',  ( 96.84719886470459471, -3.152801135295355994, 12.56250000136559208 ) ) ;
#13026 = CARTESIAN_POINT ( 'NONE',  ( 128.3974668693900298, 53.60343507247939954, 14.99999999999996447 ) ) ;
#13027 = CARTESIAN_POINT ( 'NONE',  ( -9.295050272127046043, 38.86679687608393863, -9.295050272127046043 ) ) ;
#13028 = FACE_OUTER_BOUND ( 'NONE', #14345, .T. ) ;
#13029 = CARTESIAN_POINT ( 'NONE',  ( 98.15313185440925281, 79.87500000136559208, 4.458734124999987891 ) ) ;
#13030 = CARTESIAN_POINT ( 'NONE',  ( 55.70494972787295751, 34.50117187608393721, 9.295050272127047819 ) ) ;
#13031 = CARTESIAN_POINT ( 'NONE',  ( 91.91746824999999887, 110.0000000000000000, -53.12500000273119838 ) ) ;
#13032 = DIRECTION ( 'NONE',  ( -0.000000000000000000, 1.000000000000000000, -0.000000000000000000 ) ) ;
#13033 = AXIS2_PLACEMENT_3D ( 'NONE', #13386, #19974, #26244 ) ;
#13034 = CARTESIAN_POINT ( 'NONE',  ( 104.9999999999999716, 80.56250000273119838, 2.071067811865462627 ) ) ;
#13035 = DIRECTION ( 'NONE',  ( 1.000000000000000000, 0.000000000000000000, 0.000000000000000000 ) ) ;
#13036 = CARTESIAN_POINT ( 'NONE',  ( 104.3262379212492448, 115.9545556584642867, -55.19999999453763451 ) ) ;
#13037 = CARTESIAN_POINT ( 'NONE',  ( 120.4011555911795455, 36.93203124999999432, -9.598844408820458085 ) ) ;
#13038 = ORIENTED_EDGE ( 'NONE', *, *, #18718, .T. ) ;
#13039 = DIRECTION ( 'NONE',  ( -0.000000000000000000, -1.000000000000000000, -0.000000000000000000 ) ) ;
#13040 = ADVANCED_FACE ( 'NONE', ( #8286 ), #13667, .T. ) ;
#13041 = CARTESIAN_POINT ( 'NONE',  ( 2.414731522848535132E-15, 35.39414062608393863, 13.14518615778179544 ) ) ;
#13042 = CARTESIAN_POINT ( 'NONE',  ( 5.622872871577878406, 38.17226562716786731, 13.57481594606304576 ) ) ;
#13043 = CARTESIAN_POINT ( 'NONE',  ( 143.1451861577818079, 36.13828125108393863, 5.444914386472293977 ) ) ;
#13044 = PRODUCT_DEFINITION_SHAPE ( 'NONE', 'NONE',  #21636 ) ;
#13045 = CARTESIAN_POINT ( 'NONE',  ( 51.42518405393695957, 34.00507812716787015, 5.622872871577880183 ) ) ;
#13046 = CARTESIAN_POINT ( 'NONE',  ( 12.89215161363535778, 36.00000000000001421, -4.169510824908217117 ) ) ;
#13047 = CARTESIAN_POINT ( 'NONE',  ( -5.622872871577873077, 31.42539062716787157, -13.57481594606304753 ) ) ;
#13048 = CARTESIAN_POINT ( 'NONE',  ( 97.92893218813451028, -4.999999999999989342, 7.187499999999999112 ) ) ;
#13049 = CARTESIAN_POINT ( 'NONE',  ( 96.46446609406721961, 84.87500000000000000, -3.535533905932755072 ) ) ;
#13050 = CARTESIAN_POINT ( 'NONE',  ( 181.8548138422182205, 34.20351562608393436, 0.000000000000000000 ) ) ;
#13051 = CIRCLE ( 'NONE', #26754, 23.00000000000001421 ) ;
#13052 = CARTESIAN_POINT ( 'NONE',  ( 78.57481594606305464, 38.96601562499999005, 5.622872871577868636 ) ) ;
#13053 = CARTESIAN_POINT ( 'NONE',  ( 104.9999999999999716, 81.56250000000002842, -2.071067811865491937 ) ) ;
#13054 = CARTESIAN_POINT ( 'NONE',  ( 130.0000000000000000, -7.395377635281828788, -1.503427012513233026E-14 ) ) ;
#13055 = CARTESIAN_POINT ( 'NONE',  ( 204.5988444088204687, 36.53515624999999289, 9.598844408820456309 ) ) ;
#13056 = CARTESIAN_POINT ( 'NONE',  ( -13.57481594606304753, 36.98164062499999005, -5.622872871577873077 ) ) ;
#13057 = DIRECTION ( 'NONE',  ( -0.000000000000000000, 1.000000000000000000, -0.000000000000000000 ) ) ;
#13058 = CARTESIAN_POINT ( 'NONE',  ( 13.14518615778179900, 38.81718750108393579, -5.444914386472297529 ) ) ;
#13059 = CARTESIAN_POINT ( 'NONE',  ( -5.444914386472297529, 40.40468750108393436, -13.14518615778179900 ) ) ;
#13060 = CARTESIAN_POINT ( 'NONE',  ( 185.4011555911795313, 36.13828124999999147, -9.598844408820458085 ) ) ;
#13061 = CARTESIAN_POINT ( 'NONE',  ( 51.42518405393695957, 40.20624999999999005, 0.000000000000000000 ) ) ;
#13062 = CARTESIAN_POINT ( 'NONE',  ( 9.598844408820459861, 38.91640624999999432, 9.598844408820456309 ) ) ;
#13063 = CARTESIAN_POINT ( 'NONE',  ( 74.29505027212704249, 36.08867187608392868, 9.295050272127046043 ) ) ;
#13064 =( BOUNDED_CURVE ( )  B_SPLINE_CURVE ( 2, ( #26788, #13781, #2968, #26644, #2699, #22793, #15791, #26933, #7376 ),
 .UNSPECIFIED., .F., .F. ) 
 B_SPLINE_CURVE_WITH_KNOTS ( ( 3, 2, 2, 2, 3 ),
 ( 0.6785714285714284921, 0.6874999999999998890, 0.6964285714285712858, 0.7053571428571427937, 0.7142857142857141906 ),
 .UNSPECIFIED. ) 
 CURVE ( )  GEOMETRIC_REPRESENTATION_ITEM ( )  RATIONAL_B_SPLINE_CURVE ( ( 1.000000000000000888, 0.9238795325112857393, 1.000000000000000000, 0.9238795325112867385, 1.000000000000000000, 0.9238795325112867385, 1.000000000000000000, 0.9238795325112877377, 0.9999999999999990008 ) ) 
 REPRESENTATION_ITEM ( '' )  );
#13065 = CARTESIAN_POINT ( 'NONE',  ( 98.15313185440923860, 4.458734125000016313, 3.250000001365592972 ) ) ;
#13066 = CARTESIAN_POINT ( 'NONE',  ( 104.3262379212492590, 104.0454443415356991, -43.80000000546238681 ) ) ;
#13067 = CARTESIAN_POINT ( 'NONE',  ( 95.54126587499999346, 93.87499999863439371, 1.846868145590722543 ) ) ;
#13068 = CARTESIAN_POINT ( 'NONE',  ( 97.92893218813449607, 93.18749999726877320, -4.999999999999971578 ) ) ;
#13069 = CARTESIAN_POINT ( 'NONE',  ( -9.598844408820458085, 37.72578124999999005, -9.598844408820458085 ) ) ;
#13070 = CARTESIAN_POINT ( 'NONE',  ( 130.0000000000000000, 37.77539062608393294, 13.14518615778179544 ) ) ;
#13071 = ORIENTED_EDGE ( 'NONE', *, *, #1327, .F. ) ;
#13072 = VERTEX_POINT ( 'NONE', #16943 ) ;
#13073 = CARTESIAN_POINT ( 'NONE',  ( 98.15313185440925281, 80.50000000136560629, -4.458734125000016313 ) ) ;
#13074 = EDGE_CURVE ( 'NONE', #10899, #4535, #26210, .T. ) ;
#13075 = CARTESIAN_POINT ( 'NONE',  ( 101.8468681455907330, 93.12499999863439371, 4.458734124999979898 ) ) ;
#13076 = CARTESIAN_POINT ( 'NONE',  ( 55.92190807730121094, 36.00000000000001421, -9.794392408849049048 ) ) ;
#13077 = ORIENTED_EDGE ( 'NONE', *, *, #22551, .T. ) ;
#13078 = CARTESIAN_POINT ( 'NONE',  ( 105.6631189606246153, 114.1144967660473242, -51.80000000000001137 ) ) ;
#13079 = CARTESIAN_POINT ( 'NONE',  ( 59.55508561352770158, 35.84062500108394289, -13.14518615778179900 ) ) ;
#13080 = ORIENTED_EDGE ( 'NONE', *, *, #11709, .T. ) ;
#13081 = CARTESIAN_POINT ( 'NONE',  ( 135.6228728715777549, 38.96601562716787015, 13.57481594606318076 ) ) ;
#13082 = CARTESIAN_POINT ( 'NONE',  ( 101.8468681455906903, 4.458734125000016313, 1.375000001365592972 ) ) ;
#13083 = ORIENTED_EDGE ( 'NONE', *, *, #21558, .T. ) ;
#13084 = CARTESIAN_POINT ( 'NONE',  ( -5.444914386472299306, 35.34453125108393579, 13.14518615778179722 ) ) ;
#13085 = CARTESIAN_POINT ( 'NONE',  ( -5.444914386472297529, 39.80937500108392868, -13.14518615778179900 ) ) ;
#13086 = CARTESIAN_POINT ( 'NONE',  ( 200.6228728715778686, 38.96601562716787015, 13.57481594606304576 ) ) ;
#13087 = CARTESIAN_POINT ( 'NONE',  ( -13.14518615778179722, 37.32890625108393579, -5.444914386472297529 ) ) ;
#13088 = LINE ( 'NONE', #15236, #1729 ) ;
#13089 = CARTESIAN_POINT ( 'NONE',  ( 143.1451861577818079, 36.38632812608393863, -1.609821015232357215E-15 ) ) ;
#13090 = CARTESIAN_POINT ( 'NONE',  ( -13.14518615778179189, 38.42031250108393436, 5.444914386472304635 ) ) ;
#13091 = CARTESIAN_POINT ( 'NONE',  ( 120.7049497278729575, 35.89023437608393152, 9.295050272127047819 ) ) ;
#13092 = CARTESIAN_POINT ( 'NONE',  ( 51.42518405393695957, 34.69960937499999432, 5.622872871577880183 ) ) ;
#13093 = CYLINDRICAL_SURFACE ( 'NONE', #8678, 13.57481594606304576 ) ;
#13094 = AXIS2_PLACEMENT_3D ( 'NONE', #6509, #15185, #12770 ) ;
#13095 = CARTESIAN_POINT ( 'NONE',  ( 95.54126587499995082, 1.846868145590750077, 12.62500000136559208 ) ) ;
#13096 = ADVANCED_FACE ( 'NONE', ( #1995 ), #25929, .F. ) ;
#13097 = CARTESIAN_POINT ( 'NONE',  ( 99.99999999999995737, -4.458734124999988779, 12.68750000136559208 ) ) ;
#13098 = CARTESIAN_POINT ( 'NONE',  ( 93.00000000000000000, 110.0000000000000000, -48.00000000000000711 ) ) ;
#13099 = AXIS2_PLACEMENT_3D ( 'NONE', #15425, #7557, #11677 ) ;
#13100 = CARTESIAN_POINT ( 'NONE',  ( 101.7677669529663547, 123.7000000000000028, 1.767766952966350891 ) ) ;
#13101 =( BOUNDED_CURVE ( )  B_SPLINE_CURVE ( 2, ( #3768, #12429, #27711, #16865, #25563, #14711, #6586, #8590, #188 ),
 .UNSPECIFIED., .F., .F. ) 
 B_SPLINE_CURVE_WITH_KNOTS ( ( 3, 2, 2, 2, 3 ),
 ( 0.3125000000000002220, 0.3229166666666668517, 0.3333333333333334259, 0.3437500000000000555, 0.3541666666666666852 ),
 .UNSPECIFIED. ) 
 CURVE ( )  GEOMETRIC_REPRESENTATION_ITEM ( )  RATIONAL_B_SPLINE_CURVE ( ( 0.9999999999999983347, 0.9238795325112884038, 1.000000000000000000, 0.9238795325112867385, 1.000000000000000000, 0.9238795325112867385, 1.000000000000000000, 0.9238795325112867385, 1.000000000000000000 ) ) 
 REPRESENTATION_ITEM ( '' )  );
#13102 = DIRECTION ( 'NONE',  ( -0.000000000000000000, -1.000000000000000000, -0.000000000000000000 ) ) ;
#13103 = CARTESIAN_POINT ( 'NONE',  ( 108.0825317500000011, 110.0000000000000000, -48.62499999726882294 ) ) ;
#13104 = CARTESIAN_POINT ( 'NONE',  ( 5.444914386472297529, 35.74140625108393721, -13.14518615778179900 ) ) ;
#13105 = CARTESIAN_POINT ( 'NONE',  ( 91.91746824999997045, 112.6261737610028320, -47.97499999726881725 ) ) ;
#13106 = VERTEX_POINT ( 'NONE', #27800 ) ;
#13107 = CARTESIAN_POINT ( 'NONE',  ( 100.8561741729129295, 124.5000000010924737, -2.066987299999998751 ) ) ;
#13109 = ADVANCED_FACE ( 'NONE', ( #6672 ), #21240, .T. ) ;
#13108 = FACE_OUTER_BOUND ( 'NONE', #14499, .T. ) ;
#13110 = CARTESIAN_POINT ( 'NONE',  ( -8.312177448680279460E-16, 38.51953125216787299, -13.57481594606304576 ) ) ;
#13111 = EDGE_CURVE ( 'NONE', #8015, #15078, #6262, .T. ) ;
#13112 = CARTESIAN_POINT ( 'NONE',  ( 208.1451861577817795, 40.10703125108393152, 5.444914386472293977 ) ) ;
#13113 = ORIENTED_EDGE ( 'NONE', *, *, #24870, .T. ) ;
#13114 = CARTESIAN_POINT ( 'NONE',  ( 99.99999999999998579, 95.00000000000000000, 4.999999999999983125 ) ) ;
#13115 = EDGE_CURVE ( 'NONE', #6189, #26410, #3214, .T. ) ;
#13116 = CARTESIAN_POINT ( 'NONE',  ( 65.00000000000000000, -7.395377635281828788, -7.517135062566165128E-15 ) ) ;
#13117 = CARTESIAN_POINT ( 'NONE',  ( 104.4587341249999781, 1.846868145590750299, 13.25000000136559208 ) ) ;
#13118 = VERTEX_POINT ( 'NONE', #3995 ) ;
#13119 = CARTESIAN_POINT ( 'NONE',  ( 97.83688103937538472, 116.6573956140660897, -52.40000000000000568 ) ) ;
#13120 = CARTESIAN_POINT ( 'NONE',  ( -13.14518615778179544, 39.75976562608393294, 0.000000000000000000 ) ) ;
#13121 = AXIS2_PLACEMENT_3D ( 'NONE', #10232, #1297, #6117 ) ;
#13122 = CARTESIAN_POINT ( 'NONE',  ( 99.99999999999998579, 110.0000000000000000, -145.0000000000000284 ) ) ;
#13123 = ADVANCED_FACE ( 'NONE', ( #23932, #8393 ), #4268, .T. ) ;
#13124 = CARTESIAN_POINT ( 'NONE',  ( 137.1713913950166557, 31.30502190640808990, -11.52591746582321974 ) ) ;
#13125 = CARTESIAN_POINT ( 'NONE',  ( -5.444914386472299306, 40.10703125108393152, 13.14518615778179722 ) ) ;
#13126 =( REPRESENTATION_RELATIONSHIP ('NONE','NONE', #2411, #9145 ) REPRESENTATION_RELATIONSHIP_WITH_TRANSFORMATION ( #7843 )SHAPE_REPRESENTATION_RELATIONSHIP( ) );
#13127 = CARTESIAN_POINT ( 'NONE',  ( 104.9999999999999858, 94.87499999726881583, -6.938893903907228378E-15 ) ) ;
#13128 = CARTESIAN_POINT ( 'NONE',  ( 78.14518615778179367, 37.13046875108393863, 5.444914386472293977 ) ) ;
#13129 = CARTESIAN_POINT ( 'NONE',  ( -13.57481594606304398, 34.79882812716788010, 5.622872871577880183 ) ) ;
#13130 = CARTESIAN_POINT ( 'NONE',  ( 204.2950502721270425, 35.69179687608394147, -9.295050272127046043 ) ) ;
#13131 = VERTEX_POINT ( 'NONE', #14935 ) ;
#13132 = ORIENTED_EDGE ( 'NONE', *, *, #14355, .T. ) ;
#13133 = CARTESIAN_POINT ( 'NONE',  ( 9.295050272127046043, 39.66054687608393436, -9.295050272127046043 ) ) ;
#13134 = CARTESIAN_POINT ( 'NONE',  ( 96.84719886470459471, 3.152801135295383084, 12.56250000136559208 ) ) ;
#13135 = EDGE_CURVE ( 'NONE', #2438, #19624, #26409, .T. ) ;
#13136 = CARTESIAN_POINT ( 'NONE',  ( 101.8468681455907046, 81.12500000136560629, -4.458734125000016313 ) ) ;
#13137 = CARTESIAN_POINT ( 'NONE',  ( 185.7049497278729575, 38.86679687608393863, -9.295050272127046043 ) ) ;
#13138 = CARTESIAN_POINT ( 'NONE',  ( 2.414731522848535132E-15, 36.98164062608393721, 13.14518615778179544 ) ) ;
#13139 = CARTESIAN_POINT ( 'NONE',  ( 190.0749732163493206, 49.99999999893116609, 12.67776588292511519 ) ) ;
#13140 = CARTESIAN_POINT ( 'NONE',  ( -9.598844408820454532, 37.92421874999999432, 9.598844408820459861 ) ) ;
#13141 = CIRCLE ( 'NONE', #11804, 4.999999999999997335 ) ;
#13142 = CARTESIAN_POINT ( 'NONE',  ( -15.00000000000000355, 50.00000000000000000, -14.99999999999999822 ) ) ;
#13143 = CARTESIAN_POINT ( 'NONE',  ( 104.9952793366501709, 116.8754121666685393, -52.32499999726881867 ) ) ;
#13144 = ORIENTED_EDGE ( 'NONE', *, *, #11012, .T. ) ;
#13145 = ADVANCED_FACE ( 'NONE', ( #4132 ), #12658, .T. ) ;
#13146 = CARTESIAN_POINT ( 'NONE',  ( -5.622872871577873077, 37.18007812500000853, 13.57481594606304753 ) ) ;
#13147 = CARTESIAN_POINT ( 'NONE',  ( -13.14518615778179189, 36.63437500108393152, 5.444914386472304635 ) ) ;
#13148 = CARTESIAN_POINT ( 'NONE',  ( 95.54126587499995082, 1.846868145590750077, 14.37500000136559386 ) ) ;
#13149 = CARTESIAN_POINT ( 'NONE',  ( 116.8548138422182205, 35.98945312608393721, 0.000000000000000000 ) ) ;
#13150 = CARTESIAN_POINT ( 'NONE',  ( 51.85481384221819923, 34.15390625108393863, -5.444914386472297529 ) ) ;
#13151 = EDGE_CURVE ( 'NONE', #26276, #3364, #17496, .T. ) ;
#13152 = CARTESIAN_POINT ( 'NONE',  ( 200.4449143864723055, 37.03125000108393294, 13.14518615778179189 ) ) ;
#13153 = ORIENTED_EDGE ( 'NONE', *, *, #26208, .T. ) ;
#13154 = DIRECTION ( 'NONE',  ( 0.000000000000000000, 0.000000000000000000, 1.000000000000000000 ) ) ;
#13155 = CARTESIAN_POINT ( 'NONE',  ( 2.414731522848535132E-15, 32.81445312608393294, 13.14518615778179544 ) ) ;
#13156 = CARTESIAN_POINT ( 'NONE',  ( 181.9040934463640156, 36.00000000000000000, 1.137167824541468031 ) ) ;
#13157 = FACE_OUTER_BOUND ( 'NONE', #13896, .T. ) ;
#13158 = CARTESIAN_POINT ( 'NONE',  ( 78.57481594606305464, 40.55351562499999574, 5.622872871577868636 ) ) ;
#13159 = LINE ( 'NONE', #4784, #24938 ) ;
#13160 = CARTESIAN_POINT ( 'NONE',  ( -1.605271876576585877, 53.60388944777322706, 14.99999999999999645 ) ) ;
#13161 = CARTESIAN_POINT ( 'NONE',  ( 102.4999999999999716, 123.0500000021849445, 1.035533905932722876 ) ) ;
#13162 = CARTESIAN_POINT ( 'NONE',  ( 57.36375893200157350, 54.91786508990982441, 14.99999999999998046 ) ) ;
#13163 =( LENGTH_UNIT ( ) NAMED_UNIT ( * ) SI_UNIT ( .MILLI., .METRE. ) );
#13164 = CARTESIAN_POINT ( 'NONE',  ( 96.84719886470459471, -3.152801135295355994, 8.562500001365592084 ) ) ;
#13165 = ORIENTED_EDGE ( 'NONE', *, *, #21540, .F. ) ;
#13166 = CARTESIAN_POINT ( 'NONE',  ( 97.50000000000000000, 122.7000000021849502, -9.540979117872439019E-15 ) ) ;
#13167 = CARTESIAN_POINT ( 'NONE',  ( 104.4587341249999639, 1.442382525525748735E-14, 13.93750000136559208 ) ) ;
#13168 = CARTESIAN_POINT ( 'NONE',  ( 121.5976842187730966, 54.99999999484811752, 14.99999999999996625 ) ) ;
#13169 = CARTESIAN_POINT ( 'NONE',  ( -13.14518615778179189, 38.22187500108393010, 5.444914386472304635 ) ) ;
#13170 = CARTESIAN_POINT ( 'NONE',  ( 9.598844408820456309, 32.76484374999999716, -9.598844408820458085 ) ) ;
#13171 = CARTESIAN_POINT ( 'NONE',  ( 104.4587341249999639, 82.18750000136559208, -1.442382525525748735E-14 ) ) ;
#13172 = CARTESIAN_POINT ( 'NONE',  ( 51.85481384221820633, 36.83281250108393579, 5.444914386472304635 ) ) ;
#13173 = CARTESIAN_POINT ( 'NONE',  ( 97.50236033167492167, 102.3130555110000159, -50.72500000273119980 ) ) ;
#13174 = CARTESIAN_POINT ( 'NONE',  ( 13.14518615778179722, 36.93203125108394147, 5.444914386472293977 ) ) ;
#13175 = CARTESIAN_POINT ( 'NONE',  ( 2.493653234604083739E-15, 36.43593749999999432, 13.57481594606304576 ) ) ;
#13176 = CARTESIAN_POINT ( 'NONE',  ( 120.4011555911795455, 36.13828124999999147, -9.598844408820458085 ) ) ;
#13177 = CARTESIAN_POINT ( 'NONE',  ( 97.83688103937537051, 103.3426043859339103, -56.09999999453764730 ) ) ;
#13178 = CARTESIAN_POINT ( 'NONE',  ( 135.6228728715778686, 35.98945312499999716, -13.57481594606304753 ) ) ;
#13179 = EDGE_CURVE ( 'NONE', #4960, #16430, #20224, .T. ) ;
#13180 = VERTEX_POINT ( 'NONE', #707 ) ;
#13181 = CARTESIAN_POINT ( 'NONE',  ( 105.6631189606246295, 105.8855032339526758, -55.69999999453764161 ) ) ;
#13182 = CARTESIAN_POINT ( 'NONE',  ( -9.295050272127046043, 36.68398437608393436, -9.295050272127046043 ) ) ;
#13183 = CARTESIAN_POINT ( 'NONE',  ( 13.57481594606304576, 38.32109375216786873, -1.662435489736055892E-15 ) ) ;
#13184 =( BOUNDED_CURVE ( )  B_SPLINE_CURVE ( 2, ( #1726, #21389, #21663, #15077, #27804, #3999, #4272, #8684, #1866, #25933, #10531 ),
 .UNSPECIFIED., .F., .T. ) 
 B_SPLINE_CURVE_WITH_KNOTS ( ( 3, 2, 2, 2, 2, 3 ),
 ( 0.9000000000000000222, 0.9200000000000000400, 0.9399999999999999467, 0.9599999999999999645, 0.9799999999999999822, 1.000000000000000000 ),
 .UNSPECIFIED. ) 
 CURVE ( )  GEOMETRIC_REPRESENTATION_ITEM ( )  RATIONAL_B_SPLINE_CURVE ( ( 1.000000000000000000, 0.9510565162951535312, 1.000000000000000000, 0.9510565162951535312, 1.000000000000000000, 0.9510565162951535312, 1.000000000000000000, 0.9510565162951535312, 1.000000000000000000, 0.9510565162951535312, 1.000000000000000000 ) ) 
 REPRESENTATION_ITEM ( '' )  );
#13185 = CARTESIAN_POINT ( 'NONE',  ( 139.2950502721270425, 36.08867187608392868, 9.295050272127046043 ) ) ;
#13186 = CARTESIAN_POINT ( 'NONE',  ( 70.62287287157788285, 33.40976562716787157, 13.57481594606304576 ) ) ;
#13187 = AXIS2_PLACEMENT_3D ( 'NONE', #8256, #21516, #25784 ) ;
#13188 = ORIENTED_EDGE ( 'NONE', *, *, #27304, .T. ) ;
#13189 = CARTESIAN_POINT ( 'NONE',  ( 84.99999999999998579, 95.00000000000000000, 14.99999999999999467 ) ) ;
#13190 = CARTESIAN_POINT ( 'NONE',  ( -8.312177448680279460E-16, 31.37578125216787583, -13.57481594606304576 ) ) ;
#13191 = CARTESIAN_POINT ( 'NONE',  ( 94.99999999999995737, 2.071067811865491048, 4.937500000000000888 ) ) ;
#13192 = DIRECTION ( 'NONE',  ( 0.000000000000000000, 1.000000000000000000, 0.000000000000000000 ) ) ;
#13193 = MECHANICAL_DESIGN_GEOMETRIC_PRESENTATION_REPRESENTATION (  '', ( #25076 ), #4139 ) ;
#13194 = CARTESIAN_POINT ( 'NONE',  ( 195.0000000000000000, 33.60820312608392868, 13.14518615778179544 ) ) ;
#13195 = DIRECTION ( 'NONE',  ( -0.000000000000000000, -1.000000000000000000, -0.000000000000000000 ) ) ;
#13196 = B_SPLINE_CURVE_WITH_KNOTS ( 'NONE', 3,
 ( #12152, #9751, #23017, #6046, #18461, #12017, #21150, #3206, #5491, #8033, #25564, #16590, #1636, #1363, #7761, #18600, #3487, #10153 ),
 .UNSPECIFIED., .F., .F.,
 ( 4, 2, 2, 2, 2, 2, 2, 2, 4 ),
 ( 0.000000000000000000, 0.004618502246277095095, 0.006927753369415642209, 0.009237004492554190191, 0.01039163005412350495, 0.01154625561569281970, 0.01385550673883144401, 0.01616475786197007006, 0.01847400898510869610 ),
 .UNSPECIFIED. ) ;
#13197 = CARTESIAN_POINT ( 'NONE',  ( 104.9999999999999716, 93.06249999999998579, -2.071067811865478170 ) ) ;
#13199 = VERTEX_POINT ( 'NONE', #2704 ) ;
#13198 = CARTESIAN_POINT ( 'NONE',  ( 185.4011555911795313, 40.10703124999999147, -9.598844408820458085 ) ) ;
#13200 = CARTESIAN_POINT ( 'NONE',  ( 95.27063293749995410, 79.28125000204838102, -1.387778780781445676E-14 ) ) ;
#13201 = CARTESIAN_POINT ( 'NONE',  ( 136.0790800205188020, 54.65154858643460756, 14.99999999999996092 ) ) ;
#13202 = CARTESIAN_POINT ( 'NONE',  ( -13.57481594606304576, 37.87460937499999147, 5.622872871577880183 ) ) ;
#13203 = FACE_OUTER_BOUND ( 'NONE', #15914, .T. ) ;
#13204 = CARTESIAN_POINT ( 'NONE',  ( 2.414731522848535132E-15, 36.98164062608393721, 13.14518615778179544 ) ) ;
#13205 = CARTESIAN_POINT ( 'NONE',  ( 5.444914386472302859, 35.24531250108393010, 13.14518615778179189 ) ) ;
#13206 = CARTESIAN_POINT ( 'NONE',  ( 204.5988444088204403, 35.93984374999999432, -9.598844408820458085 ) ) ;
#13207 = CARTESIAN_POINT ( 'NONE',  ( 91.91746824999998466, 107.3738262389971680, -45.27500000273118985 ) ) ;
#13208 = CARTESIAN_POINT ( 'NONE',  ( 130.0000000000000000, 36.43593749999999432, 13.57481594606304576 ) ) ;
#13209 = CARTESIAN_POINT ( 'NONE',  ( 65.00000000000000000, 34.00507812608393721, -13.14518615778179544 ) ) ;
#13210 = CARTESIAN_POINT ( 'NONE',  ( 96.84719886470459471, -3.152801135295355994, 1.562500001365591418 ) ) ;
#13211 = CARTESIAN_POINT ( 'NONE',  ( 97.57936185695767506, 123.0000000000000000, -0.6890590944183185851 ) ) ;
#13212 = DIRECTION ( 'NONE',  ( 1.000000000000000000, 0.000000000000000000, -2.385244779468110248E-16 ) ) ;
#13213 = CARTESIAN_POINT ( 'NONE',  ( -5.622872871577873077, 37.18007812500000853, 13.57481594606304753 ) ) ;
#13214 = CARTESIAN_POINT ( 'NONE',  ( 120.7049497278729575, 39.06523437608392868, -9.295050272127046043 ) ) ;
#13215 = VERTEX_POINT ( 'NONE', #13785 ) ;
#13216 = VERTEX_POINT ( 'NONE', #2973 ) ;
#13217 = CARTESIAN_POINT ( 'NONE',  ( 97.92893218813451028, 83.81250000000001421, -5.000000000000018652 ) ) ;
#13218 = AXIS2_PLACEMENT_3D ( 'NONE', #9615, #16167, #514 ) ;
#13219 = CARTESIAN_POINT ( 'NONE',  ( 104.9999999999999574, 83.68750000273119838, -2.071067811865491937 ) ) ;
#13220 = CARTESIAN_POINT ( 'NONE',  ( 103.5355339059327235, 90.12500000000000000, -3.535533905932738197 ) ) ;
#13221 = CARTESIAN_POINT ( 'NONE',  ( 66.46433772032058585, 36.00000000000002842, -13.46163418879030438 ) ) ;
#13222 = CARTESIAN_POINT ( 'NONE',  ( 93.00000000000000000, 112.2744378736303332, -47.10000000000001563 ) ) ;
#13223 = CARTESIAN_POINT ( 'NONE',  ( 59.37712712842213136, 40.35507812499998437, 13.57481594606304753 ) ) ;
#13224 = ORIENTED_EDGE ( 'NONE', *, *, #10156, .F. ) ;
#13225 = CARTESIAN_POINT ( 'NONE',  ( 13.57481594606304931, 32.71523437716787441, 5.622872871577868636 ) ) ;
#13226 = CARTESIAN_POINT ( 'NONE',  ( 95.54126587499995082, 1.846868145590750077, 4.625000001365592084 ) ) ;
#13227 = ORIENTED_EDGE ( 'NONE', *, *, #27428, .F. ) ;
#13228 = CARTESIAN_POINT ( 'NONE',  ( -13.14518615778179722, 33.55859375108393294, -5.444914386472297529 ) ) ;
#13229 = CARTESIAN_POINT ( 'NONE',  ( -13.14518615778179189, 39.21406250108392300, 5.444914386472304635 ) ) ;
#13230 = CARTESIAN_POINT ( 'NONE',  ( 185.4011555911795597, 35.64218750216787868, 9.598844408820459861 ) ) ;
#13231 = CARTESIAN_POINT ( 'NONE',  ( 9.295050272127046043, 34.69960937608393436, -9.295050272127046043 ) ) ;
#13232 = CARTESIAN_POINT ( 'NONE',  ( -5.622872871577873966, 32.11992187499999574, -13.57481594606304753 ) ) ;
#13233 = PRODUCT_DEFINITION ( 'UNKNOWN', '', #21314, #27459 ) ;
#13234 = CARTESIAN_POINT ( 'NONE',  ( 139.2950502721270425, 37.87460937608393863, 9.295050272127046043 ) ) ;
#13235 = CARTESIAN_POINT ( 'NONE',  ( -13.14518615778179900, 35.93984375108393436, -5.444914386472297529 ) ) ;
#13236 = EDGE_CURVE ( 'NONE', #12623, #10198, #17411, .T. ) ;
#13237 = CARTESIAN_POINT ( 'NONE',  ( 139.2950502721270425, 35.29492187608393294, 9.295050272127046043 ) ) ;
#13238 = CARTESIAN_POINT ( 'NONE',  ( 74.59884440882045453, 34.15390624999999858, 9.598844408820456309 ) ) ;
#13239 = CARTESIAN_POINT ( 'NONE',  ( 94.99999999999995737, 1.387778780781445676E-14, 8.000000000000000000 ) ) ;
#13240 = CARTESIAN_POINT ( 'NONE',  ( 104.4587341249999781, -1.846868145590721655, 12.12500000136559208 ) ) ;
#13241 = CARTESIAN_POINT ( 'NONE',  ( 181.4251840539369596, 36.98164062499999005, -5.622872871577872189 ) ) ;
#13242 = CARTESIAN_POINT ( 'NONE',  ( 103.1528011352953342, -3.152801135295355106, 1.812500001365591640 ) ) ;
#13243 = CARTESIAN_POINT ( 'NONE',  ( 95.00472066334982912, 103.1245878333314323, -50.82500000273118701 ) ) ;
#13244 = CARTESIAN_POINT ( 'NONE',  ( 2.493653234604083739E-15, 38.91640625216786731, 13.57481594606304576 ) ) ;
#13245 = DIRECTION ( 'NONE',  ( -0.000000000000000000, -0.000000000000000000, -1.000000000000000000 ) ) ;
#13246 = CARTESIAN_POINT ( 'NONE',  ( 95.00472066334981491, 116.8754121666685393, -47.92499999726882720 ) ) ;
#13247 = CARTESIAN_POINT ( 'NONE',  ( -9.295050272127044266, 35.29492187608393294, 9.295050272127047819 ) ) ;
#13248 = CARTESIAN_POINT ( 'NONE',  ( 99.99999999999997158, 101.5015231886685854, -49.37499999726882294 ) ) ;
#13249 = ORIENTED_EDGE ( 'NONE', *, *, #22715, .T. ) ;
#13250 = CARTESIAN_POINT ( 'NONE',  ( 107.0000000000000142, 112.2744378736303332, -51.40000000546236691 ) ) ;
#13251 = CARTESIAN_POINT ( 'NONE',  ( 100.8561741729129437, 123.2000000010924765, 2.066987299999979655 ) ) ;
#13252 = DIRECTION ( 'NONE',  ( 0.000000000000000000, 0.000000000000000000, -1.000000000000000000 ) ) ;
#13253 = CARTESIAN_POINT ( 'NONE',  ( 181.8548138422181921, 38.22187500108393010, 5.444914386472304635 ) ) ;
#13254 = EDGE_LOOP ( 'NONE', ( #8280, #21196, #20759, #22123, #3767, #5231, #24970, #2623, #3495, #26424, #5163, #8265, #19106 ) ) ;
#13255 = CARTESIAN_POINT ( 'NONE',  ( 102.0710678118654329, -4.999999999999989342, 7.437500002731187720 ) ) ;
#13256 = CARTESIAN_POINT ( 'NONE',  ( 204.1801758136479918, 55.00000000000000000, -15.00000000000000000 ) ) ;
#13257 = CARTESIAN_POINT ( 'NONE',  ( 96.84719886470459471, -3.152801135295355994, 13.81250000136559208 ) ) ;
#13258 = ORIENTED_EDGE ( 'NONE', *, *, #13961, .T. ) ;
#13259 = CARTESIAN_POINT ( 'NONE',  ( 93.00000000000001421, 112.2744378736303332, -48.10000000000000142 ) ) ;
#13260 = CARTESIAN_POINT ( 'NONE',  ( 13.14518615778179900, 38.61875000108393152, -5.444914386472297529 ) ) ;
#13261 = CARTESIAN_POINT ( 'NONE',  ( 97.50000000000000000, 124.9500000000000028, -1.035533905932742416 ) ) ;
#13262 = CARTESIAN_POINT ( 'NONE',  ( 124.3771271284221314, 32.21914062716787441, -13.57481594606304753 ) ) ;
#13263 = CARTESIAN_POINT ( 'NONE',  ( 9.295050272127047819, 40.25585937608393294, 9.295050272127046043 ) ) ;
#13264 = CARTESIAN_POINT ( 'NONE',  ( 97.92893218813452449, 92.18749999726880162, -4.999999999999997335 ) ) ;
#13265 =( BOUNDED_CURVE ( )  B_SPLINE_CURVE ( 2, ( #13017, #1809, #2231, #21755, #28163, #25734, #2372, #19465, #11030 ),
 .UNSPECIFIED., .F., .F. ) 
 B_SPLINE_CURVE_WITH_KNOTS ( ( 3, 2, 2, 2, 3 ),
 ( 0.6458333333333333703, 0.6562500000000000000, 0.6666666666666665186, 0.6770833333333332593, 0.6874999999999997780 ),
 .UNSPECIFIED. ) 
 CURVE ( )  GEOMETRIC_REPRESENTATION_ITEM ( )  RATIONAL_B_SPLINE_CURVE ( ( 1.000000000000000000, 0.9238795325112867385, 1.000000000000000000, 0.9238795325112867385, 1.000000000000000000, 0.9238795325112867385, 1.000000000000000000, 0.9238795325112884038, 0.9999999999999983347 ) ) 
 REPRESENTATION_ITEM ( '' )  );
#13266 = CARTESIAN_POINT ( 'NONE',  ( 70.44491438647230552, 37.32890625108393579, -13.14518615778179900 ) ) ;
#13267 = EDGE_CURVE ( 'NONE', #21009, #2581, #4033, .T. ) ;
#13268 = CARTESIAN_POINT ( 'NONE',  ( 74.18017581364799184, 55.00000000000000000, -15.00000000000000000 ) ) ;
#13269 = CARTESIAN_POINT ( 'NONE',  ( 195.0000000000000000, 33.40976562608393863, -13.14518615778179544 ) ) ;
#13270 = ADVANCED_FACE ( 'NONE', ( #9938 ), #7673, .F. ) ;
#13271 = EDGE_LOOP ( 'NONE', ( #929, #12939 ) ) ;
#13272 = ORIENTED_EDGE ( 'NONE', *, *, #26943, .T. ) ;
#13273 = CARTESIAN_POINT ( 'NONE',  ( -8.049105076161786076E-16, 38.96601562608393721, -13.14518615778179544 ) ) ;
#13274 = DIRECTION ( 'NONE',  ( 1.000000000000000000, 0.000000000000000000, 0.000000000000000000 ) ) ;
#13275 = CARTESIAN_POINT ( 'NONE',  ( 95.54126587499996504, -1.846868145590724986, 9.750000001365593860 ) ) ;
#13276 = CARTESIAN_POINT ( 'NONE',  ( 101.0355339059327378, 124.7500000000000284, -2.499999999999988010 ) ) ;
#13277 = CARTESIAN_POINT ( 'NONE',  ( 101.8468681455907046, 79.75000000136560629, 4.458734124999987891 ) ) ;
#13278 = CARTESIAN_POINT ( 'NONE',  ( 208.1451861577818079, 40.10703125108393152, 5.444914386472293977 ) ) ;
#13279 = CARTESIAN_POINT ( 'NONE',  ( -13.14518615778179722, 37.52734375108393294, -5.444914386472297529 ) ) ;
#13280 = CARTESIAN_POINT ( 'NONE',  ( 185.8198241863519797, 50.00000000000000000, 9.999999999999948486 ) ) ;
#13281 = CARTESIAN_POINT ( 'NONE',  ( 94.99999999999995737, 1.387778780781445676E-14, 34.79898987322334136 ) ) ;
#13282 = DIRECTION ( 'NONE',  ( -1.156482317317871478E-16, -0.000000000000000000, -1.000000000000000000 ) ) ;
#13283 = CARTESIAN_POINT ( 'NONE',  ( 108.0825317500000011, 110.0000000000000000, -54.62499999726882294 ) ) ;
#13284 = EDGE_CURVE ( 'NONE', #12047, #22508, #36, .T. ) ;
#13285 = ORIENTED_EDGE ( 'NONE', *, *, #6335, .T. ) ;
#13286 = ORIENTED_EDGE ( 'NONE', *, *, #14042, .T. ) ;
#13287 = CARTESIAN_POINT ( 'NONE',  ( -8.312177448680279460E-16, 37.62656249999999858, -13.57481594606304576 ) ) ;
#13288 = CARTESIAN_POINT ( 'NONE',  ( 13.14518615778179900, 38.51953125108393294, 5.444914386472293977 ) ) ;
#13289 = ORIENTED_EDGE ( 'NONE', *, *, #1510, .T. ) ;
#13290 = CARTESIAN_POINT ( 'NONE',  ( 143.1451861577818079, 37.92421875108392726, 5.444914386472293977 ) ) ;
#13291 = CARTESIAN_POINT ( 'NONE',  ( 55.70494972787295751, 34.10429687608393579, -9.295050272127046043 ) ) ;
#13292 = VECTOR ( 'NONE', #5116, 1000.000000000000000 ) ;
#13293 = CARTESIAN_POINT ( 'NONE',  ( 200.4449143864723055, 35.74140625108393721, -13.14518615778179900 ) ) ;
#13294 = ORIENTED_EDGE ( 'NONE', *, *, #2215, .F. ) ;
#13295 = CARTESIAN_POINT ( 'NONE',  ( 95.54126587499996504, 79.56250000136559208, -1.387778780781445676E-14 ) ) ;
#13296 = CARTESIAN_POINT ( 'NONE',  ( 13.14518615778179900, 32.96328125108393436, 5.444914386472293977 ) ) ;
#13297 =( REPRESENTATION_RELATIONSHIP ('NONE','NONE', #2411, #10045 ) REPRESENTATION_RELATIONSHIP_WITH_TRANSFORMATION ( #3576 )SHAPE_REPRESENTATION_RELATIONSHIP( ) );
#13298 = CARTESIAN_POINT ( 'NONE',  ( 125.1415007095402530, 49.99999999891476676, -12.70434618648937963 ) ) ;
#13299 = DIRECTION ( 'NONE',  ( 1.000000000000000000, 0.000000000000000000, -1.156482317317871478E-16 ) ) ;
#13300 = CARTESIAN_POINT ( 'NONE',  ( 195.0000000000000000, 50.00000000000000000, -2.255140518769849538E-14 ) ) ;
#13301 = CARTESIAN_POINT ( 'NONE',  ( 0.000000000000000000, 1.500000000000001332, 0.000000000000000000 ) ) ;
#13302 = CARTESIAN_POINT ( 'NONE',  ( 199.1572863549628210, 35.99999999999999289, -12.92256159328821141 ) ) ;
#13303 = EDGE_CURVE ( 'NONE', #20591, #14157, #16592, .T. ) ;
#13304 = CARTESIAN_POINT ( 'NONE',  ( 101.0355339059327378, 124.0500000021849445, -2.499999999999997780 ) ) ;
#13305 = CARTESIAN_POINT ( 'NONE',  ( 56.24166560764628997, 50.00000000000000000, 10.38725784494103799 ) ) ;
#13306 = ORIENTED_EDGE ( 'NONE', *, *, #10677, .F. ) ;
#13307 =( LENGTH_UNIT ( ) NAMED_UNIT ( * ) SI_UNIT ( .MILLI., .METRE. ) );
#13308 = CARTESIAN_POINT ( 'NONE',  ( 103.1528011352953342, 3.152801135295383084, 8.062500001365592084 ) ) ;
#13309 = VERTEX_POINT ( 'NONE', #14354 ) ;
#13310 = CARTESIAN_POINT ( 'NONE',  ( 102.0669872999999797, 124.1500000010924794, -9.794112055954760458E-15 ) ) ;
#13311 = CARTESIAN_POINT ( 'NONE',  ( 98.15313185440925281, -4.458734124999987891, 13.62500000136559208 ) ) ;
#13312 = CARTESIAN_POINT ( 'NONE',  ( 92.99999999999998579, 110.0000000000000000, -49.00000000000001421 ) ) ;
#13313 = ADVANCED_FACE ( 'NONE', ( #3547 ), #20931, .F. ) ;
#13314 = AXIS2_PLACEMENT_3D ( 'NONE', #5222, #26608, #16177 ) ;
#13315 = CARTESIAN_POINT ( 'NONE',  ( 9.295050272127047819, 37.67617187608393436, 9.295050272127046043 ) ) ;
#13316 = PLANE ( 'NONE',  #3585 ) ;
#13317 = CARTESIAN_POINT ( 'NONE',  ( 95.54126587499996504, 80.68750000136559208, -1.387778780781445676E-14 ) ) ;
#13318 = CARTESIAN_POINT ( 'NONE',  ( 65.00000000000000000, 33.80664062608393294, 13.14518615778179544 ) ) ;
#13319 =( BOUNDED_SURFACE ( )  B_SPLINE_SURFACE ( 1, 2, ( 
 ( #9331, #14022, #11880, #15880, #18174, #22318, #20604, #9473, #659, #26887, #13595, #16021, #24734, #26740, #5214, #15598, #24304, #13878, #13447, #3074, #4788, #22174, #20035, #515, #7043, #14303, #10445, #7626, #25289, #6053, #10029, #16872, #27173, #16318, #5917, #23021, #14717, #23160, #27719, #7765, #25569, #25148, #1368, #12021, #8180, #9894, #10299, #5774, #3636, #21155, #27579, #19006, #25018, #14584, #3775, #22885, #3910, #3494, #16735, #27309, #8038, #14445, #14166, #1641, #25434, #5638, #23435, #12571, #27437, #21298, #1780, #3351, #18605, #5497, #20883, #20745, #1230, #16595, #18739, #16452, #12156, #7901, #23302, #12299, #21024, #1504, #12433, #10158, #18869, #22001, #10860, #2476, #23996, #195, #19153, #25705, #4188, #4328, #23851, #6736, #8456, #21865, #13130, #23714, #12985, #27855, #17001, #17569, #4054, #19711, #8736, #6185, #17429, #12716, #17144, #14855, #2340, #4472, #8598, #17287, #6319, #8314, #1920, #10587, #21578, #10997, #15421, #19432, #2198, #14995, #8877, #25989, #12850, #19572, #27995, #21725, #15130, #2054, #6458, #26274, #24135, #10723, #23573, #57, #4611, #26128, #6594, #21441, #13269, #28131, #19295, #25845, #15276, #15852, #9166, #11283, #3428, #26707, #5580, #5043, #627, #20822, #17859, #9026, #17999, #24561, #20147, #23100, #20282, #15711, #9968, #7015, #1300, #25228, #2764, #13415, #20004, #12096, #9442, #485, #13707, #9302, #11428 ),
 ( #18681, #6879, #4903, #11137, #19852, #2620, #7156, #17719, #22427, #14383, #26420, #26563, #27383, #339, #22141, #16395, #5717, #2896, #7842, #11565, #24413, #15566, #25093, #768, #13565, #24274, #14245, #4755, #18142, #22288, #22966, #26855, #7702, #16536, #12376, #19364, #27655, #20959, #27519, #14653, #25924, #8388, #3845, #17074, #21234, #10236, #12652, #10378, #8533, #27793, #8115, #28067, #21094, #19227, #14931, #10100, #25371, #1990, #19085, #10656, #1583, #18812, #15067, #8250, #4126, #17219, #18946, #1717, #23372, #25638, #16810, #6398, #12231, #3575, #1442, #7975, #25508, #16674, #27928, #23237, #16938, #5852, #12791, #5987, #14522, #21377, #3714, #6121, #12505, #25779, #6257, #23651, #21510, #14787, #23510, #3989, #1855, #10520, #13060, #19508, #17794, #9099, #13206, #21940, #10935, #7089, #6529, #15208, #26204, #6953, #11357, #24068, #6811, #19645, #26496, #2417, #128, #15499, #4406, #270, #19788, #17503, #11076, #2697, #13498, #6667, #2129, #8956, #22218, #17645, #24211, #4262, #15648, #8813, #23785, #12922, #26352, #4690, #21797, #23927, #24346, #20080, #15352, #558, #21654, #10794, #2556, #4544, #9240, #13350, #4837, #2276, #17932, #22079, #11216, #8673, #26642, #19933, #17209, #415, #17365, #26061, #16216, #27213, #24492, #22790, #20649, #11500, #20787, #20364, #5401, #15922, #24917, #3118, #2832, #9801, #14070, #22501, #12062, #1268, #16068, #7668, #9932 ) ),
 .UNSPECIFIED., .F., .F., .F. ) 
 B_SPLINE_SURFACE_WITH_KNOTS ( ( 2, 2 ),
 ( 3, 2, 2, 2, 2, 2, 2, 2, 2, 2, 2, 2, 2, 2, 2, 2, 2, 2, 2, 2, 2, 2, 2, 2, 2, 2, 2, 2, 2, 2, 2, 2, 2, 2, 2, 2, 2, 2, 2, 2, 2, 2, 2, 2, 2, 2, 2, 2, 2, 2, 2, 2, 2, 2, 2, 2, 2, 2, 2, 2, 2, 2, 2, 2, 2, 2, 2, 2, 2, 2, 2, 2, 2, 2, 2, 2, 2, 2, 2, 2, 2, 2, 2, 2, 2, 2, 2, 2, 2, 2, 2, 3 ),
 ( 0.000000000000000000, 1.000000000000000000 ),
 ( 0.000000000000000000, 0.01041666666666666609, 0.02083333333333333218, 0.03125000000000000000, 0.04166666666666666435, 0.05208333333333333565, 0.06250000000000000000, 0.07291666666666667129, 0.08333333333333332871, 0.09375000000000000000, 0.1041666666666666713, 0.1145833333333333287, 0.1250000000000000000, 0.1354166666666666574, 0.1458333333333333426, 0.1562500000000000000, 0.1666666666666666574, 0.1770833333333333426, 0.1875000000000000000, 0.1979166666666666574, 0.2083333333333333426, 0.2187500000000000000, 0.2291666666666666574, 0.2395833333333333426, 0.2500000000000000000, 0.2604166666666666852, 0.2708333333333333148, 0.2812500000000000000, 0.2916666666666666852, 0.3020833333333333148, 0.3125000000000000000, 0.3229166666666666852, 0.3333333333333333148, 0.3437500000000000000, 0.3541666666666666852, 0.3645833333333333148, 0.3750000000000000000, 0.3854166666666666852, 0.3958333333333333148, 0.4062500000000000000, 0.4166666666666666852, 0.4270833333333333148, 0.4375000000000000000, 0.4479166666666666852, 0.4583333333333333148, 0.4687500000000000000, 0.4791666666666666852, 0.4895833333333333148, 0.5000000000000000000, 0.5104166666666666297, 0.5208333333333333703, 0.5312500000000000000, 0.5416666666666666297, 0.5520833333333333703, 0.5625000000000000000, 0.5729166666666666297, 0.5833333333333333703, 0.5937500000000000000, 0.6041666666666666297, 0.6145833333333333703, 0.6250000000000000000, 0.6354166666666666297, 0.6458333333333333703, 0.6562500000000000000, 0.6666666666666666297, 0.6770833333333333703, 0.6875000000000000000, 0.6979166666666666297, 0.7083333333333333703, 0.7187500000000000000, 0.7291666666666666297, 0.7395833333333333703, 0.7500000000000000000, 0.7604166666666666297, 0.7708333333333333703, 0.7812500000000000000, 0.7916666666666666297, 0.8020833333333333703, 0.8125000000000000000, 0.8229166666666666297, 0.8333333333333333703, 0.8437500000000000000, 0.8541666666666666297, 0.8645833333333333703, 0.8750000000000000000, 0.8854166666666666297, 0.8958333333333333703, 0.9062500000000000000, 0.9166666666666666297, 0.9270833333333333703, 0.9375000000000000000, 0.9448586968893691873 ),
 .UNSPECIFIED. ) 
 GEOMETRIC_REPRESENTATION_ITEM ( )  RATIONAL_B_SPLINE_SURFACE ( (
 ( 1.000000000000000000, 0.9238795325112867385, 1.000000000000000000, 0.9238795325112867385, 1.000000000000000000, 0.9238795325112867385, 1.000000000000000000, 0.9238795325112867385, 1.000000000000000000, 0.9238795325112867385, 1.000000000000000000, 0.9238795325112867385, 1.000000000000000000, 0.9238795325112867385, 1.000000000000000000, 0.9238795325112867385, 1.000000000000000000, 0.9238795325112867385, 1.000000000000000000, 0.9238795325112867385, 1.000000000000000000, 0.9238795325112867385, 1.000000000000000000, 0.9238795325112867385, 1.000000000000000000, 0.9238795325112867385, 1.000000000000000000, 0.9238795325112867385, 1.000000000000000000, 0.9238795325112867385, 1.000000000000000000, 0.9238795325112867385, 1.000000000000000000, 0.9238795325112867385, 1.000000000000000000, 0.9238795325112867385, 1.000000000000000000, 0.9238795325112867385, 1.000000000000000000, 0.9238795325112867385, 1.000000000000000000, 0.9238795325112867385, 1.000000000000000000, 0.9238795325112867385, 1.000000000000000000, 0.9238795325112867385, 1.000000000000000000, 0.9238795325112867385, 1.000000000000000000, 0.9238795325112867385, 1.000000000000000000, 0.9238795325112867385, 1.000000000000000000, 0.9238795325112867385, 1.000000000000000000, 0.9238795325112867385, 1.000000000000000000, 0.9238795325112867385, 1.000000000000000000, 0.9238795325112867385, 1.000000000000000000, 0.9238795325112867385, 1.000000000000000000, 0.9238795325112867385, 1.000000000000000000, 0.9238795325112867385, 1.000000000000000000, 0.9238795325112867385, 1.000000000000000000, 0.9238795325112867385, 1.000000000000000000, 0.9238795325112867385, 1.000000000000000000, 0.9238795325112867385, 1.000000000000000000, 0.9238795325112867385, 1.000000000000000000, 0.9238795325112867385, 1.000000000000000000, 0.9238795325112867385, 1.000000000000000000, 0.9238795325112867385, 1.000000000000000000, 0.9238795325112867385, 1.000000000000000000, 0.9238795325112867385, 1.000000000000000000, 0.9238795325112867385, 1.000000000000000000, 0.9238795325112867385, 1.000000000000000000, 0.9238795325112867385, 1.000000000000000000, 0.9238795325112867385, 1.000000000000000000, 0.9238795325112867385, 1.000000000000000000, 0.9238795325112867385, 1.000000000000000000, 0.9238795325112867385, 1.000000000000000000, 0.9238795325112867385, 1.000000000000000000, 0.9238795325112867385, 1.000000000000000000, 0.9238795325112867385, 1.000000000000000000, 0.9238795325112867385, 1.000000000000000000, 0.9238795325112867385, 1.000000000000000000, 0.9238795325112867385, 1.000000000000000000, 0.9238795325112867385, 1.000000000000000000, 0.9238795325112867385, 1.000000000000000000, 0.9238795325112867385, 1.000000000000000000, 0.9238795325112867385, 1.000000000000000000, 0.9238795325112867385, 1.000000000000000000, 0.9238795325112867385, 1.000000000000000000, 0.9238795325112867385, 1.000000000000000000, 0.9238795325112867385, 1.000000000000000000, 0.9238795325112867385, 1.000000000000000000, 0.9238795325112867385, 1.000000000000000000, 0.9238795325112867385, 1.000000000000000000, 0.9238795325112867385, 1.000000000000000000, 0.9238795325112867385, 1.000000000000000000, 0.9238795325112867385, 1.000000000000000000, 0.9238795325112867385, 1.000000000000000000, 0.9238795325112867385, 1.000000000000000000, 0.9238795325112867385, 1.000000000000000000, 0.9238795325112867385, 1.000000000000000000, 0.9238795325112867385, 1.000000000000000000, 0.9238795325112867385, 1.000000000000000000, 0.9238795325112867385, 1.000000000000000000, 0.9238795325112867385, 1.000000000000000000, 0.9238795325112867385, 1.000000000000000000, 0.9238795325112867385, 1.000000000000000000, 0.9238795325112867385, 1.000000000000000000, 0.9238795325112867385, 1.000000000000000000, 0.9238795325112867385, 1.000000000000000000, 0.9238795325112867385, 1.000000000000000000, 0.9238795325112867385, 1.000000000000000000, 0.9238795325112867385, 1.000000000000000000, 0.9238795325112867385, 1.000000000000000000, 0.9238795325112867385, 1.000000000000000000, 0.9238795325112867385, 1.000000000000000000, 0.9238795325112867385, 1.000000000000000000, 0.9462258450566536361, 0.9684275698016389100),
 ( 1.000000000000000000, 0.9238795325112867385, 1.000000000000000000, 0.9238795325112867385, 1.000000000000000000, 0.9238795325112867385, 1.000000000000000000, 0.9238795325112867385, 1.000000000000000000, 0.9238795325112867385, 1.000000000000000000, 0.9238795325112867385, 1.000000000000000000, 0.9238795325112867385, 1.000000000000000000, 0.9238795325112867385, 1.000000000000000000, 0.9238795325112867385, 1.000000000000000000, 0.9238795325112867385, 1.000000000000000000, 0.9238795325112867385, 1.000000000000000000, 0.9238795325112867385, 1.000000000000000000, 0.9238795325112867385, 1.000000000000000000, 0.9238795325112867385, 1.000000000000000000, 0.9238795325112867385, 1.000000000000000000, 0.9238795325112867385, 1.000000000000000000, 0.9238795325112867385, 1.000000000000000000, 0.9238795325112867385, 1.000000000000000000, 0.9238795325112867385, 1.000000000000000000, 0.9238795325112867385, 1.000000000000000000, 0.9238795325112867385, 1.000000000000000000, 0.9238795325112867385, 1.000000000000000000, 0.9238795325112867385, 1.000000000000000000, 0.9238795325112867385, 1.000000000000000000, 0.9238795325112867385, 1.000000000000000000, 0.9238795325112867385, 1.000000000000000000, 0.9238795325112867385, 1.000000000000000000, 0.9238795325112867385, 1.000000000000000000, 0.9238795325112867385, 1.000000000000000000, 0.9238795325112867385, 1.000000000000000000, 0.9238795325112867385, 1.000000000000000000, 0.9238795325112867385, 1.000000000000000000, 0.9238795325112867385, 1.000000000000000000, 0.9238795325112867385, 1.000000000000000000, 0.9238795325112867385, 1.000000000000000000, 0.9238795325112867385, 1.000000000000000000, 0.9238795325112867385, 1.000000000000000000, 0.9238795325112867385, 1.000000000000000000, 0.9238795325112867385, 1.000000000000000000, 0.9238795325112867385, 1.000000000000000000, 0.9238795325112867385, 1.000000000000000000, 0.9238795325112867385, 1.000000000000000000, 0.9238795325112867385, 1.000000000000000000, 0.9238795325112867385, 1.000000000000000000, 0.9238795325112867385, 1.000000000000000000, 0.9238795325112867385, 1.000000000000000000, 0.9238795325112867385, 1.000000000000000000, 0.9238795325112867385, 1.000000000000000000, 0.9238795325112867385, 1.000000000000000000, 0.9238795325112867385, 1.000000000000000000, 0.9238795325112867385, 1.000000000000000000, 0.9238795325112867385, 1.000000000000000000, 0.9238795325112867385, 1.000000000000000000, 0.9238795325112867385, 1.000000000000000000, 0.9238795325112867385, 1.000000000000000000, 0.9238795325112867385, 1.000000000000000000, 0.9238795325112867385, 1.000000000000000000, 0.9238795325112867385, 1.000000000000000000, 0.9238795325112867385, 1.000000000000000000, 0.9238795325112867385, 1.000000000000000000, 0.9238795325112867385, 1.000000000000000000, 0.9238795325112867385, 1.000000000000000000, 0.9238795325112867385, 1.000000000000000000, 0.9238795325112867385, 1.000000000000000000, 0.9238795325112867385, 1.000000000000000000, 0.9238795325112867385, 1.000000000000000000, 0.9238795325112867385, 1.000000000000000000, 0.9238795325112867385, 1.000000000000000000, 0.9238795325112867385, 1.000000000000000000, 0.9238795325112867385, 1.000000000000000000, 0.9238795325112867385, 1.000000000000000000, 0.9238795325112867385, 1.000000000000000000, 0.9238795325112867385, 1.000000000000000000, 0.9238795325112867385, 1.000000000000000000, 0.9238795325112867385, 1.000000000000000000, 0.9238795325112867385, 1.000000000000000000, 0.9238795325112867385, 1.000000000000000000, 0.9238795325112867385, 1.000000000000000000, 0.9238795325112867385, 1.000000000000000000, 0.9238795325112867385, 1.000000000000000000, 0.9238795325112867385, 1.000000000000000000, 0.9238795325112867385, 1.000000000000000000, 0.9238795325112867385, 1.000000000000000000, 0.9238795325112867385, 1.000000000000000000, 0.9238795325112867385, 1.000000000000000000, 0.9238795325112867385, 1.000000000000000000, 0.9238795325112867385, 1.000000000000000000, 0.9238795325112867385, 1.000000000000000000, 0.9238795325112867385, 1.000000000000000000, 0.9238795325112867385, 1.000000000000000000, 0.9462258450566536361, 0.9684275698016389100) ) ) 
 REPRESENTATION_ITEM ( '' )  SURFACE ( )  );
#13320 = CARTESIAN_POINT ( 'NONE',  ( 91.91746824999998466, 107.3738262389971538, -53.02500000273119696 ) ) ;
#13321 = CARTESIAN_POINT ( 'NONE',  ( -13.14518615778179544, 38.17226562608393436, 0.000000000000000000 ) ) ;
#13322 = CARTESIAN_POINT ( 'NONE',  ( -5.622872871577816234, 39.26367187500000000, -13.57481594606310260 ) ) ;
#13323 = DIRECTION ( 'NONE',  ( 5.782411586589358625E-17, -0.000000000000000000, 1.000000000000000000 ) ) ;
#13324 = CARTESIAN_POINT ( 'NONE',  ( 92.99999999999998579, 110.0000000000000000, -54.49999999453763877 ) ) ;
#13325 = CARTESIAN_POINT ( 'NONE',  ( 124.3771271284221314, 38.76757812500000000, 13.57481594606304753 ) ) ;
#13326 = ORIENTED_EDGE ( 'NONE', *, *, #18902, .T. ) ;
#13327 = EDGE_CURVE ( 'NONE', #17637, #5570, #8086, .T. ) ;
#13328 = ORIENTED_EDGE ( 'NONE', *, *, #23943, .T. ) ;
#13329 = DIRECTION ( 'NONE',  ( 0.000000000000000000, 0.000000000000000000, -1.000000000000000000 ) ) ;
#13330 = CARTESIAN_POINT ( 'NONE',  ( -5.444914386472299306, 37.72578125108395142, 13.14518615778179722 ) ) ;
#13331 = CARTESIAN_POINT ( 'NONE',  ( 9.598844408820459861, 35.84062500216786873, 9.598844408820456309 ) ) ;
#13332 = CARTESIAN_POINT ( 'NONE',  ( 102.0710678118654329, 5.000000000000018652, 7.812500002731185056 ) ) ;
#13333 = CARTESIAN_POINT ( 'NONE',  ( 116.8548138422182063, 36.63437500108393152, 5.444914386472304635 ) ) ;
#13334 = CARTESIAN_POINT ( 'NONE',  ( 74.59884440882045453, 35.04687500216787299, 9.598844408820456309 ) ) ;
#13335 = ORIENTED_EDGE ( 'NONE', *, *, #26203, .T. ) ;
#13336 = CARTESIAN_POINT ( 'NONE',  ( 4.859977269582195447, 36.00000000000000000, 12.29462155906275100 ) ) ;
#13337 = CARTESIAN_POINT ( 'NONE',  ( -8.312177448680279460E-16, 33.75703125216787726, -13.57481594606304576 ) ) ;
#13338 = CARTESIAN_POINT ( 'NONE',  ( 101.0355339059327235, 123.7500000021849615, 2.499999999999987121 ) ) ;
#13339 = CARTESIAN_POINT ( 'NONE',  ( 99.99999999999997158, 118.4984768113314146, -46.37499999726881583 ) ) ;
#13340 = CARTESIAN_POINT ( 'NONE',  ( 181.8548138422181921, 35.84062500108394289, 5.444914386472304635 ) ) ;
#13341 = CARTESIAN_POINT ( 'NONE',  ( 116.4251840539369596, 40.99999999999999289, 0.000000000000000000 ) ) ;
#13342 = DIRECTION ( 'NONE',  ( 1.000000000000000000, 0.000000000000000000, -5.782411586589357392E-17 ) ) ;
#13343 = CYLINDRICAL_SURFACE ( 'NONE', #22819, 13.57481594606304398 ) ;
#13344 = CARTESIAN_POINT ( 'NONE',  ( 97.71650635000000307, 124.8750000005462368, -9.540979117872439019E-15 ) ) ;
#13345 = CARTESIAN_POINT ( 'NONE',  ( -13.57481594606304398, 32.41757812716787868, 5.622872871577880183 ) ) ;
#13346 = CARTESIAN_POINT ( 'NONE',  ( 13.57481594606304576, 38.22187499999999716, -1.662435489736055892E-15 ) ) ;
#13347 = CYLINDRICAL_SURFACE ( 'NONE', #8891, 13.57481594606304576 ) ;
#13348 = CARTESIAN_POINT ( 'NONE',  ( -9.295050272127046043, 37.47773437608393010, -9.295050272127046043 ) ) ;
#13349 = CARTESIAN_POINT ( 'NONE',  ( -13.14518615778179189, 35.04687500108393294, 5.444914386472304635 ) ) ;
#13350 = CARTESIAN_POINT ( 'NONE',  ( 200.6228728715778686, 33.60820312499998863, -13.57481594606304753 ) ) ;
#13351 = EDGE_CURVE ( 'NONE', #27982, #12810, #13928, .T. ) ;
#13352 = LINE ( 'NONE', #9100, #5864 ) ;
#13353 = CARTESIAN_POINT ( 'NONE',  ( 91.00000000000000000, 110.0000000000000000, -45.00000000000000711 ) ) ;
#13354 = CARTESIAN_POINT ( 'NONE',  ( 51.85481384221819923, 34.94765625108392726, -5.444914386472297529 ) ) ;
#13355 = CARTESIAN_POINT ( 'NONE',  ( 99.99999999999995737, -4.458734124999988779, 2.687500001365592528 ) ) ;
#13356 = CARTESIAN_POINT ( 'NONE',  ( -8.312177448680279460E-16, 35.34453125216787583, -13.57481594606304576 ) ) ;
#13357 = ORIENTED_EDGE ( 'NONE', *, *, #16988, .T. ) ;
#13358 = CARTESIAN_POINT ( 'NONE',  ( 104.9999999999999716, 1.449011120738813565E-14, 4.499999999999999112 ) ) ;
#13359 = CARTESIAN_POINT ( 'NONE',  ( 5.622872871577878406, 34.89804687499999147, 13.57481594606304576 ) ) ;
#13360 = CARTESIAN_POINT ( 'NONE',  ( 116.8548138422182063, 37.52734375108393294, -5.444914386472297529 ) ) ;
#13361 = ORIENTED_EDGE ( 'NONE', *, *, #7016, .T. ) ;
#13362 = CARTESIAN_POINT ( 'NONE',  ( 104.4587341249999639, 80.18750000136559208, -1.442382525525748735E-14 ) ) ;
#13363 = DIRECTION ( 'NONE',  ( 0.000000000000000000, 1.000000000000000000, 0.000000000000000000 ) ) ;
#13364 = CARTESIAN_POINT ( 'NONE',  ( 104.9999999999999574, 81.56250000273119838, 2.071067811865462627 ) ) ;
#13365 = CARTESIAN_POINT ( 'NONE',  ( 95.54126587499999346, 93.87499999863439371, 1.846868145590722543 ) ) ;
#13366 = CARTESIAN_POINT ( 'NONE',  ( 0.000000000000000000, -7.395377635281828788, 0.000000000000000000 ) ) ;
#13367 = CARTESIAN_POINT ( 'NONE',  ( 104.3262379212492448, 115.9545556584642867, -47.70000000000001705 ) ) ;
#13368 = CARTESIAN_POINT ( 'NONE',  ( 78.57481594606304043, 39.75976562499999289, 5.622872871577869525 ) ) ;
#13369 = ORIENTED_EDGE ( 'NONE', *, *, #16314, .F. ) ;
#13370 = DIRECTION ( 'NONE',  ( 1.000000000000000000, -0.000000000000000000, 1.224646799147353207E-16 ) ) ;
#13371 = CARTESIAN_POINT ( 'NONE',  ( 104.9999999999999574, -2.071067811865462627, 13.43749999999999822 ) ) ;
#13372 = ORIENTED_EDGE ( 'NONE', *, *, #28182, .T. ) ;
#13373 = CARTESIAN_POINT ( 'NONE',  ( 2.414731522848535132E-15, 33.01289062608393721, 13.14518615778179544 ) ) ;
#13374 = CARTESIAN_POINT ( 'NONE',  ( 5.444914386472302859, 38.61875000108393152, 13.14518615778179189 ) ) ;
#13375 = CARTESIAN_POINT ( 'NONE',  ( 208.5748159460630688, 35.93984375216787441, -1.662435489736055892E-15 ) ) ;
#13376 = VERTEX_POINT ( 'NONE', #22655 ) ;
#13377 = CARTESIAN_POINT ( 'NONE',  ( -13.14518615778179722, 35.74140625108393721, -5.444914386472297529 ) ) ;
#13378 = CARTESIAN_POINT ( 'NONE',  ( -9.598844408820454532, 32.36796874999999574, 9.598844408820459861 ) ) ;
#13379 = CARTESIAN_POINT ( 'NONE',  ( 195.0000000000000000, 38.51953125216787299, -13.57481594606304576 ) ) ;
#13380 = EDGE_LOOP ( 'NONE', ( #12058, #25150, #1968 ) ) ;
#13381 = CARTESIAN_POINT ( 'NONE',  ( 5.444914386472297529, 34.15390625108393863, -13.14518615778179900 ) ) ;
#13382 = CARTESIAN_POINT ( 'NONE',  ( 116.8548138422182205, 34.20351562608393436, 0.000000000000000000 ) ) ;
#13383 = CARTESIAN_POINT ( 'NONE',  ( 55.40115559117954547, 36.13828124999999147, -9.598844408820458085 ) ) ;
#13384 = DIRECTION ( 'NONE',  ( 7.228014483236696740E-18, -0.000000000000000000, 1.000000000000000000 ) ) ;
#13385 = CARTESIAN_POINT ( 'NONE',  ( 101.8468681455906903, 4.458734125000016313, 12.37500000136559208 ) ) ;
#13386 = CARTESIAN_POINT ( 'NONE',  ( -7.228014483236695816E-17, 75.00000000000000000, -9.999999999999998224 ) ) ;
#13387 = AXIS2_PLACEMENT_3D ( 'NONE', #22775, #11910, #27334 ) ;
#13388 = CARTESIAN_POINT ( 'NONE',  ( 98.15313185440923860, 4.458734125000016313, 12.25000000136559208 ) ) ;
#13389 = CARTESIAN_POINT ( 'NONE',  ( 106.5389055433251002, 114.7507929638356785, -45.92500000273119554 ) ) ;
#13390 = CARTESIAN_POINT ( 'NONE',  ( 95.54126587499996504, 1.387778780781445676E-14, 0.6875000013655923059 ) ) ;
#13391 = CARTESIAN_POINT ( 'NONE',  ( 104.9999999999999716, 83.68750000273119838, -2.071067811865491937 ) ) ;
#13392 = CARTESIAN_POINT ( 'NONE',  ( 104.9952793366501567, 103.1245878333314465, -46.92499999726882720 ) ) ;
#13393 = CARTESIAN_POINT ( 'NONE',  ( -5.444914386472297529, 35.84062500108394289, -13.14518615778179900 ) ) ;
#13394 = CARTESIAN_POINT ( 'NONE',  ( 108.0825317499999869, 107.3738262389971538, -52.97499999726881015 ) ) ;
#13395 = ORIENTED_EDGE ( 'NONE', *, *, #14163, .T. ) ;
#13396 = CARTESIAN_POINT ( 'NONE',  ( 97.83688103937538472, 116.6573956140660897, -50.90000000546238113 ) ) ;
#13397 = CARTESIAN_POINT ( 'NONE',  ( 99.99999999999995737, -4.999999999999990230, 12.37500000273118594 ) ) ;
#13398 = LINE ( 'NONE', #2325, #12910 ) ;
#13399 = EDGE_CURVE ( 'NONE', #15490, #291, #25339, .T. ) ;
#13400 = CARTESIAN_POINT ( 'NONE',  ( 181.8548138422181921, 34.94765625108392726, -5.444914386472297529 ) ) ;
#13401 = ORIENTED_EDGE ( 'NONE', *, *, #23321, .F. ) ;
#13402 = FACE_OUTER_BOUND ( 'NONE', #6222, .T. ) ;
#13403 = CARTESIAN_POINT ( 'NONE',  ( 59.68264842252411029, 54.47013368152370560, -15.00000000000000000 ) ) ;
#13404 = EDGE_LOOP ( 'NONE', ( #8649, #10225, #12704, #16841 ) ) ;
#13405 = CARTESIAN_POINT ( 'NONE',  ( 102.4976396683250925, 117.6869444889999841, -51.97500000273119980 ) ) ;
#13406 = VECTOR ( 'NONE', #8063, 1000.000000000000000 ) ;
#13407 = CARTESIAN_POINT ( 'NONE',  ( 5.444914386472297529, 40.30546875108393579, -13.14518615778179900 ) ) ;
#13408 = CARTESIAN_POINT ( 'NONE',  ( 97.50000000000000000, 125.0000000000000000, -9.540979117872439019E-15 ) ) ;
#13409 = CARTESIAN_POINT ( 'NONE',  ( 116.4251840539369454, 31.52460937716787370, -5.622872871577873077 ) ) ;
#13410 = CYLINDRICAL_SURFACE ( 'NONE', #4347, 13.57481594606304398 ) ;
#13412 = AXIS2_PLACEMENT_3D ( 'NONE', #19419, #4042, #28120 ) ;
#13411 = CARTESIAN_POINT ( 'NONE',  ( 95.00000000000000000, 93.43749999726880162, 2.071067811865463959 ) ) ;
#13413 = CARTESIAN_POINT ( 'NONE',  ( 74.29505027212704249, 38.86679687608393863, -9.295050272127046043 ) ) ;
#13414 = CARTESIAN_POINT ( 'NONE',  ( 58.91405578400244281, 54.65299103241780188, -15.00000000000000178 ) ) ;
#13415 = CARTESIAN_POINT ( 'NONE',  ( 181.8548138422181921, 32.07031250108393294, 5.444914386472304635 ) ) ;
#13416 = DIRECTION ( 'NONE',  ( 1.000000000000000000, 0.000000000000000000, -3.469446951953613696E-16 ) ) ;
#13417 = EDGE_LOOP ( 'NONE', ( #27813, #7290, #20410, #25653 ) ) ;
#13418 = VERTEX_POINT ( 'NONE', #18370 ) ;
#13419 = CARTESIAN_POINT ( 'NONE',  ( 9.295050272127047819, 36.28710937608393294, 9.295050272127046043 ) ) ;
#13420 = CARTESIAN_POINT ( 'NONE',  ( 99.99999999999995737, 4.458734125000016313, 12.43750000136559208 ) ) ;
#13421 = CARTESIAN_POINT ( 'NONE',  ( 70.90850774719304184, 36.04503594658366694, 12.68159279706107334 ) ) ;
#13422 = CARTESIAN_POINT ( 'NONE',  ( 102.0710678118654471, 91.06249999726878741, -5.000000000000000000 ) ) ;
#13423 = CARTESIAN_POINT ( 'NONE',  ( 181.8548138422182205, 38.12265625108393863, -5.444914386472297529 ) ) ;
#13424 = ORIENTED_EDGE ( 'NONE', *, *, #17353, .F. ) ;
#13425 = CARTESIAN_POINT ( 'NONE',  ( -8.049105076161786076E-16, 36.58476562608393579, -13.14518615778179544 ) ) ;
#13426 = AXIS2_PLACEMENT_3D ( 'NONE', #5898, #12277, #25683 ) ;
#13427 = CARTESIAN_POINT ( 'NONE',  ( 104.4587341249999923, 90.62499999863439371, -1.846868145590737198 ) ) ;
#13428 = CARTESIAN_POINT ( 'NONE',  ( 208.1451861577818079, 39.51171875108393294, 5.444914386472293977 ) ) ;
#13429 = CARTESIAN_POINT ( 'NONE',  ( 108.0825317499999869, 107.3738262389971538, -52.72499999726881015 ) ) ;
#13430 = ORIENTED_EDGE ( 'NONE', *, *, #118, .F. ) ;
#13431 = CARTESIAN_POINT ( 'NONE',  ( 13.57481594606304753, 35.09648437499998863, -5.622872871577873077 ) ) ;
#13432 = CARTESIAN_POINT ( 'NONE',  ( 5.444914386472302859, 36.83281250108392868, 13.14518615778179189 ) ) ;
#13433 = AXIS2_PLACEMENT_3D ( 'NONE', #7418, #7565, #16259 ) ;
#13434 = ORIENTED_EDGE ( 'NONE', *, *, #9151, .F. ) ;
#13435 = CARTESIAN_POINT ( 'NONE',  ( 139.2950502721270425, 32.51679687608393721, -9.295050272127046043 ) ) ;
#13436 = CARTESIAN_POINT ( 'NONE',  ( 65.00000000000000000, 34.79882812608393294, -13.14518615778179544 ) ) ;
#13437 = CARTESIAN_POINT ( 'NONE',  ( 195.0000000000000000, 36.58476562608393579, -13.14518615778179544 ) ) ;
#13438 = ORIENTED_EDGE ( 'NONE', *, *, #6510, .F. ) ;
#13439 = CARTESIAN_POINT ( 'NONE',  ( 99.14382582708708469, 124.4000000010924794, -2.066987299999998751 ) ) ;
#13440 =( LENGTH_UNIT ( ) NAMED_UNIT ( * ) SI_UNIT ( .MILLI., .METRE. ) );
#13441 = CARTESIAN_POINT ( 'NONE',  ( 94.99999999999997158, -2.071067811865486608, 1.187500002731185722 ) ) ;
#13442 =( BOUNDED_CURVE ( )  B_SPLINE_CURVE ( 2, ( #27415, #9873, #16429, #27696, #5895, #7740, #10136, #5754, #7878 ),
 .UNSPECIFIED., .F., .F. ) 
 B_SPLINE_CURVE_WITH_KNOTS ( ( 3, 2, 2, 2, 3 ),
 ( 0.1041666666666664909, 0.1145833333333332732, 0.1250000000000000833, 0.1354166666666668517, 0.1458333333333336757 ),
 .UNSPECIFIED. ) 
 CURVE ( )  GEOMETRIC_REPRESENTATION_ITEM ( )  RATIONAL_B_SPLINE_CURVE ( ( 1.000000000000001332, 0.9238795325112854062, 1.000000000000000000, 0.9238795325112867385, 1.000000000000000000, 0.9238795325112867385, 1.000000000000000000, 0.9238795325112842960, 1.000000000000002442 ) ) 
 REPRESENTATION_ITEM ( '' )  );
#13443 = CARTESIAN_POINT ( 'NONE',  ( 130.0000000000000000, 39.71015625216787015, 13.57481594606304576 ) ) ;
#13444 = CARTESIAN_POINT ( 'NONE',  ( 97.50236033167492167, 117.6869444889999841, -53.52500000273118985 ) ) ;
#13445 = FACE_OUTER_BOUND ( 'NONE', #19144, .T. ) ;
#13446 = DIRECTION ( 'NONE',  ( 0.000000000000000000, 0.000000000000000000, -1.000000000000000000 ) ) ;
#13447 = CARTESIAN_POINT ( 'NONE',  ( 185.7049497278729575, 39.85898437608393152, -9.295050272127046043 ) ) ;
#13448 = ORIENTED_EDGE ( 'NONE', *, *, #7944, .F. ) ;
#13449 = CARTESIAN_POINT ( 'NONE',  ( 103.1528011352953342, 3.152801135295383084, 4.062500001365592084 ) ) ;
#13450 = AXIS2_PLACEMENT_3D ( 'NONE', #19757, #17615, #26323 ) ;
#13451 = ORIENTED_EDGE ( 'NONE', *, *, #27456, .F. ) ;
#13452 = CARTESIAN_POINT ( 'NONE',  ( 97.93301269999999192, 122.9000000010924936, -0.8561741729129505041 ) ) ;
#13453 = CARTESIAN_POINT ( 'NONE',  ( 99.99999999999995737, 4.458734125000016313, 9.187500001365592084 ) ) ;
#13454 = CARTESIAN_POINT ( 'NONE',  ( 128.9858691739322865, 51.45790058219387220, 14.99999999999793765 ) ) ;
#13455 = CARTESIAN_POINT ( 'NONE',  ( 9.295050272127047819, 34.50117187608393010, 9.295050272127046043 ) ) ;
#13456 = CARTESIAN_POINT ( 'NONE',  ( -5.622872871577816234, 38.56914062716787583, -13.57481594606310260 ) ) ;
#13457 = CARTESIAN_POINT ( 'NONE',  ( 95.54126587499995082, 81.75000000136560629, 1.846868145590724986 ) ) ;
#13458 = CARTESIAN_POINT ( 'NONE',  ( 74.29505027212704249, 36.48554687608393721, -9.295050272127046043 ) ) ;
#13459 = EDGE_CURVE ( 'NONE', #7002, #17147, #24923, .T. ) ;
#13460 = CARTESIAN_POINT ( 'NONE',  ( 181.4251840539369596, 37.82499999999999574, 0.000000000000000000 ) ) ;
#13461 = CARTESIAN_POINT ( 'NONE',  ( 9.295050272127047819, 39.26367187608393294, 9.295050272127046043 ) ) ;
#13462 = DIRECTION ( 'NONE',  ( 0.000000000000000000, 0.000000000000000000, 1.000000000000000000 ) ) ;
#13463 = DIRECTION ( 'NONE',  ( 0.000000000000000000, -1.000000000000000000, 0.000000000000000000 ) ) ;
#13464 = CARTESIAN_POINT ( 'NONE',  ( 104.9999999999999716, 82.43750000000002842, 2.071067811865462627 ) ) ;
#13465 = CARTESIAN_POINT ( 'NONE',  ( 135.6228728715778686, 36.78320312499999289, -13.57481594606304753 ) ) ;
#13466 = ORIENTED_EDGE ( 'NONE', *, *, #8261, .F. ) ;
#13467 = ORIENTED_EDGE ( 'NONE', *, *, #11748, .T. ) ;
#13468 = CARTESIAN_POINT ( 'NONE',  ( 9.598844408820456309, 33.55859375000000000, -9.598844408820458085 ) ) ;
#13469 = CARTESIAN_POINT ( 'NONE',  ( -5.444914386472297529, 38.22187500108393010, -13.14518615778179900 ) ) ;
#13470 = CARTESIAN_POINT ( 'NONE',  ( -9.598844408820454532, 38.81718750216787583, 9.598844408820459861 ) ) ;
#13471 = VECTOR ( 'NONE', #23678, 1000.000000000000000 ) ;
#13472 = CARTESIAN_POINT ( 'NONE',  ( 103.5355339059327093, -3.535533905932726206, 8.500000002731185944 ) ) ;
#13473 = CARTESIAN_POINT ( 'NONE',  ( 139.2950502721270425, 33.90585937608393152, -9.295050272127046043 ) ) ;
#13474 = ADVANCED_FACE ( 'NONE', ( #22797 ), #1841, .T. ) ;
#13475 = CARTESIAN_POINT ( 'NONE',  ( 55.40115559117954547, 33.26093750216787726, 9.598844408820459861 ) ) ;
#13476 = EDGE_CURVE ( 'NONE', #20673, #949, #7095, .T. ) ;
#13477 = VERTEX_POINT ( 'NONE', #6234 ) ;
#13478 = CARTESIAN_POINT ( 'NONE',  ( 11.20653150213565041, 36.00000000000000711, 7.323573988460845285 ) ) ;
#13479 = CARTESIAN_POINT ( 'NONE',  ( 13.57481594606304753, 32.02070312716787015, -5.622872871577873077 ) ) ;
#13480 = CONICAL_SURFACE ( 'NONE', #15771, 17.49444650053485972, 0.5235987755983000369 ) ;
#13481 = CARTESIAN_POINT ( 'NONE',  ( 104.9999999999999574, 2.071067811865491937, 1.562499999999999556 ) ) ;
#13482 = CARTESIAN_POINT ( 'NONE',  ( 102.4976396683250783, 102.3130555110000159, -49.27499999726882152 ) ) ;
#13483 = CARTESIAN_POINT ( 'NONE',  ( 5.622872871577871301, 38.46992187716787015, -13.57481594606304753 ) ) ;
#13484 = CARTESIAN_POINT ( 'NONE',  ( 204.2950502721270425, 33.11210937608393579, -9.295050272127046043 ) ) ;
#13485 = CARTESIAN_POINT ( 'NONE',  ( 99.99999999999995737, 5.000000000000018652, 5.875000002731185056 ) ) ;
#13486 = CARTESIAN_POINT ( 'NONE',  ( 203.7548989532324413, 50.00000000000000000, 10.39041163856606964 ) ) ;
#13487 = ADVANCED_FACE ( 'NONE', ( #23897 ), #26031, .T. ) ;
#13488 = CARTESIAN_POINT ( 'NONE',  ( 130.0000000000000000, 36.38632812608393152, -13.14518615778179544 ) ) ;
#13489 = CARTESIAN_POINT ( 'NONE',  ( 96.46446609406726225, 94.24999999726881583, -3.535533905932738197 ) ) ;
#13490 =( BOUNDED_CURVE ( )  B_SPLINE_CURVE ( 2, ( #11876, #16731, #25430, #27167, #8175, #16447, #21018, #1225, #9889 ),
 .UNSPECIFIED., .F., .T. ) 
 B_SPLINE_CURVE_WITH_KNOTS ( ( 3, 2, 2, 2, 3 ),
 ( 0.7291666666666668517, 0.7395833333333334814, 0.7500000000000001110, 0.7604166666666667407, 0.7708333333333333703 ),
 .UNSPECIFIED. ) 
 CURVE ( )  GEOMETRIC_REPRESENTATION_ITEM ( )  RATIONAL_B_SPLINE_CURVE ( ( 0.9999999999999983347, 0.9238795325112884038, 1.000000000000000000, 0.9238795325112867385, 1.000000000000000000, 0.9238795325112867385, 1.000000000000000000, 0.9238795325112867385, 1.000000000000000000 ) ) 
 REPRESENTATION_ITEM ( '' )  );
#13491 = CARTESIAN_POINT ( 'NONE',  ( 0.000000000000000000, 36.00000000000000000, 0.000000000000000000 ) ) ;
#13492 = CARTESIAN_POINT ( 'NONE',  ( 200.6228728715777834, 36.48554687499999716, 13.57481594606309194 ) ) ;
#13493 = CARTESIAN_POINT ( 'NONE',  ( -5.622872871577873077, 38.46992187499999716, -13.57481594606304753 ) ) ;
#13494 = CARTESIAN_POINT ( 'NONE',  ( 107.0000000000000000, 112.2744378736303190, -45.90000000000000568 ) ) ;
#13495 = AXIS2_PLACEMENT_3D ( 'NONE', #22540, #7705, #1303 ) ;
#13496 = CARTESIAN_POINT ( 'NONE',  ( 9.295050272127046043, 33.31054687608394005, -9.295050272127046043 ) ) ;
#13497 = CARTESIAN_POINT ( 'NONE',  ( 13.14518615778179544, 36.18789062608393436, -1.609821015232357215E-15 ) ) ;
#13498 = CARTESIAN_POINT ( 'NONE',  ( 195.0000000000000000, 34.84843749999999574, 13.57481594606304576 ) ) ;
#13499 = CARTESIAN_POINT ( 'NONE',  ( -5.622872871577873077, 37.27929687716787299, 13.57481594606304753 ) ) ;
#13500 = CARTESIAN_POINT ( 'NONE',  ( 13.57481594606304753, 36.68398437500000142, -5.622872871577873966 ) ) ;
#13501 = LINE ( 'NONE', #561, #7397 ) ;
#13502 = CARTESIAN_POINT ( 'NONE',  ( 55.70494972787295751, 36.48554687608393721, -9.295050272127046043 ) ) ;
#13503 = CARTESIAN_POINT ( 'NONE',  ( 103.1528011352953342, 3.152801135295383084, 1.062500001365592528 ) ) ;
#13504 = CARTESIAN_POINT ( 'NONE',  ( 101.8427817263613235, 123.0000000000000284, -1.695516854503018589 ) ) ;
#13505 = VERTEX_POINT ( 'NONE', #4235 ) ;
#13506 = CARTESIAN_POINT ( 'NONE',  ( 99.99999999999995737, 5.000000000000018652, 4.749999999999999112 ) ) ;
#13507 = CARTESIAN_POINT ( 'NONE',  ( -13.57481594606304753, 36.98164062499999005, -5.622872871577873077 ) ) ;
#13508 = CARTESIAN_POINT ( 'NONE',  ( 143.1451861577818079, 38.71796875108393721, 5.444914386472293977 ) ) ;
#13509 = ADVANCED_FACE ( 'NONE', ( #16913 ), #6095, .T. ) ;
#13510 = ORIENTED_EDGE ( 'NONE', *, *, #24310, .T. ) ;
#13511 = CARTESIAN_POINT ( 'NONE',  ( 103.5355339059327093, 80.62500000000000000, -3.535533905932755072 ) ) ;
#13512 = CARTESIAN_POINT ( 'NONE',  ( -8.312177448680279460E-16, 35.24531249999999716, -13.57481594606304576 ) ) ;
#13513 = CARTESIAN_POINT ( 'NONE',  ( 94.99999999999995737, 80.18750000273121259, 2.071067811865466624 ) ) ;
#13514 = CARTESIAN_POINT ( 'NONE',  ( 97.92893218813452449, 92.31250000000000000, -4.999999999999997335 ) ) ;
#13515 = CARTESIAN_POINT ( 'NONE',  ( 62.10793747869670511, 36.00000000000000000, -13.15766692561476958 ) ) ;
#13516 = EDGE_CURVE ( 'NONE', #20267, #10849, #14627, .T. ) ;
#13517 = CARTESIAN_POINT ( 'NONE',  ( 104.3262379212492448, 104.0454443415356991, -50.30000000000001137 ) ) ;
#13518 = CARTESIAN_POINT ( 'NONE',  ( 51.85481384221820633, 32.07031250108393294, 5.444914386472304635 ) ) ;
#13519 = VERTEX_POINT ( 'NONE', #14762 ) ;
#13520 = AXIS2_PLACEMENT_3D ( 'NONE', #13521, #2436, #22379 ) ;
#13521 = CARTESIAN_POINT ( 'NONE',  ( 99.99999999999998579, 130.0000000000000000, -5.204170427930421283E-15 ) ) ;
#13522 = ADVANCED_FACE ( 'NONE', ( #19199 ), #4376, .T. ) ;
#13523 = CARTESIAN_POINT ( 'NONE',  ( 104.9999999999999574, 2.071067811865491937, 12.56249999999999822 ) ) ;
#13524 = ORIENTED_EDGE ( 'NONE', *, *, #11918, .T. ) ;
#13525 = CARTESIAN_POINT ( 'NONE',  ( -13.14518615778179189, 35.24531250108393721, 5.444914386472304635 ) ) ;
#13526 = CARTESIAN_POINT ( 'NONE',  ( 204.5988444088204403, 34.45156250216787441, -9.598844408820458085 ) ) ;
#13527 = VERTEX_POINT ( 'NONE', #21769 ) ;
#13528 = CARTESIAN_POINT ( 'NONE',  ( -5.444914386472299306, 34.35234375108392868, 13.14518615778179722 ) ) ;
#13529 = DIRECTION ( 'NONE',  ( -5.782411586589357392E-17, -0.000000000000000000, -1.000000000000000000 ) ) ;
#13530 = CARTESIAN_POINT ( 'NONE',  ( 195.0000000000000000, 39.71015625216787015, 13.57481594606304576 ) ) ;
#13531 = CARTESIAN_POINT ( 'NONE',  ( -9.295050272127044266, 33.70742187608393436, 9.295050272127047819 ) ) ;
#13532 = CYLINDRICAL_SURFACE ( 'NONE', #9954, 5.000000000000004441 ) ;
#13533 = CARTESIAN_POINT ( 'NONE',  ( 55.40115559117954547, 34.74921874999999716, 9.598844408820459861 ) ) ;
#13534 =( BOUNDED_CURVE ( )  B_SPLINE_CURVE ( 2, ( #26524, #24096, #9126, #20394, #4572, #26383, #7262, #17533, #19818 ),
 .UNSPECIFIED., .F., .F. ) 
 B_SPLINE_CURVE_WITH_KNOTS ( ( 3, 2, 2, 2, 3 ),
 ( 0.3541666666666666852, 0.3645833333333332593, 0.3749999999999998890, 0.3854166666666665741, 0.3958333333333331483 ),
 .UNSPECIFIED. ) 
 CURVE ( )  GEOMETRIC_REPRESENTATION_ITEM ( )  RATIONAL_B_SPLINE_CURVE ( ( 1.000000000000000000, 0.9238795325112867385, 1.000000000000000000, 0.9238795325112867385, 1.000000000000000000, 0.9238795325112867385, 1.000000000000000000, 0.9238795325112879597, 0.9999999999999987788 ) ) 
 REPRESENTATION_ITEM ( '' )  );
#13535 = PLANE ( 'NONE',  #7768 ) ;
#13536 = CARTESIAN_POINT ( 'NONE',  ( 98.15313185440925281, 4.458734125000016313, 9.500000001365593860 ) ) ;
#13537 = DIRECTION ( 'NONE',  ( 0.000000000000000000, 0.000000000000000000, -1.000000000000000000 ) ) ;
#13538 = CARTESIAN_POINT ( 'NONE',  ( 104.4587341249999639, 1.442382525525748735E-14, 0.9375000013655925279 ) ) ;
#13539 = CARTESIAN_POINT ( 'NONE',  ( 99.99999999999998579, 117.3602355696678501, -53.00000000546238255 ) ) ;
#13540 = DIRECTION ( 'NONE',  ( 0.000000000000000000, 0.000000000000000000, -1.000000000000000000 ) ) ;
#13541 = DIRECTION ( 'NONE',  ( -1.000000000000000000, 0.000000000000000000, 0.000000000000000000 ) ) ;
#13542 = CARTESIAN_POINT ( 'NONE',  ( 102.4976396683250783, 117.6869444889999841, -50.22499999726882436 ) ) ;
#13543 = CARTESIAN_POINT ( 'NONE',  ( -8.049105076161786076E-16, 37.37851562608393863, -13.14518615778179544 ) ) ;
#13544 = CARTESIAN_POINT ( 'NONE',  ( 93.46109445667489979, 105.2492070361643215, -55.67499999726882720 ) ) ;
#13545 = EDGE_LOOP ( 'NONE', ( #8353, #24432, #2068, #26910 ) ) ;
#13546 = CARTESIAN_POINT ( 'NONE',  ( 97.93301270000000613, 123.2000000010924765, 0.8561741729129328515 ) ) ;
#13547 = LINE ( 'NONE', #22270, #252 ) ;
#13548 = CARTESIAN_POINT ( 'NONE',  ( 104.9999999999999858, -2.071067811865442643, 1.437500000000000444 ) ) ;
#13549 = CARTESIAN_POINT ( 'NONE',  ( 181.8548138422182205, 35.79101562608393294, 0.000000000000000000 ) ) ;
#13550 = EDGE_LOOP ( 'NONE', ( #805, #6008 ) ) ;
#13551 = CARTESIAN_POINT ( 'NONE',  ( 95.67376207875072680, 115.9545556584642867, -48.79999999453764303 ) ) ;
#13552 = CARTESIAN_POINT ( 'NONE',  ( 95.54126587499995082, -1.846868145590724986, 9.750000001365593860 ) ) ;
#13553 = ORIENTED_EDGE ( 'NONE', *, *, #9339, .F. ) ;
#13554 = CARTESIAN_POINT ( 'NONE',  ( 93.00000000000000000, 110.0000000000000000, -46.00000000000000711 ) ) ;
#13555 = CARTESIAN_POINT ( 'NONE',  ( 5.444914386472302859, 37.62656250108393863, 13.14518615778179189 ) ) ;
#13556 = CARTESIAN_POINT ( 'NONE',  ( 99.99999999999998579, 124.0000000000000000, -2.499999999999997780 ) ) ;
#13557 = AXIS2_PLACEMENT_3D ( 'NONE', #20367, #9524, #11502 ) ;
#13558 = CARTESIAN_POINT ( 'NONE',  ( 120.7049497278729575, 39.66054687608393436, -9.295050272127046043 ) ) ;
#13559 = DIRECTION ( 'NONE',  ( -0.000000000000000000, 1.000000000000000000, -0.000000000000000000 ) ) ;
#13560 = CARTESIAN_POINT ( 'NONE',  ( 2.414731522848535132E-15, 35.19570312608392726, 13.14518615778179544 ) ) ;
#13561 = CARTESIAN_POINT ( 'NONE',  ( 102.0710678118654613, 95.06249999726880162, -4.999999999999997335 ) ) ;
#13562 = CARTESIAN_POINT ( 'NONE',  ( 55.70494972787295751, 38.46992187608393721, 9.295050272127047819 ) ) ;
#13563 = CARTESIAN_POINT ( 'NONE',  ( 68.11469774553764012, 53.90847045361286405, -15.00000000000000000 ) ) ;
#13564 = CARTESIAN_POINT ( 'NONE',  ( 104.9952793366501709, 116.8754121666685393, -52.07500000273120122 ) ) ;
#13565 = CARTESIAN_POINT ( 'NONE',  ( 208.5748159460630688, 39.80937499999999574, -1.662435489736055892E-15 ) ) ;
#13566 = CARTESIAN_POINT ( 'NONE',  ( 72.06563498876006690, 36.00000000000002842, 11.21307450592250987 ) ) ;
#13567 = CARTESIAN_POINT ( 'NONE',  ( 13.14518615778179900, 36.43593750108392726, -5.444914386472297529 ) ) ;
#13568 = CARTESIAN_POINT ( 'NONE',  ( 99.99999999999995737, -4.458734124999988779, 6.937500001365592972 ) ) ;
#13569 = CARTESIAN_POINT ( 'NONE',  ( 51.85481384221820633, 36.53515625108393294, -5.444914386472297529 ) ) ;
#13570 = DIRECTION ( 'NONE',  ( -5.782411586589357392E-17, 0.000000000000000000, -1.000000000000000000 ) ) ;
#13571 = DIRECTION ( 'NONE',  ( -0.000000000000000000, -1.000000000000000000, -0.000000000000000000 ) ) ;
#13572 = ORIENTED_EDGE ( 'NONE', *, *, #21514, .F. ) ;
#13573 = CARTESIAN_POINT ( 'NONE',  ( 13.14518615778179544, 37.18007812608393436, -1.609821015232357215E-15 ) ) ;
#13574 = CARTESIAN_POINT ( 'NONE',  ( -9.598844408820458085, 36.13828124999999147, -9.598844408820458085 ) ) ;
#13575 = CARTESIAN_POINT ( 'NONE',  ( 189.5550856135277229, 38.51953125108393294, 13.14518615778179722 ) ) ;
#13576 = CARTESIAN_POINT ( 'NONE',  ( 91.91746824999998466, 110.0000000000000000, -49.87499999726882294 ) ) ;
#13577 = AXIS2_PLACEMENT_3D ( 'NONE', #26324, #4661, #18479 ) ;
#13578 = VERTEX_POINT ( 'NONE', #23757 ) ;
#13579 = CARTESIAN_POINT ( 'NONE',  ( 9.598844408820456309, 32.76484374999999716, -9.598844408820458085 ) ) ;
#13580 = CARTESIAN_POINT ( 'NONE',  ( -13.14518615778179189, 35.04687500108393294, 5.444914386472304635 ) ) ;
#13581 = VECTOR ( 'NONE', #4121, 1000.000000000000000 ) ;
#13582 = VERTEX_POINT ( 'NONE', #2246 ) ;
#13583 = ORIENTED_EDGE ( 'NONE', *, *, #21548, .T. ) ;
#13584 = CARTESIAN_POINT ( 'NONE',  ( 120.7049497278729575, 34.30273437608393294, -9.295050272127046043 ) ) ;
#13585 = CARTESIAN_POINT ( 'NONE',  ( 78.14518615778179367, 40.35507812608393863, -1.609821015232357215E-15 ) ) ;
#13586 = CARTESIAN_POINT ( 'NONE',  ( 185.7049497278729575, 35.09648437608393579, -9.295050272127046043 ) ) ;
#13587 = ORIENTED_EDGE ( 'NONE', *, *, #24186, .T. ) ;
#13588 = DIRECTION ( 'NONE',  ( -0.000000000000000000, -0.000000000000000000, -1.000000000000000000 ) ) ;
#13589 = CARTESIAN_POINT ( 'NONE',  ( 9.295050272127046043, 32.31835937608393294, -9.295050272127046043 ) ) ;
#13590 = CARTESIAN_POINT ( 'NONE',  ( 6.944426393311537993, 31.75150625057403175, -11.16113171639042356 ) ) ;
#13591 = DIRECTION ( 'NONE',  ( 0.000000000000000000, 0.000000000000000000, 1.000000000000000000 ) ) ;
#13592 = CARTESIAN_POINT ( 'NONE',  ( 99.99999999999998579, 101.5015231886685712, -50.62500000273119838 ) ) ;
#13593 = CARTESIAN_POINT ( 'NONE',  ( 92.99999999999998579, 110.0000000000000000, -46.49999999453763877 ) ) ;
#13594 = CARTESIAN_POINT ( 'NONE',  ( 9.598844408820459861, 36.53515624999999289, 9.598844408820456309 ) ) ;
#13595 = CARTESIAN_POINT ( 'NONE',  ( 204.2950502721270425, 40.25585937608393294, 9.295050272127046043 ) ) ;
#13596 = ADVANCED_FACE ( 'NONE', ( #10908 ), #23346, .T. ) ;
#13597 = ORIENTED_EDGE ( 'NONE', *, *, #20062, .F. ) ;
#13598 = CARTESIAN_POINT ( 'NONE',  ( 98.15313185440925281, -4.458734124999987891, 5.625000001365591196 ) ) ;
#13599 = ORIENTED_EDGE ( 'NONE', *, *, #20104, .F. ) ;
#13600 = CARTESIAN_POINT ( 'NONE',  ( 101.4615807364564546, 123.4500000010924765, -1.461580736456474794 ) ) ;
#13601 = CARTESIAN_POINT ( 'NONE',  ( 98.15313185440925281, -4.458734124999987891, 6.625000001365592084 ) ) ;
#13602 = CARTESIAN_POINT ( 'NONE',  ( 134.5048870863210766, 51.44650206076644139, 15.00000000000063416 ) ) ;
#13603 = AXIS2_PLACEMENT_3D ( 'NONE', #15112, #2603, #17410 ) ;
#13604 = CARTESIAN_POINT ( 'NONE',  ( 13.14518615778179900, 34.55078125108393294, 5.444914386472293977 ) ) ;
#13605 = FACE_OUTER_BOUND ( 'NONE', #8689, .T. ) ;
#13606 = CARTESIAN_POINT ( 'NONE',  ( 78.57481594606305464, 37.52734375216787299, -1.662435489736055892E-15 ) ) ;
#13607 = CARTESIAN_POINT ( 'NONE',  ( 104.4587341249999781, 92.31249999863440792, -6.938893903907228378E-15 ) ) ;
#13608 = DIRECTION ( 'NONE',  ( 0.000000000000000000, 0.000000000000000000, 1.000000000000000000 ) ) ;
#13609 = CARTESIAN_POINT ( 'NONE',  ( 13.14518615778179544, 36.98164062608393010, -1.609821015232357215E-15 ) ) ;
#13610 = CARTESIAN_POINT ( 'NONE',  ( 94.33688103937534208, 114.1144967660473242, -52.69999999453764161 ) ) ;
#13611 = CARTESIAN_POINT ( 'NONE',  ( -8.772609246135315786, 50.37415326814002725, 15.00000000000326317 ) ) ;
#13612 = CARTESIAN_POINT ( 'NONE',  ( 99.99999999999998579, 91.62499999726880162, 4.999999999999984013 ) ) ;
#13613 = CARTESIAN_POINT ( 'NONE',  ( 130.0000000000000000, 37.62656249999999858, -13.57481594606304576 ) ) ;
#13614 = EDGE_LOOP ( 'NONE', ( #27856, #13721, #6573, #1913 ) ) ;
#13615 = CARTESIAN_POINT ( 'NONE',  ( 96.46446609406721961, -3.535533905932727539, 8.125000000000000000 ) ) ;
#13616 = CARTESIAN_POINT ( 'NONE',  ( 13.14518615778179900, 32.36796875108393579, 5.444914386472293977 ) ) ;
#13617 = CARTESIAN_POINT ( 'NONE',  ( 13.57481594606304576, 33.55859375216787299, -1.662435489736055892E-15 ) ) ;
#13618 =( BOUNDED_CURVE ( )  B_SPLINE_CURVE ( 2, ( #22545, #24534, #17975, #20407, #13684, #22401, #18266, #7417, #26972 ),
 .UNSPECIFIED., .F., .F. ) 
 B_SPLINE_CURVE_WITH_KNOTS ( ( 3, 2, 2, 2, 3 ),
 ( 0.7857142857142856984, 0.7946428571428570953, 0.8035714285714286031, 0.8125000000000000000, 0.8214285714285713969 ),
 .UNSPECIFIED. ) 
 CURVE ( )  GEOMETRIC_REPRESENTATION_ITEM ( )  RATIONAL_B_SPLINE_CURVE ( ( 1.000000000000000000, 0.9238795325112867385, 1.000000000000000000, 0.9238795325112867385, 1.000000000000000000, 0.9238795325112867385, 1.000000000000000000, 0.9238795325112867385, 1.000000000000000000 ) ) 
 REPRESENTATION_ITEM ( '' )  );
#13619 = CARTESIAN_POINT ( 'NONE',  ( 97.92893218813451028, 5.000000000000018652, 10.93750000273118594 ) ) ;
#13620 = CARTESIAN_POINT ( 'NONE',  ( 143.1451861577818079, 32.21914062608393436, -1.609821015232357215E-15 ) ) ;
#13621 = CARTESIAN_POINT ( 'NONE',  ( 74.59884440882045453, 31.87187500216787228, 9.598844408820456309 ) ) ;
#13622 = EDGE_LOOP ( 'NONE', ( #303, #24263, #26956, #11447, #4474, #23542, #7995, #13856, #7964, #1534 ) ) ;
#13623 = CARTESIAN_POINT ( 'NONE',  ( 51.42518405393695957, 37.18007812716787441, 5.622872871577880183 ) ) ;
#13624 = CARTESIAN_POINT ( 'NONE',  ( 2.493653234604083739E-15, 34.15390625216787157, 13.57481594606304576 ) ) ;
#13625 = VECTOR ( 'NONE', #862, 1000.000000000000000 ) ;
#13626 = CARTESIAN_POINT ( 'NONE',  ( 51.42518405393695957, 37.87460937499999147, 5.622872871577880183 ) ) ;
#13627 = CYLINDRICAL_SURFACE ( 'NONE', #25820, 5.000000000000000888 ) ;
#13628 = CARTESIAN_POINT ( 'NONE',  ( -9.598844408820458085, 39.41250000216787441, -9.598844408820458085 ) ) ;
#13629 = CARTESIAN_POINT ( 'NONE',  ( 200.4449143864723055, 34.74921875108394431, -13.14518615778179900 ) ) ;
#13630 = DIRECTION ( 'NONE',  ( 0.000000000000000000, -1.000000000000000000, 0.000000000000000000 ) ) ;
#13631 = CARTESIAN_POINT ( 'NONE',  ( 101.7677669529663547, 124.5069999999781487, 1.767766952966350891 ) ) ;
#13632 = VECTOR ( 'NONE', #13958, 1000.000000000000000 ) ;
#13633 = SURFACE_STYLE_USAGE ( .BOTH. , #9793 ) ;
#13635 = ORIENTED_EDGE ( 'NONE', *, *, #9787, .F. ) ;
#13634 = CARTESIAN_POINT ( 'NONE',  ( 99.99999999999998579, 138.0000000000000000, 11.50000000000001243 ) ) ;
#13636 = FACE_OUTER_BOUND ( 'NONE', #14802, .T. ) ;
#13637 = LINE ( 'NONE', #24771, #17858 ) ;
#13638 = CARTESIAN_POINT ( 'NONE',  ( -9.598844408820458085, 34.55078124999999289, -9.598844408820458085 ) ) ;
#13639 = CARTESIAN_POINT ( 'NONE',  ( 95.67376207875072680, 115.9545556584642867, -54.30000000000001137 ) ) ;
#13640 = CARTESIAN_POINT ( 'NONE',  ( -9.295050272127046043, 35.09648437608393579, -9.295050272127046043 ) ) ;
#13641 = CARTESIAN_POINT ( 'NONE',  ( 13.14518615778179900, 35.44375000108393436, -5.444914386472297529 ) ) ;
#13642 = EDGE_CURVE ( 'NONE', #12810, #4709, #5118, .T. ) ;
#13643 = CARTESIAN_POINT ( 'NONE',  ( 13.14518615778179722, 34.55078125108393294, 5.444914386472293977 ) ) ;
#13644 = CARTESIAN_POINT ( 'NONE',  ( 5.622872871577871301, 36.08867187716787583, -13.57481594606304753 ) ) ;
#13645 = CARTESIAN_POINT ( 'NONE',  ( 13.57481594606304576, 36.63437499999999858, -1.662435489736055892E-15 ) ) ;
#13646 = CARTESIAN_POINT ( 'NONE',  ( 98.15313185440925281, 82.25000000136559208, -4.458734125000016313 ) ) ;
#13647 = CARTESIAN_POINT ( 'NONE',  ( 70.44491438647230552, 34.45156250108393436, 13.14518615778179189 ) ) ;
#13648 = EDGE_CURVE ( 'NONE', #18589, #10173, #15834, .T. ) ;
#13649 = LINE ( 'NONE', #3125, #21232 ) ;
#13650 = CARTESIAN_POINT ( 'NONE',  ( 98.17215415578155557, 123.0000000000000000, 1.711519470631157391 ) ) ;
#13651 = DIRECTION ( 'NONE',  ( -0.000000000000000000, -1.000000000000000000, -0.000000000000000000 ) ) ;
#13652 = CARTESIAN_POINT ( 'NONE',  ( -13.57481594606304576, 33.06249999999999289, 0.000000000000000000 ) ) ;
#13653 = CARTESIAN_POINT ( 'NONE',  ( 130.0000000000000000, 38.17226562608394147, -13.14518615778179544 ) ) ;
#13654 = EDGE_LOOP ( 'NONE', ( #6579, #16496, #7691, #25448 ) ) ;
#13655 = CARTESIAN_POINT ( 'NONE',  ( 104.9999999999999716, 81.50000000000000000, -1.449011120738813565E-14 ) ) ;
#13656 = CARTESIAN_POINT ( 'NONE',  ( 13.57481594606304576, 35.04687499999999289, -1.662435489736055892E-15 ) ) ;
#13657 = CARTESIAN_POINT ( 'NONE',  ( 102.0710678118654329, 83.81250000273119838, -5.000000000000018652 ) ) ;
#13658 = CARTESIAN_POINT ( 'NONE',  ( 99.99999999999998579, 93.75000000000000000, 4.999999999999984013 ) ) ;
#13659 = CYLINDRICAL_SURFACE ( 'NONE', #27455, 13.57481594606304398 ) ;
#13660 = EDGE_CURVE ( 'NONE', #6320, #26359, #17750, .T. ) ;
#13661 = CARTESIAN_POINT ( 'NONE',  ( 97.83688103937535629, 116.6573956140660897, -53.40000000000001990 ) ) ;
#13662 = CARTESIAN_POINT ( 'NONE',  ( 65.00000000000000000, 32.61601562608393579, -13.14518615778179544 ) ) ;
#13663 = EDGE_LOOP ( 'NONE', ( #1834, #20884 ) ) ;
#13664 = CARTESIAN_POINT ( 'NONE',  ( 104.9999999999999716, 1.449011120738813565E-14, 6.499999999999999112 ) ) ;
#13665 = CARTESIAN_POINT ( 'NONE',  ( 99.99999999999995737, 5.000000000000018652, 14.75000000000000000 ) ) ;
#13666 = VERTEX_POINT ( 'NONE', #9628 ) ;
#13667 =( BOUNDED_SURFACE ( )  B_SPLINE_SURFACE ( 1, 2, ( 
 ( #21839, #2452, #21695, #15393, #23825, #4166, #12826, #28106, #15247, #6158, #23548, #10972, #14825, #4305, #23967, #12961, #8570, #25818, #2027, #6293, #24106, #21553, #4025, #12691, #19402, #21416, #19684, #17261, #171, #25962, #14970, #17402, #2169, #13243, #10831, #10695, #4583, #19547, #8853, #1894, #10560, #26247, #21975, #28, #19269, #8710, #27968, #8425, #6567, #17542, #4446, #9137, #26681, #20119, #22399, #17830, #3158, #8998, #5298, #7415, #16110, #22260, #4729, #15965, #19976, #15826, #13819, #26971, #22543, #7129, #9415, #22116, #13682, #15685, #3011, #11682, #11257, #9277, #20405, #2596, #17973, #24531, #13389, #890, #9561, #455, #24679, #18264, #26534, #24815, #5156, #597, #13963, #22688, #11828, #24386, #312, #17690, #4875, #26395, #6991 ),
 ( #5017, #2868, #6849, #15538, #24246, #13539, #2735, #11400, #11539, #20256, #741, #18114, #26828, #7274, #18951, #16402, #1588, #5993, #25100, #25378, #5441, #27112, #12101, #18405, #14528, #7562, #7848, #8122, #23243, #18818, #10243, #5858, #3435, #27660, #16256, #14250, #3851, #1033, #11969, #1305, #24956, #20828, #23379, #14109, #1175, #16817, #20552, #22833, #3720, #14658, #5724, #25514, #18686, #5585, #7708, #9974, #27525, #3299, #20692, #12382, #9704, #27389, #7981, #25233, #16543, #9840, #22971, #18547, #27251, #14389, #23106, #3580, #12237, #20966, #21100, #1449, #10105, #16679, #19233, #21659, #19370, #17508, #8538, #17082, #133, #1862, #4411, #15358, #14793, #2281, #10939, #28073, #19651, #21383, #19091, #24073, #17224, #13066, #8819, #10527, #10662 ) ),
 .UNSPECIFIED., .F., .F., .F. ) 
 B_SPLINE_SURFACE_WITH_KNOTS ( ( 2, 2 ),
 ( 3, 2, 2, 2, 2, 2, 2, 2, 2, 2, 2, 2, 2, 2, 2, 2, 2, 2, 2, 2, 2, 2, 2, 2, 2, 2, 2, 2, 2, 2, 2, 2, 2, 2, 2, 2, 2, 2, 2, 2, 2, 2, 2, 2, 2, 2, 2, 2, 2, 2, 3 ),
 ( 0.000000000000000000, 1.000000000000000000 ),
 ( 0.000000000000000000, 0.02000000000000000042, 0.04000000000000000083, 0.05999999999999999778, 0.08000000000000000167, 0.1000000000000000056, 0.1199999999999999956, 0.1400000000000000133, 0.1600000000000000033, 0.1799999999999999933, 0.2000000000000000111, 0.2200000000000000011, 0.2399999999999999911, 0.2600000000000000089, 0.2800000000000000266, 0.2999999999999999889, 0.3200000000000000067, 0.3400000000000000244, 0.3599999999999999867, 0.3800000000000000044, 0.4000000000000000222, 0.4199999999999999845, 0.4400000000000000022, 0.4600000000000000200, 0.4799999999999999822, 0.5000000000000000000, 0.5200000000000000178, 0.5400000000000000355, 0.5600000000000000533, 0.5799999999999999600, 0.5999999999999999778, 0.6199999999999999956, 0.6400000000000000133, 0.6600000000000000311, 0.6800000000000000488, 0.6999999999999999556, 0.7199999999999999734, 0.7399999999999999911, 0.7600000000000000089, 0.7800000000000000266, 0.8000000000000000444, 0.8199999999999999512, 0.8399999999999999689, 0.8599999999999999867, 0.8800000000000000044, 0.9000000000000000222, 0.9200000000000000400, 0.9399999999999999467, 0.9599999999999999645, 0.9799999999999999822, 1.000000000000000000 ),
 .UNSPECIFIED. ) 
 GEOMETRIC_REPRESENTATION_ITEM ( )  RATIONAL_B_SPLINE_SURFACE ( (
 ( 1.000000000000000000, 0.9510565162951535312, 1.000000000000000000, 0.9510565162951535312, 1.000000000000000000, 0.9510565162951535312, 1.000000000000000000, 0.9510565162951535312, 1.000000000000000000, 0.9510565162951535312, 1.000000000000000000, 0.9510565162951535312, 1.000000000000000000, 0.9510565162951535312, 1.000000000000000000, 0.9510565162951535312, 1.000000000000000000, 0.9510565162951535312, 1.000000000000000000, 0.9510565162951535312, 1.000000000000000000, 0.9510565162951535312, 1.000000000000000000, 0.9510565162951535312, 1.000000000000000000, 0.9510565162951535312, 1.000000000000000000, 0.9510565162951535312, 1.000000000000000000, 0.9510565162951535312, 1.000000000000000000, 0.9510565162951535312, 1.000000000000000000, 0.9510565162951535312, 1.000000000000000000, 0.9510565162951535312, 1.000000000000000000, 0.9510565162951535312, 1.000000000000000000, 0.9510565162951535312, 1.000000000000000000, 0.9510565162951535312, 1.000000000000000000, 0.9510565162951535312, 1.000000000000000000, 0.9510565162951535312, 1.000000000000000000, 0.9510565162951535312, 1.000000000000000000, 0.9510565162951535312, 1.000000000000000000, 0.9510565162951535312, 1.000000000000000000, 0.9510565162951535312, 1.000000000000000000, 0.9510565162951535312, 1.000000000000000000, 0.9510565162951535312, 1.000000000000000000, 0.9510565162951535312, 1.000000000000000000, 0.9510565162951535312, 1.000000000000000000, 0.9510565162951535312, 1.000000000000000000, 0.9510565162951535312, 1.000000000000000000, 0.9510565162951535312, 1.000000000000000000, 0.9510565162951535312, 1.000000000000000000, 0.9510565162951535312, 1.000000000000000000, 0.9510565162951535312, 1.000000000000000000, 0.9510565162951535312, 1.000000000000000000, 0.9510565162951535312, 1.000000000000000000, 0.9510565162951535312, 1.000000000000000000, 0.9510565162951535312, 1.000000000000000000, 0.9510565162951535312, 1.000000000000000000, 0.9510565162951535312, 1.000000000000000000, 0.9510565162951535312, 1.000000000000000000, 0.9510565162951535312, 1.000000000000000000, 0.9510565162951535312, 1.000000000000000000, 0.9510565162951535312, 1.000000000000000000, 0.9510565162951535312, 1.000000000000000000, 0.9510565162951535312, 1.000000000000000000, 0.9510565162951535312, 1.000000000000000000),
 ( 1.000000000000000000, 0.9510565162951535312, 1.000000000000000000, 0.9510565162951535312, 1.000000000000000000, 0.9510565162951535312, 1.000000000000000000, 0.9510565162951535312, 1.000000000000000000, 0.9510565162951535312, 1.000000000000000000, 0.9510565162951535312, 1.000000000000000000, 0.9510565162951535312, 1.000000000000000000, 0.9510565162951535312, 1.000000000000000000, 0.9510565162951535312, 1.000000000000000000, 0.9510565162951535312, 1.000000000000000000, 0.9510565162951535312, 1.000000000000000000, 0.9510565162951535312, 1.000000000000000000, 0.9510565162951535312, 1.000000000000000000, 0.9510565162951535312, 1.000000000000000000, 0.9510565162951535312, 1.000000000000000000, 0.9510565162951535312, 1.000000000000000000, 0.9510565162951535312, 1.000000000000000000, 0.9510565162951535312, 1.000000000000000000, 0.9510565162951535312, 1.000000000000000000, 0.9510565162951535312, 1.000000000000000000, 0.9510565162951535312, 1.000000000000000000, 0.9510565162951535312, 1.000000000000000000, 0.9510565162951535312, 1.000000000000000000, 0.9510565162951535312, 1.000000000000000000, 0.9510565162951535312, 1.000000000000000000, 0.9510565162951535312, 1.000000000000000000, 0.9510565162951535312, 1.000000000000000000, 0.9510565162951535312, 1.000000000000000000, 0.9510565162951535312, 1.000000000000000000, 0.9510565162951535312, 1.000000000000000000, 0.9510565162951535312, 1.000000000000000000, 0.9510565162951535312, 1.000000000000000000, 0.9510565162951535312, 1.000000000000000000, 0.9510565162951535312, 1.000000000000000000, 0.9510565162951535312, 1.000000000000000000, 0.9510565162951535312, 1.000000000000000000, 0.9510565162951535312, 1.000000000000000000, 0.9510565162951535312, 1.000000000000000000, 0.9510565162951535312, 1.000000000000000000, 0.9510565162951535312, 1.000000000000000000, 0.9510565162951535312, 1.000000000000000000, 0.9510565162951535312, 1.000000000000000000, 0.9510565162951535312, 1.000000000000000000, 0.9510565162951535312, 1.000000000000000000, 0.9510565162951535312, 1.000000000000000000, 0.9510565162951535312, 1.000000000000000000, 0.9510565162951535312, 1.000000000000000000, 0.9510565162951535312, 1.000000000000000000, 0.9510565162951535312, 1.000000000000000000, 0.9510565162951535312, 1.000000000000000000) ) ) 
 REPRESENTATION_ITEM ( '' )  SURFACE ( )  );
#13668 = CARTESIAN_POINT ( 'NONE',  ( 5.444914386472302859, 36.23750000108393721, 13.14518615778179189 ) ) ;
#13669 = CARTESIAN_POINT ( 'NONE',  ( 204.5988444088204687, 35.84062500216786873, 9.598844408820456309 ) ) ;
#13670 = CARTESIAN_POINT ( 'NONE',  ( -5.444914386472297529, 31.67343750108393863, -13.14518615778179722 ) ) ;
#13671 = CYLINDRICAL_SURFACE ( 'NONE', #11195, 5.000000000000004441 ) ;
#13672 = EDGE_CURVE ( 'NONE', #8864, #4666, #15479, .T. ) ;
#13673 = CARTESIAN_POINT ( 'NONE',  ( 95.27063293749995410, 84.28125000204839523, -1.387778780781445676E-14 ) ) ;
#13674 = CARTESIAN_POINT ( 'NONE',  ( -13.14518615778179544, 33.60820312608393579, 0.000000000000000000 ) ) ;
#13675 = CARTESIAN_POINT ( 'NONE',  ( 116.8548138422182205, 32.61601562608393579, 0.000000000000000000 ) ) ;
#13676 = CARTESIAN_POINT ( 'NONE',  ( 74.59884440882045453, 32.76484374999999716, -9.598844408820458085 ) ) ;
#13677 = DIRECTION ( 'NONE',  ( -0.000000000000000000, -1.000000000000000000, -0.000000000000000000 ) ) ;
#13678 = CARTESIAN_POINT ( 'NONE',  ( 99.99999999999998579, 90.00000000000000000, 4.999999999999983125 ) ) ;
#13679 = CARTESIAN_POINT ( 'NONE',  ( 99.99999999999995737, 4.458734125000016313, 9.437500001365593860 ) ) ;
#13680 = CARTESIAN_POINT ( 'NONE',  ( 208.4541126562309330, 35.99999999999997158, 0.6772748633551743946 ) ) ;
#13681 = CARTESIAN_POINT ( 'NONE',  ( 104.4587341249999639, 1.442382525525748735E-14, 11.93750000136559208 ) ) ;
#13682 = CARTESIAN_POINT ( 'NONE',  ( 93.46109445667491400, 105.2492070361643215, -46.92500000273119554 ) ) ;
#13683 = CARTESIAN_POINT ( 'NONE',  ( 104.4587341249999923, 92.49999999863442213, 1.846868145590726318 ) ) ;
#13684 = CARTESIAN_POINT ( 'NONE',  ( 99.99999999999995737, 5.000000000000018652, 3.750000000000000000 ) ) ;
#13685 = CARTESIAN_POINT ( 'NONE',  ( 99.99999999999997158, 101.5015231886685712, -53.12499999726883004 ) ) ;
#13686 = CARTESIAN_POINT ( 'NONE',  ( -13.14518615778179900, 34.35234375108393579, -5.444914386472297529 ) ) ;
#13687 = EDGE_CURVE ( 'NONE', #25435, #28031, #19501, .T. ) ;
#13688 = ORIENTED_EDGE ( 'NONE', *, *, #14517, .T. ) ;
#13689 = CARTESIAN_POINT ( 'NONE',  ( 130.0000000000000000, 36.83281249999999574, -13.57481594606304576 ) ) ;
#13690 = LINE ( 'NONE', #13827, #18862 ) ;
#13691 = CARTESIAN_POINT ( 'NONE',  ( -13.57481594606304576, 36.23749999999999005, 0.000000000000000000 ) ) ;
#13692 = TOROIDAL_SURFACE ( 'NONE', #1436, 23.26794919243112503, 1.000000000000000000 ) ;
#13693 = CARTESIAN_POINT ( 'NONE',  ( 208.1451861577817795, 37.03125000108393294, -5.444914386472297529 ) ) ;
#13694 = ORIENTED_EDGE ( 'NONE', *, *, #24287, .T. ) ;
#13695 = CARTESIAN_POINT ( 'NONE',  ( 193.1124712741235783, 53.66306546785489218, -14.99999999999999645 ) ) ;
#13696 = CARTESIAN_POINT ( 'NONE',  ( 95.54126587499996504, 1.387778780781445676E-14, 11.68750000136559208 ) ) ;
#13697 = ORIENTED_EDGE ( 'NONE', *, *, #71, .F. ) ;
#13698 = CARTESIAN_POINT ( 'NONE',  ( 106.5389055433251002, 105.2492070361643215, -52.57500000273119412 ) ) ;
#13699 = CARTESIAN_POINT ( 'NONE',  ( 2.414731522848535132E-15, 35.19570312608392726, 13.14518615778179544 ) ) ;
#13700 = FACE_OUTER_BOUND ( 'NONE', #25790, .T. ) ;
#13701 = CARTESIAN_POINT ( 'NONE',  ( 135.4449143864723055, 37.92421875108392726, -13.14518615778179900 ) ) ;
#13702 = LINE ( 'NONE', #4895, #27573 ) ;
#13703 = CARTESIAN_POINT ( 'NONE',  ( 2.414731522848535132E-15, 36.78320312608393294, 13.14518615778179544 ) ) ;
#13704 = CARTESIAN_POINT ( 'NONE',  ( 103.1528011352953484, 91.43749999863440792, 3.152801135295352886 ) ) ;
#13705 = CARTESIAN_POINT ( 'NONE',  ( 64.67139972343294119, 53.49358765998906051, -15.00000000000000000 ) ) ;
#13706 = CARTESIAN_POINT ( 'NONE',  ( 104.9952793366501709, 116.8754121666685393, -54.07500000273119412 ) ) ;
#13707 = CARTESIAN_POINT ( 'NONE',  ( 195.0000000000000000, 31.82226562608393650, -13.14518615778179544 ) ) ;
#13708 = CARTESIAN_POINT ( 'NONE',  ( 101.7677669529663547, 123.2000000021849502, -1.767766952966370209 ) ) ;
#13709 = ORIENTED_EDGE ( 'NONE', *, *, #18597, .F. ) ;
#13710 = CARTESIAN_POINT ( 'NONE',  ( -13.14518615778179900, 35.93984375108393436, -5.444914386472297529 ) ) ;
#13711 = CARTESIAN_POINT ( 'NONE',  ( 98.15313185440923860, 4.458734125000016313, 8.500000001365592084 ) ) ;
#13712 = CARTESIAN_POINT ( 'NONE',  ( 74.29505027212704249, 38.46992187608393010, 9.295050272127046043 ) ) ;
#13713 = EDGE_CURVE ( 'NONE', #16704, #7323, #7777, .T. ) ;
#13714 = LINE ( 'NONE', #22148, #10601 ) ;
#13715 = CARTESIAN_POINT ( 'NONE',  ( 99.99999999999995737, -4.999999999999990230, 14.24999999999999822 ) ) ;
#13716 = CARTESIAN_POINT ( 'NONE',  ( -5.444914386472299306, 35.34453125108393579, 13.14518615778179722 ) ) ;
#13717 = CARTESIAN_POINT ( 'NONE',  ( 102.0669872999999939, 123.4000000010924936, -0.8561741729129507261 ) ) ;
#13718 = CARTESIAN_POINT ( 'NONE',  ( 94.99999999999995737, 1.387778780781445676E-14, 12.00000000000000000 ) ) ;
#13719 = CARTESIAN_POINT ( 'NONE',  ( 204.2950502721270425, 39.46210937608393721, 9.295050272127046043 ) ) ;
#13720 = CARTESIAN_POINT ( 'NONE',  ( 108.0825317499999869, 112.6261737610028320, -48.77499999726882152 ) ) ;
#13721 = ORIENTED_EDGE ( 'NONE', *, *, #3383, .F. ) ;
#13722 = CARTESIAN_POINT ( 'NONE',  ( 7.171391216998965312, 31.99955315621561525, -11.52591757658528948 ) ) ;
#13723 = CARTESIAN_POINT ( 'NONE',  ( 9.295050272127047819, 32.91367187608393152, 9.295050272127046043 ) ) ;
#13724 = VERTEX_POINT ( 'NONE', #16181 ) ;
#13725 = CARTESIAN_POINT ( 'NONE',  ( 124.5550856135277087, 32.96328125108393436, 13.14518615778179722 ) ) ;
#13726 = CARTESIAN_POINT ( 'NONE',  ( 51.85481384221820633, 31.87187500108393223, 5.444914386472304635 ) ) ;
#13727 = CARTESIAN_POINT ( 'NONE',  ( 195.0000000000000000, 32.61601562608393579, -13.14518615778179544 ) ) ;
#13728 = VERTEX_POINT ( 'NONE', #14178 ) ;
#13729 = CARTESIAN_POINT ( 'NONE',  ( 97.93301270000000613, 123.8000000010924566, 0.8561741729129328515 ) ) ;
#13730 = CARTESIAN_POINT ( 'NONE',  ( 96.46446609406721961, 3.535533905932755072, 9.000000002731184168 ) ) ;
#13731 = CYLINDRICAL_SURFACE ( 'NONE', #5880, 5.000000000000004441 ) ;
#13732 = CARTESIAN_POINT ( 'NONE',  ( 116.4251840539369596, 37.97382812716787726, 5.622872871577880183 ) ) ;
#13733 = CARTESIAN_POINT ( 'NONE',  ( 97.50236033167492167, 102.3130555110000159, -48.72500000273119269 ) ) ;
#13734 = CARTESIAN_POINT ( 'NONE',  ( 96.46446609406721961, -3.535533905932727539, 2.250000002731185500 ) ) ;
#13735 = CARTESIAN_POINT ( 'NONE',  ( -13.57481594606304576, 33.95546875216787441, 0.000000000000000000 ) ) ;
#13736 = CARTESIAN_POINT ( 'NONE',  ( 68.63649624680374473, 51.46815297079189833, 14.99999999999998401 ) ) ;
#13737 = EDGE_LOOP ( 'NONE', ( #19239, #20163, #22579, #19379, #14608, #11415, #1766, #13306, #18232, #25071, #13697, #13438, #15296 ) ) ;
#13738 = CARTESIAN_POINT ( 'NONE',  ( 98.15313185440925281, -4.458734124999987891, 4.625000001365592084 ) ) ;
#13739 = VERTEX_POINT ( 'NONE', #16606 ) ;
#13740 = CARTESIAN_POINT ( 'NONE',  ( -2.849501950123402991E-15, -1.000000000000001998, -23.26794919243113213 ) ) ;
#13741 = CARTESIAN_POINT ( 'NONE',  ( 99.99999999999995737, -4.458734124999988779, 6.687500001365592084 ) ) ;
#13742 = CARTESIAN_POINT ( 'NONE',  ( 136.8735082435767083, 51.14166184781144864, 15.00000000000258638 ) ) ;
#13743 = CARTESIAN_POINT ( 'NONE',  ( -5.444914386472299306, 35.14609375108393152, 13.14518615778179722 ) ) ;
#13744 = DIRECTION ( 'NONE',  ( -0.000000000000000000, -0.000000000000000000, -1.000000000000000000 ) ) ;
#13745 = CARTESIAN_POINT ( 'NONE',  ( 78.14518615778179367, 32.46718750108393436, -5.444914386472297529 ) ) ;
#13746 = CARTESIAN_POINT ( 'NONE',  ( 102.0710678118654329, -4.999999999999989342, 5.312499999999999112 ) ) ;
#13747 = CARTESIAN_POINT ( 'NONE',  ( 104.9952793366501851, 116.8754121666685393, -45.82500000273119412 ) ) ;
#13748 = CARTESIAN_POINT ( 'NONE',  ( -9.295050272127044266, 38.27148437608393294, 9.295050272127047819 ) ) ;
#13749 = LINE ( 'NONE', #25029, #3013 ) ;
#13750 = CARTESIAN_POINT ( 'NONE',  ( 7.114649318941503431, 31.93754143773660203, -11.43472154218138570 ) ) ;
#13751 = DIRECTION ( 'NONE',  ( 0.000000000000000000, 0.000000000000000000, -1.000000000000000000 ) ) ;
#13752 = CARTESIAN_POINT ( 'NONE',  ( 124.3771271284221314, 34.00507812499999716, 13.57481594606304753 ) ) ;
#13753 = ORIENTED_EDGE ( 'NONE', *, *, #27289, .F. ) ;
#13754 = FACE_BOUND ( 'NONE', #10567, .T. ) ;
#13755 = CARTESIAN_POINT ( 'NONE',  ( -13.14518615778179189, 32.86406250108393579, 5.444914386472304635 ) ) ;
#13756 = CARTESIAN_POINT ( 'NONE',  ( -13.57481594606304753, 33.11210937716786873, -5.622872871577873077 ) ) ;
#13757 = CARTESIAN_POINT ( 'NONE',  ( 96.46446609406721961, 3.535533905932755072, 8.000000002731185944 ) ) ;
#13758 = CARTESIAN_POINT ( 'NONE',  ( 143.1451861577818079, 34.65000000108393152, -5.444914386472297529 ) ) ;
#13759 = PRODUCT_DEFINITION_SHAPE ( 'NONE', 'NONE',  #28205 ) ;
#13760 = CARTESIAN_POINT ( 'NONE',  ( 78.14518615778179367, 40.20625000108393010, -5.444914386472297529 ) ) ;
#13761 = EDGE_CURVE ( 'NONE', #16261, #21367, #20435, .T. ) ;
#13762 = CARTESIAN_POINT ( 'NONE',  ( 65.00000000000000000, 52.00000000000000711, -7.517135062566165128E-15 ) ) ;
#13763 = CARTESIAN_POINT ( 'NONE',  ( 13.14518615778179900, 37.72578125108393721, 5.444914386472293977 ) ) ;
#13764 = CARTESIAN_POINT ( 'NONE',  ( 94.99999999999995737, 1.387778780781445676E-14, 0.9999999999999991118 ) ) ;
#13765 = CARTESIAN_POINT ( 'NONE',  ( 104.9952793366501567, 103.1245878333314465, -55.17499999726882720 ) ) ;
#13766 = CARTESIAN_POINT ( 'NONE',  ( 2.493653234604083739E-15, 38.91640625216786731, 13.57481594606304576 ) ) ;
#13767 = CARTESIAN_POINT ( 'NONE',  ( -5.444914386472297529, 40.40468750108393436, -13.14518615778179900 ) ) ;
#13768 = FACE_OUTER_BOUND ( 'NONE', #18178, .T. ) ;
#13769 = CARTESIAN_POINT ( 'NONE',  ( 104.3262379212492448, 104.0454443415356991, -52.30000000000001137 ) ) ;
#13770 = AXIS2_PLACEMENT_3D ( 'NONE', #20482, #24892, #5089 ) ;
#13771 =( NAMED_UNIT ( * ) PLANE_ANGLE_UNIT ( ) SI_UNIT ( $, .RADIAN. ) );
#13772 = DIRECTION ( 'NONE',  ( -0.000000000000000000, -1.000000000000000000, -0.000000000000000000 ) ) ;
#13773 = DIRECTION ( 'NONE',  ( -0.000000000000000000, -1.000000000000000000, -0.000000000000000000 ) ) ;
#13774 = CARTESIAN_POINT ( 'NONE',  ( 99.99999999999998579, 123.3000000021849587, -2.499999999999997780 ) ) ;
#13775 = CARTESIAN_POINT ( 'NONE',  ( -8.312177448680279460E-16, 32.86406249999999574, -13.57481594606304576 ) ) ;
#13776 = CARTESIAN_POINT ( 'NONE',  ( 6.944423797152706079, 31.55306878032414986, -11.16113333171310451 ) ) ;
#13777 = CARTESIAN_POINT ( 'NONE',  ( -8.049105076161786076E-16, 34.99726562608393721, -13.14518615778179544 ) ) ;
#13778 = CARTESIAN_POINT ( 'NONE',  ( 5.444914386472302859, 37.62656250108393863, 13.14518615778179189 ) ) ;
#13779 = CARTESIAN_POINT ( 'NONE',  ( 2.414731522848535132E-15, 34.40195312608393152, 13.14518615778179544 ) ) ;
#13780 = CARTESIAN_POINT ( 'NONE',  ( -13.57481594606304753, 34.69960937716787441, -5.622872871577873077 ) ) ;
#13781 = CARTESIAN_POINT ( 'NONE',  ( 104.9999999999999858, -2.071067811865442643, 4.562500002731185944 ) ) ;
#13782 = CARTESIAN_POINT ( 'NONE',  ( 95.54126587499996504, 82.43750000136559208, -1.387778780781445676E-14 ) ) ;
#13783 = CARTESIAN_POINT ( 'NONE',  ( 55.70494972787295751, 31.72304687608393081, -9.295050272127046043 ) ) ;
#13784 = CARTESIAN_POINT ( 'NONE',  ( 99.99999999999998579, 118.4984768113314004, -51.87500000273118417 ) ) ;
#13785 = CARTESIAN_POINT ( 'NONE',  ( 114.9999999999999858, 95.00000000000000000, 14.99999999999999289 ) ) ;
#13786 =( BOUNDED_CURVE ( )  B_SPLINE_CURVE ( 2, ( #21805, #24218, #21661, #4270, #2138, #4026, #4552, #6960, #22227 ),
 .UNSPECIFIED., .F., .F. ) 
 B_SPLINE_CURVE_WITH_KNOTS ( ( 3, 2, 2, 2, 3 ),
 ( 0.4166666666666667407, 0.4583333333333334259, 0.5000000000000002220, 0.5416666666666668517, 0.5833333333333337034 ),
 .UNSPECIFIED. ) 
 CURVE ( )  GEOMETRIC_REPRESENTATION_ITEM ( )  RATIONAL_B_SPLINE_CURVE ( ( 0.9999999999999998890, 0.9238795325112868495, 1.000000000000000000, 0.9238795325112867385, 1.000000000000000000, 0.9238795325112867385, 1.000000000000000000, 0.9238795325112861834, 1.000000000000000666 ) ) 
 REPRESENTATION_ITEM ( '' )  );
#13787 = ORIENTED_EDGE ( 'NONE', *, *, #22894, .F. ) ;
#13788 = CARTESIAN_POINT ( 'NONE',  ( 99.99999999999998579, 124.3500000010924822, -2.066987299999998751 ) ) ;
#13789 = CARTESIAN_POINT ( 'NONE',  ( 7.171391216998965312, 31.99955315621561525, -11.52591757658528948 ) ) ;
#13790 = CARTESIAN_POINT ( 'NONE',  ( 135.4449143864723055, 35.74140625108393721, -13.14518615778179900 ) ) ;
#13791 = ORIENTED_EDGE ( 'NONE', *, *, #27439, .F. ) ;
#13792 = CARTESIAN_POINT ( 'NONE',  ( 102.0710678118654329, 81.31250000000000000, 4.999999999999989342 ) ) ;
#13793 = CARTESIAN_POINT ( 'NONE',  ( 97.92893218813448186, 94.31250000000001421, -4.999999999999948486 ) ) ;
#13794 = CARTESIAN_POINT ( 'NONE',  ( 96.46446609406721961, 80.00000000273119838, -3.535533905932755072 ) ) ;
#13795 = CARTESIAN_POINT ( 'NONE',  ( 95.00000000000000000, 90.50000000000000000, -7.551217303480904118E-15 ) ) ;
#13796 = CARTESIAN_POINT ( 'NONE',  ( 78.57481594606305464, 39.11484375216787157, -1.662435489736055892E-15 ) ) ;
#13797 = CARTESIAN_POINT ( 'NONE',  ( 106.5389055433250860, 105.2492070361643215, -48.82499999726882578 ) ) ;
#13798 = CARTESIAN_POINT ( 'NONE',  ( 70.44491438647230552, 32.56640625108394005, -13.14518615778179900 ) ) ;
#13799 = CARTESIAN_POINT ( 'NONE',  ( 59.55508561352770158, 36.13828125108393152, 13.14518615778179722 ) ) ;
#13800 = ORIENTED_EDGE ( 'NONE', *, *, #3260, .T. ) ;
#13801 = CARTESIAN_POINT ( 'NONE',  ( 130.0000000000000000, -7.395377635281828788, -1.503427012513233026E-14 ) ) ;
#13802 = CARTESIAN_POINT ( 'NONE',  ( 94.99999999999995737, 2.071067811865491048, 12.93749999999999822 ) ) ;
#13803 = EDGE_CURVE ( 'NONE', #5516, #19665, #23344, .T. ) ;
#13804 = EDGE_LOOP ( 'NONE', ( #26142, #3363, #1524, #18698 ) ) ;
#13805 = CARTESIAN_POINT ( 'NONE',  ( 5.444914386472297529, 37.32890625108393579, -13.14518615778179900 ) ) ;
#13806 = CARTESIAN_POINT ( 'NONE',  ( 195.0000000000000000, 33.36015625216786873, 13.57481594606304576 ) ) ;
#13807 = ORIENTED_EDGE ( 'NONE', *, *, #22040, .T. ) ;
#13808 = CARTESIAN_POINT ( 'NONE',  ( -5.444914386472299306, 32.76484375108393010, 13.14518615778179722 ) ) ;
#13809 = CARTESIAN_POINT ( 'NONE',  ( 2.493653234604083739E-15, 32.46718749999999432, 13.57481594606304576 ) ) ;
#13810 = CARTESIAN_POINT ( 'NONE',  ( 104.9999999999999716, -2.071067811865462627, 3.437499999999999556 ) ) ;
#13811 = CARTESIAN_POINT ( 'NONE',  ( -9.295050272127046043, 36.68398437608393436, -9.295050272127046043 ) ) ;
#13812 = DIRECTION ( 'NONE',  ( 5.782411586589357392E-17, 0.000000000000000000, 1.000000000000000000 ) ) ;
#13813 = CARTESIAN_POINT ( 'NONE',  ( 99.99999999999998579, 92.56249999863440792, -4.458734124999994997 ) ) ;
#13814 =( LENGTH_UNIT ( ) NAMED_UNIT ( * ) SI_UNIT ( .MILLI., .METRE. ) );
#13815 = CARTESIAN_POINT ( 'NONE',  ( 99.99999999999998579, 110.0000000000000000, -145.0000000000000284 ) ) ;
#13816 = CARTESIAN_POINT ( 'NONE',  ( 99.99999999999995737, 4.458734125000016313, 5.437500001365592972 ) ) ;
#13817 = CARTESIAN_POINT ( 'NONE',  ( 98.23223304703363112, 123.2999999999999972, -1.767766952966370209 ) ) ;
#13818 = CARTESIAN_POINT ( 'NONE',  ( 96.84719886470459471, 3.152801135295383084, 10.31250000136559208 ) ) ;
#13819 = CARTESIAN_POINT ( 'NONE',  ( 97.50236033167492167, 117.6869444889999841, -47.52500000273119696 ) ) ;
#13820 = DIRECTION ( 'NONE',  ( 0.000000000000000000, 0.000000000000000000, 1.000000000000000000 ) ) ;
#13821 = DIRECTION ( 'NONE',  ( 0.000000000000000000, 0.000000000000000000, 1.000000000000000000 ) ) ;
#13822 = CARTESIAN_POINT ( 'NONE',  ( 195.0000000000000000, 50.00000000000000000, -2.255140518769849538E-14 ) ) ;
#13823 = CARTESIAN_POINT ( 'NONE',  ( -8.049105076161786076E-16, 31.82226562608393650, -13.14518615778179544 ) ) ;
#13824 = ORIENTED_EDGE ( 'NONE', *, *, #21691, .F. ) ;
#13825 = DIRECTION ( 'NONE',  ( -0.000000000000000000, -1.000000000000000000, -0.000000000000000000 ) ) ;
#13826 = EDGE_CURVE ( 'NONE', #6897, #7134, #26897, .T. ) ;
#13827 = CARTESIAN_POINT ( 'NONE',  ( -9.396418828207704684E-17, 78.00000000000000000, -12.99999999999999822 ) ) ;
#13828 =( BOUNDED_SURFACE ( )  B_SPLINE_SURFACE ( 1, 2, ( 
 ( #308, #449, #11533, #4724, #24673, #8993, #22112, #26389, #9132, #17825, #26530, #15681, #14244, #25370, #12094, #18680, #16103, #18811, #22825, #18945, #24809, #5579, #20821, #5436, #7556, #27518, #14521, #18541, #5850, #22965, #7841, #1028, #22683, #23236, #10099, #5716, #3713, #12230, #27245, #12375, #3153 ),
 ( #5292, #27105, #16394, #13956, #7701, #10235, #11822, #16251, #21093, #7409, #9698, #20958, #1582, #1299, #20545, #3427, #3293, #11963, #25092, #14382, #18398, #24949, #1441, #14103, #9967, #23098, #27382, #16535, #20685, #1168, #9834, #25227, #3574, #7974, #16673, #10518, #21796, #4260, #27927, #12921, #17073 ) ),
 .UNSPECIFIED., .F., .F., .F. ) 
 B_SPLINE_SURFACE_WITH_KNOTS ( ( 2, 2 ),
 ( 3, 2, 2, 2, 2, 2, 2, 2, 2, 2, 2, 2, 2, 2, 2, 2, 2, 2, 2, 2, 3 ),
 ( 0.000000000000000000, 1.000000000000000000 ),
 ( 0.000000000000000000, 0.04166666666666666435, 0.08333333333333332871, 0.1250000000000000000, 0.1666666666666666574, 0.2083333333333333426, 0.2500000000000000000, 0.2916666666666666852, 0.3333333333333333148, 0.3750000000000000000, 0.4166666666666666852, 0.4583333333333333148, 0.5000000000000000000, 0.5416666666666666297, 0.5833333333333333703, 0.6250000000000000000, 0.6666666666666666297, 0.7083333333333333703, 0.7500000000000000000, 0.7916666666666666297, 0.8333333333333333703 ),
 .UNSPECIFIED. ) 
 GEOMETRIC_REPRESENTATION_ITEM ( )  RATIONAL_B_SPLINE_SURFACE ( (
 ( 1.000000000000000000, 0.9238795325112867385, 1.000000000000000000, 0.9238795325112867385, 1.000000000000000000, 0.9238795325112867385, 1.000000000000000000, 0.9238795325112867385, 1.000000000000000000, 0.9238795325112867385, 1.000000000000000000, 0.9238795325112867385, 1.000000000000000000, 0.9238795325112867385, 1.000000000000000000, 0.9238795325112867385, 1.000000000000000000, 0.9238795325112867385, 1.000000000000000000, 0.9238795325112867385, 1.000000000000000000, 0.9238795325112867385, 1.000000000000000000, 0.9238795325112867385, 1.000000000000000000, 0.9238795325112867385, 1.000000000000000000, 0.9238795325112867385, 1.000000000000000000, 0.9238795325112867385, 1.000000000000000000, 0.9238795325112867385, 1.000000000000000000, 0.9238795325112867385, 1.000000000000000000, 0.9238795325112867385, 1.000000000000000000, 0.9238795325112867385, 1.000000000000000000, 0.9238795325112867385, 1.000000000000000000),
 ( 1.000000000000000000, 0.9238795325112867385, 1.000000000000000000, 0.9238795325112867385, 1.000000000000000000, 0.9238795325112867385, 1.000000000000000000, 0.9238795325112867385, 1.000000000000000000, 0.9238795325112867385, 1.000000000000000000, 0.9238795325112867385, 1.000000000000000000, 0.9238795325112867385, 1.000000000000000000, 0.9238795325112867385, 1.000000000000000000, 0.9238795325112867385, 1.000000000000000000, 0.9238795325112867385, 1.000000000000000000, 0.9238795325112867385, 1.000000000000000000, 0.9238795325112867385, 1.000000000000000000, 0.9238795325112867385, 1.000000000000000000, 0.9238795325112867385, 1.000000000000000000, 0.9238795325112867385, 1.000000000000000000, 0.9238795325112867385, 1.000000000000000000, 0.9238795325112867385, 1.000000000000000000, 0.9238795325112867385, 1.000000000000000000, 0.9238795325112867385, 1.000000000000000000, 0.9238795325112867385, 1.000000000000000000) ) ) 
 REPRESENTATION_ITEM ( '' )  SURFACE ( )  );
#13829 = CARTESIAN_POINT ( 'NONE',  ( 185.7049497278729575, 37.27929687608393294, -9.295050272127046043 ) ) ;
#13830 = ORIENTED_EDGE ( 'NONE', *, *, #16950, .T. ) ;
#13831 = EDGE_CURVE ( 'NONE', #18466, #12623, #16754, .T. ) ;
#13832 = CARTESIAN_POINT ( 'NONE',  ( 201.1165602397168186, 54.66944451632673463, -15.00000000000000178 ) ) ;
#13833 = CARTESIAN_POINT ( 'NONE',  ( 99.99999999999995737, -4.458734124999988779, 10.93750000136559208 ) ) ;
#13834 = ORIENTED_EDGE ( 'NONE', *, *, #11586, .T. ) ;
#13835 = CARTESIAN_POINT ( 'NONE',  ( 102.4976396683250925, 117.6869444889999841, -53.97500000273119980 ) ) ;
#13836 = CARTESIAN_POINT ( 'NONE',  ( -13.14518615778179900, 37.32890625108393579, -5.444914386472297529 ) ) ;
#13837 = CARTESIAN_POINT ( 'NONE',  ( 98.96446609406727646, 124.0499999999999972, -2.499999999999997780 ) ) ;
#13838 = CYLINDRICAL_SURFACE ( 'NONE', #25786, 13.57481594606304398 ) ;
#13839 = EDGE_CURVE ( 'NONE', #18823, #18668, #3783, .T. ) ;
#13840 = CARTESIAN_POINT ( 'NONE',  ( 143.1451861577818079, 38.51953125108393294, 5.444914386472293977 ) ) ;
#13841 = CARTESIAN_POINT ( 'NONE',  ( -13.14518615778179189, 36.83281250108393579, 5.444914386472304635 ) ) ;
#13842 = CARTESIAN_POINT ( 'NONE',  ( 5.444914386472297529, 36.33671875108394289, -13.14518615778179900 ) ) ;
#13843 = AXIS2_PLACEMENT_3D ( 'NONE', #12009, #4142, #22733 ) ;
#13844 = CARTESIAN_POINT ( 'NONE',  ( 98.15313185440925281, 94.24999999863439371, 4.458734124999979898 ) ) ;
#13845 = CARTESIAN_POINT ( 'NONE',  ( -13.57481594606304753, 36.28710937716787299, -5.622872871577872189 ) ) ;
#13846 = CARTESIAN_POINT ( 'NONE',  ( 106.5389055433251002, 105.2492070361643215, -48.57500000273119412 ) ) ;
#13847 = ADVANCED_FACE ( 'NONE', ( #19015, #27866 ), #21588, .T. ) ;
#13848 = CARTESIAN_POINT ( 'NONE',  ( 77.66784425494549282, 35.99999999999997868, 4.396229039744254941 ) ) ;
#13849 = CARTESIAN_POINT ( 'NONE',  ( 9.295050272127047819, 34.69960937608393436, 9.295050272127046043 ) ) ;
#13850 = CARTESIAN_POINT ( 'NONE',  ( 96.84719886470459471, -3.152801135295355994, 8.812500001365592084 ) ) ;
#13851 = CARTESIAN_POINT ( 'NONE',  ( 65.00000000000000000, 38.37070312608393152, 13.14518615778179544 ) ) ;
#13852 = CARTESIAN_POINT ( 'NONE',  ( 102.4999999999999858, 124.6000000000000085, -9.847140817659276890E-15 ) ) ;
#13853 = CARTESIAN_POINT ( 'NONE',  ( 196.1371678245420753, 35.99999999999999289, 13.09590655363592582 ) ) ;
#13854 = ORIENTED_EDGE ( 'NONE', *, *, #7706, .T. ) ;
#13855 = CARTESIAN_POINT ( 'NONE',  ( 13.14518615778179722, 34.74921875108395142, 5.444914386472293977 ) ) ;
#13856 = ORIENTED_EDGE ( 'NONE', *, *, #24116, .F. ) ;
#13857 = CARTESIAN_POINT ( 'NONE',  ( 101.0355339059327378, 122.9500000021849502, 2.499999999999977796 ) ) ;
#13858 = CARTESIAN_POINT ( 'NONE',  ( 101.8468681455907330, 92.37499999863440792, 4.458734124999980786 ) ) ;
#13859 = CARTESIAN_POINT ( 'NONE',  ( 181.8548138422182205, 36.83281250108393579, 5.444914386472304635 ) ) ;
#13860 = CARTESIAN_POINT ( 'NONE',  ( 106.5389055433250860, 105.2492070361643215, -49.07499999726882578 ) ) ;
#13861 = ORIENTED_EDGE ( 'NONE', *, *, #21226, .F. ) ;
#13862 = AXIS2_PLACEMENT_3D ( 'NONE', #6936, #2401, #11200 ) ;
#13863 = CARTESIAN_POINT ( 'NONE',  ( -8.312177448680279460E-16, 32.07031249999999289, -13.57481594606304576 ) ) ;
#13864 = CARTESIAN_POINT ( 'NONE',  ( -9.295050272127044266, 32.71523437608393436, 9.295050272127047819 ) ) ;
#13865 = ORIENTED_EDGE ( 'NONE', *, *, #11572, .F. ) ;
#13866 = CARTESIAN_POINT ( 'NONE',  ( 139.2950502721270425, 34.69960937608393436, 9.295050272127046043 ) ) ;
#13867 = CARTESIAN_POINT ( 'NONE',  ( 78.14518615778180788, 40.40468750108393436, -5.444914386472297529 ) ) ;
#13868 = CARTESIAN_POINT ( 'NONE',  ( 181.8548138422182205, 33.60820312608393579, 0.000000000000000000 ) ) ;
#13869 = VERTEX_POINT ( 'NONE', #6470 ) ;
#13870 = CARTESIAN_POINT ( 'NONE',  ( 103.5355339059327093, -3.535533905932726206, 13.37500000000000000 ) ) ;
#13871 = CARTESIAN_POINT ( 'NONE',  ( -0.8765262653614457333, 51.45968077934941221, -14.99999999999999289 ) ) ;
#13872 = LINE ( 'NONE', #9326, #19972 ) ;
#13873 = ADVANCED_FACE ( 'NONE', ( #10456 ), #25578, .F. ) ;
#13874 = CARTESIAN_POINT ( 'NONE',  ( 143.5748159460630404, 39.16445312716788152, -5.622872871577873077 ) ) ;
#13875 = CARTESIAN_POINT ( 'NONE',  ( 95.00472066334981491, 103.1245878333314465, -50.82500000273119412 ) ) ;
#13876 = CYLINDRICAL_SURFACE ( 'NONE', #26996, 13.57481594606304398 ) ;
#13877 = CYLINDRICAL_SURFACE ( 'NONE', #14149, 5.000000000000004441 ) ;
#13878 = CARTESIAN_POINT ( 'NONE',  ( 181.8548138422181921, 39.90859375108394147, -5.444914386472297529 ) ) ;
#13879 = CIRCLE ( 'NONE', #13426, 13.57481594606304398 ) ;
#13880 = ORIENTED_EDGE ( 'NONE', *, *, #5505, .T. ) ;
#13881 =( LENGTH_UNIT ( ) NAMED_UNIT ( * ) SI_UNIT ( .MILLI., .METRE. ) );
#13882 = CARTESIAN_POINT ( 'NONE',  ( 104.4587341249999781, 1.846868145590750299, 6.000000001365591196 ) ) ;
#13883 = ORIENTED_EDGE ( 'NONE', *, *, #9595, .F. ) ;
#13884 = CARTESIAN_POINT ( 'NONE',  ( -9.598844408820458085, 35.44375000216787441, -9.598844408820458085 ) ) ;
#13885 = CARTESIAN_POINT ( 'NONE',  ( 101.8468681455906903, 4.458734125000016313, 6.125000001365591196 ) ) ;
#13886 = CARTESIAN_POINT ( 'NONE',  ( 133.8030543732469653, 54.09082899096448926, 14.99999999999996447 ) ) ;
#13887 = CARTESIAN_POINT ( 'NONE',  ( -7.068365687998699798, 35.99999999999997158, 11.09140360074105658 ) ) ;
#13888 = CARTESIAN_POINT ( 'NONE',  ( 51.85481384221820633, 32.86406250108393579, 5.444914386472304635 ) ) ;
#13889 = DIRECTION ( 'NONE',  ( 1.156482317317871478E-16, 0.000000000000000000, 1.000000000000000000 ) ) ;
#13890 = DIRECTION ( 'NONE',  ( -1.000000000000000000, 0.000000000000000000, 0.000000000000000000 ) ) ;
#13891 = CIRCLE ( 'NONE', #5731, 11.57481594606304576 ) ;
#13892 = CYLINDRICAL_SURFACE ( 'NONE', #20303, 13.57481594606304398 ) ;
#13893 = CARTESIAN_POINT ( 'NONE',  ( -8.758334392354218068, 50.00000000000000000, 10.38725784494356930 ) ) ;
#13894 = CARTESIAN_POINT ( 'NONE',  ( 143.5748159460630688, 40.65273437499999432, -5.622872871577873966 ) ) ;
#13895 = CARTESIAN_POINT ( 'NONE',  ( 130.0000000000000000, 35.64218749999999147, 13.57481594606304576 ) ) ;
#13896 = EDGE_LOOP ( 'NONE', ( #17959, #6972, #13709, #1795 ) ) ;
#13897 = ORIENTED_EDGE ( 'NONE', *, *, #11067, .F. ) ;
#13898 = DIRECTION ( 'NONE',  ( 1.000000000000000000, 0.000000000000000000, -1.156482317317871725E-16 ) ) ;
#13899 = CARTESIAN_POINT ( 'NONE',  ( 9.295050272127046043, 34.89804687608393863, -9.295050272127046043 ) ) ;
#13900 = CARTESIAN_POINT ( 'NONE',  ( 5.622872871577871301, 32.91367187716787157, -13.57481594606304753 ) ) ;
#13901 = CARTESIAN_POINT ( 'NONE',  ( 96.46446609406721961, -3.535533905932727539, 11.25000000273118594 ) ) ;
#13902 = CARTESIAN_POINT ( 'NONE',  ( 124.5550856135277087, 32.46718750108393436, -13.14518615778179900 ) ) ;
#13903 = CARTESIAN_POINT ( 'NONE',  ( 55.70494972787295751, 39.66054687608393436, -9.295050272127046043 ) ) ;
#13904 = CARTESIAN_POINT ( 'NONE',  ( 102.0710678118654897, 80.68750000000002842, -4.999999999999968914 ) ) ;
#13905 = CARTESIAN_POINT ( 'NONE',  ( -13.14518615778179189, 39.01562500108393294, 5.444914386472304635 ) ) ;
#13906 = CARTESIAN_POINT ( 'NONE',  ( -9.295050272127044266, 32.91367187608393152, 9.295050272127047819 ) ) ;
#13907 = CARTESIAN_POINT ( 'NONE',  ( 97.92893218813451028, -4.999999999999989342, 3.187499999999999556 ) ) ;
#13908 = CARTESIAN_POINT ( 'NONE',  ( 93.46109445667489979, 114.7507929638356785, -54.07499999726881867 ) ) ;
#13909 = CARTESIAN_POINT ( 'NONE',  ( 84.99999999999998579, 120.0000000000000000, -45.00000000000000711 ) ) ;
#13910 = CARTESIAN_POINT ( 'NONE',  ( 185.7049497278729575, 32.71523437608393436, 9.295050272127047819 ) ) ;
#13911 = CIRCLE ( 'NONE', #3924, 23.00000000000001421 ) ;
#13912 = CARTESIAN_POINT ( 'NONE',  ( -5.622872871577873966, 31.42539062716787157, -13.57481594606304753 ) ) ;
#13913 = CARTESIAN_POINT ( 'NONE',  ( 99.99999999999998579, 124.0069999999781487, -2.499999999999997780 ) ) ;
#13914 = CARTESIAN_POINT ( 'NONE',  ( 102.0669872999999939, 123.3000000010924850, 0.8561741729129311862 ) ) ;
#13915 = CARTESIAN_POINT ( 'NONE',  ( 132.0072970100684984, 35.99999999999997158, -13.40042260803736696 ) ) ;
#13916 = CARTESIAN_POINT ( 'NONE',  ( 124.3771271284222877, 36.18789062716787441, -13.57481594606318254 ) ) ;
#13917 = CARTESIAN_POINT ( 'NONE',  ( 104.9999999999999716, 1.449011120738813565E-14, 2.625000002731185500 ) ) ;
#13918 = CARTESIAN_POINT ( 'NONE',  ( 13.57481594606304753, 35.09648437499998863, -5.622872871577873077 ) ) ;
#13919 = CARTESIAN_POINT ( 'NONE',  ( -9.295050272127046043, 35.89023437608393152, -9.295050272127046043 ) ) ;
#13920 = CARTESIAN_POINT ( 'NONE',  ( 13.14518615778179900, 32.16953125108393152, 5.444914386472293977 ) ) ;
#13921 = CARTESIAN_POINT ( 'NONE',  ( 13.14518615778179544, 35.39414062608393152, -1.609821015232357215E-15 ) ) ;
#13922 = CARTESIAN_POINT ( 'NONE',  ( 13.57481594606304576, 37.52734375216787299, -1.662435489736055892E-15 ) ) ;
#13923 = LINE ( 'NONE', #27072, #6728 ) ;
#13924 = CARTESIAN_POINT ( 'NONE',  ( 99.99999999999995737, 83.18750000136560629, -4.458734125000016313 ) ) ;
#13925 = CARTESIAN_POINT ( 'NONE',  ( 51.85481384221820633, 40.75195312608393294, 0.000000000000000000 ) ) ;
#13926 = EDGE_CURVE ( 'NONE', #2259, #24967, #8189, .T. ) ;
#13927 = FACE_OUTER_BOUND ( 'NONE', #18643, .T. ) ;
#13928 = LINE ( 'NONE', #18786, #9574 ) ;
#13929 = AXIS2_PLACEMENT_3D ( 'NONE', #7734, #16284, #27550 ) ;
#13930 = CARTESIAN_POINT ( 'NONE',  ( 98.53841926354351699, 123.8500000010924680, 1.461580736456455920 ) ) ;
#13931 = CARTESIAN_POINT ( 'NONE',  ( -13.57481594606304753, 33.80664062500000000, -5.622872871577873077 ) ) ;
#13932 = CARTESIAN_POINT ( 'NONE',  ( 120.7049497278729575, 33.70742187608393436, 9.295050272127047819 ) ) ;
#13933 = VERTEX_POINT ( 'NONE', #8048 ) ;
#13934 = CARTESIAN_POINT ( 'NONE',  ( 0.000000000000000000, 40.99999999999999289, -13.57481594606304576 ) ) ;
#13935 = CARTESIAN_POINT ( 'NONE',  ( 107.0000000000000000, 112.2744378736303190, -47.90000000000001990 ) ) ;
#13936 = CARTESIAN_POINT ( 'NONE',  ( 94.99999999999995737, 80.12500000273119838, -1.387778780781445676E-14 ) ) ;
#13937 = VECTOR ( 'NONE', #12283, 1000.000000000000000 ) ;
#13938 = CARTESIAN_POINT ( 'NONE',  ( 103.5355339059327235, 94.12500000000000000, -3.535533905932738197 ) ) ;
#13939 = CARTESIAN_POINT ( 'NONE',  ( 70.62287287157786864, 39.26367187716787299, -13.57481594606304753 ) ) ;
#13940 = CARTESIAN_POINT ( 'NONE',  ( 99.99999999999997158, 117.3602355696678501, -53.50000000000001421 ) ) ;
#13941 = CARTESIAN_POINT ( 'NONE',  ( 200.4449143864723055, 40.20625000108394431, 13.14518615778179189 ) ) ;
#13942 = CARTESIAN_POINT ( 'NONE',  ( 9.598844408820456309, 38.42031250216787441, -9.598844408820458085 ) ) ;
#13943 = ORIENTED_EDGE ( 'NONE', *, *, #19889, .F. ) ;
#13944 = CARTESIAN_POINT ( 'NONE',  ( 183.8544531269043887, 35.99999999999999289, -7.260818043106919362 ) ) ;
#13945 = CARTESIAN_POINT ( 'NONE',  ( 104.9999999999999716, 1.449011120738813565E-14, 12.49999999999999822 ) ) ;
#13946 = EDGE_LOOP ( 'NONE', ( #24613, #3203, #8315, #26982 ) ) ;
#13947 = CARTESIAN_POINT ( 'NONE',  ( -9.295050272127046043, 35.89023437608393152, -9.295050272127046043 ) ) ;
#13948 = CARTESIAN_POINT ( 'NONE',  ( 189.5550856135277229, 39.61093750108393152, -13.14518615778179900 ) ) ;
#13949 =( BOUNDED_CURVE ( )  B_SPLINE_CURVE ( 2, ( #14945, #23524, #12668, #20975, #18960, #21392, #23115, #16826, #6001 ),
 .UNSPECIFIED., .F., .T. ) 
 B_SPLINE_CURVE_WITH_KNOTS ( ( 3, 2, 2, 2, 3 ),
 ( 0.8958333333333335924, 0.9062500000000002220, 0.9166666666666667407, 0.9270833333333334814, 0.9375000000000000000 ),
 .UNSPECIFIED. ) 
 CURVE ( )  GEOMETRIC_REPRESENTATION_ITEM ( )  RATIONAL_B_SPLINE_CURVE ( ( 0.9999999999999983347, 0.9238795325112884038, 1.000000000000000000, 0.9238795325112867385, 1.000000000000000000, 0.9238795325112867385, 1.000000000000000000, 0.9238795325112867385, 1.000000000000000000 ) ) 
 REPRESENTATION_ITEM ( '' )  );
#13950 = CARTESIAN_POINT ( 'NONE',  ( -9.295050272127044266, 34.30273437608393294, 9.295050272127047819 ) ) ;
#13951 = DIRECTION ( 'NONE',  ( -0.000000000000000000, -1.000000000000000000, -0.000000000000000000 ) ) ;
#13952 = DIRECTION ( 'NONE',  ( -0.000000000000000000, 1.000000000000000000, -0.000000000000000000 ) ) ;
#13953 = CARTESIAN_POINT ( 'NONE',  ( 9.295050272127047819, 33.11210937608393579, 9.295050272127046043 ) ) ;
#13954 = CARTESIAN_POINT ( 'NONE',  ( 99.99999999999995737, 1.387778780781445676E-14, 34.79898987322334136 ) ) ;
#13955 = CARTESIAN_POINT ( 'NONE',  ( 104.4587341249999781, 91.31249999863440792, -6.938893903907228378E-15 ) ) ;
#13956 = CARTESIAN_POINT ( 'NONE',  ( 98.96446609406727646, 124.8500000000000085, -2.499999999999997780 ) ) ;
#13957 = DIRECTION ( 'NONE',  ( 0.000000000000000000, 0.000000000000000000, 1.000000000000000000 ) ) ;
#13958 = DIRECTION ( 'NONE',  ( -0.000000000000000000, -1.000000000000000000, -0.000000000000000000 ) ) ;
#13959 = CARTESIAN_POINT ( 'NONE',  ( 98.15313185440925281, 4.458734125000016313, 6.500000001365592084 ) ) ;
#13960 = CARTESIAN_POINT ( 'NONE',  ( 185.8198241863519513, 55.00000000000000000, -15.00000000000000000 ) ) ;
#13961 = EDGE_CURVE ( 'NONE', #26002, #26108, #17296, .T. ) ;
#13962 = CARTESIAN_POINT ( 'NONE',  ( 104.4587341249999781, 1.846868145590750521, 12.00000000136559208 ) ) ;
#13963 = CARTESIAN_POINT ( 'NONE',  ( 93.46109445667491400, 105.2492070361643215, -44.92500000273119554 ) ) ;
#13964 = CARTESIAN_POINT ( 'NONE',  ( 96.84719886470463734, 91.18749999863440792, 3.152801135295351997 ) ) ;
#13965 = DIRECTION ( 'NONE',  ( 0.000000000000000000, 0.000000000000000000, -1.000000000000000000 ) ) ;
#13966 = CARTESIAN_POINT ( 'NONE',  ( 99.99999999999997158, 118.4984768113314146, -54.12499999726881583 ) ) ;
#13967 = CARTESIAN_POINT ( 'NONE',  ( 9.295050272127047819, 33.90585937608393863, 9.295050272127046043 ) ) ;
#13968 = ORIENTED_EDGE ( 'NONE', *, *, #10318, .F. ) ;
#13969 = CARTESIAN_POINT ( 'NONE',  ( 5.622872871577863307, 39.75976562716787299, 13.57481594606306174 ) ) ;
#13970 = CARTESIAN_POINT ( 'NONE',  ( 97.50000000000000000, 123.5000000021849615, -9.540979117872439019E-15 ) ) ;
#13971 = CARTESIAN_POINT ( 'NONE',  ( 189.5550856135277229, 35.14609375108393152, 13.14518615778179722 ) ) ;
#13972 = ORIENTED_EDGE ( 'NONE', *, *, #3586, .T. ) ;
#13973 = LINE ( 'NONE', #3168, #5370 ) ;
#13974 = CARTESIAN_POINT ( 'NONE',  ( 96.84719886470459471, 3.152801135295383084, 12.56250000136559208 ) ) ;
#13975 = ORIENTED_EDGE ( 'NONE', *, *, #21526, .T. ) ;
#13976 = CARTESIAN_POINT ( 'NONE',  ( 104.9952793366501851, 116.8754121666685393, -52.07500000273120122 ) ) ;
#13977 = CARTESIAN_POINT ( 'NONE',  ( 9.295050272127046043, 37.87460937608393152, -9.295050272127046043 ) ) ;
#13978 = CARTESIAN_POINT ( 'NONE',  ( 181.4251840539369596, 38.76757812716787299, 5.622872871577880183 ) ) ;
#13979 = DIRECTION ( 'NONE',  ( -0.000000000000000000, 1.000000000000000000, -0.000000000000000000 ) ) ;
#13980 = CARTESIAN_POINT ( 'NONE',  ( 139.2950502721270425, 37.67617187608393436, 9.295050272127046043 ) ) ;
#13981 = CARTESIAN_POINT ( 'NONE',  ( 5.444914386472302859, 37.82500000108392868, 13.14518615778179189 ) ) ;
#13982 = CARTESIAN_POINT ( 'NONE',  ( -13.14518615778179189, 34.25312500108393010, 5.444914386472304635 ) ) ;
#13983 = ADVANCED_FACE ( 'NONE', ( #16880 ), #1929, .F. ) ;
#13984 = CARTESIAN_POINT ( 'NONE',  ( 99.99999999999998579, 90.81249999863440792, -4.458734124999994997 ) ) ;
#13985 = CIRCLE ( 'NONE', #10339, 4.999999999999989342 ) ;
#13986 = VECTOR ( 'NONE', #7143, 1000.000000000000000 ) ;
#13987 = CARTESIAN_POINT ( 'NONE',  ( 69.06258354057162308, 50.00000000116031629, -12.98908657125264554 ) ) ;
#13988 = CARTESIAN_POINT ( 'NONE',  ( 97.50236033167492167, 102.3130555110000159, -52.97500000273119980 ) ) ;
#13989 = ORIENTED_EDGE ( 'NONE', *, *, #1814, .T. ) ;
#13990 = CARTESIAN_POINT ( 'NONE',  ( 65.00000000000000000, 50.00000000000000000, -7.517135062566165128E-15 ) ) ;
#13991 = CARTESIAN_POINT ( 'NONE',  ( -13.14518615778179900, 37.52734375108393294, -5.444914386472297529 ) ) ;
#13992 = CARTESIAN_POINT ( 'NONE',  ( 103.1528011352953342, 3.152801135295383084, 7.312500001365592084 ) ) ;
#13993 = ADVANCED_FACE ( 'NONE', ( #6062 ), #6329, .T. ) ;
#13994 = CARTESIAN_POINT ( 'NONE',  ( 51.85481384221821344, 36.63437500108393863, 5.444914386472304635 ) ) ;
#13995 = PRODUCT_DEFINITION_SHAPE ( 'NONE', 'NONE',  #9428 ) ;
#13996 = CARTESIAN_POINT ( 'NONE',  ( 104.9999999999999716, 2.071067811865491937, 6.687500002731185056 ) ) ;
#13997 = CARTESIAN_POINT ( 'NONE',  ( 100.0000000000000000, 110.0000000000000000, -55.00000000000000711 ) ) ;
#13998 = CARTESIAN_POINT ( 'NONE',  ( 208.1451861577818079, 36.93203125108394147, 5.444914386472293977 ) ) ;
#13999 = ADVANCED_FACE ( 'NONE', ( #12859 ), #15002, .F. ) ;
#14000 = CARTESIAN_POINT ( 'NONE',  ( 13.14518615778179722, 36.33671875108393579, 5.444914386472293977 ) ) ;
#14001 =( BOUNDED_CURVE ( )  B_SPLINE_CURVE ( 2, ( #27624, #14490, #16777, #14623, #23341, #21202, #10344, #19051, #27760 ),
 .UNSPECIFIED., .F., .F. ) 
 B_SPLINE_CURVE_WITH_KNOTS ( ( 3, 2, 2, 2, 3 ),
 ( 0.3958333333333331483, 0.4062499999999999445, 0.4166666666666667407, 0.4270833333333335369, 0.4375000000000003331 ),
 .UNSPECIFIED. ) 
 CURVE ( )  GEOMETRIC_REPRESENTATION_ITEM ( )  RATIONAL_B_SPLINE_CURVE ( ( 1.000000000000001110, 0.9238795325112855172, 1.000000000000000000, 0.9238795325112867385, 1.000000000000000000, 0.9238795325112867385, 1.000000000000000000, 0.9238795325112842960, 1.000000000000002442 ) ) 
 REPRESENTATION_ITEM ( '' )  );
#14002 = CARTESIAN_POINT ( 'NONE',  ( 98.96446609406727646, 123.3500000021849701, -2.499999999999997780 ) ) ;
#14003 = CARTESIAN_POINT ( 'NONE',  ( 104.4587341249999781, 92.56249999863440792, -6.938893903907228378E-15 ) ) ;
#14004 = CARTESIAN_POINT ( 'NONE',  ( 200.4449143864723055, 39.41250000108393436, 13.14518615778179189 ) ) ;
#14005 = CARTESIAN_POINT ( 'NONE',  ( 91.91746824999997045, 107.3738262389971538, -49.77499999726881441 ) ) ;
#14006 = CARTESIAN_POINT ( 'NONE',  ( -13.57481594606304753, 33.01289062500000426, -5.622872871577873077 ) ) ;
#14007 = CARTESIAN_POINT ( 'NONE',  ( -5.444914386472299306, 35.14609375108393152, 13.14518615778179722 ) ) ;
#14008 = EDGE_LOOP ( 'NONE', ( #3479, #3448, #9881, #6459 ) ) ;
#14009 = CARTESIAN_POINT ( 'NONE',  ( 87.00000000000000000, 0.000000000000000000, 8.673617379884035472E-16 ) ) ;
#14010 = CARTESIAN_POINT ( 'NONE',  ( 139.1801758136479918, 55.00000000000000000, -15.00000000000000000 ) ) ;
#14011 = CARTESIAN_POINT ( 'NONE',  ( 99.14382582708708469, 123.0000000010924879, -2.066987299999998751 ) ) ;
#14012 = ADVANCED_FACE ( 'NONE', ( #3923 ), #15143, .F. ) ;
#14013 = CARTESIAN_POINT ( 'NONE',  ( 189.5550856135277229, 33.75703125108393721, 13.14518615778179722 ) ) ;
#14014 = ORIENTED_EDGE ( 'NONE', *, *, #20419, .F. ) ;
#14015 = CARTESIAN_POINT ( 'NONE',  ( 104.9999999999999574, 2.071067811865501263, 10.68750000273118594 ) ) ;
#14016 = CARTESIAN_POINT ( 'NONE',  ( 8.772609246137605510, 50.37415326814473104, -14.99999999999999822 ) ) ;
#14017 = CARTESIAN_POINT ( 'NONE',  ( 55.70494972787295751, 35.69179687608393436, -9.295050272127046043 ) ) ;
#14018 = CARTESIAN_POINT ( 'NONE',  ( 103.5355339059327093, -3.535533905932726206, 1.500000002731184612 ) ) ;
#14019 = CARTESIAN_POINT ( 'NONE',  ( 124.3771271284221314, 36.18789062716787441, -13.57481594606304753 ) ) ;
#14020 = CARTESIAN_POINT ( 'NONE',  ( 65.00000000000000000, 39.61093749999999147, 13.57481594606304576 ) ) ;
#14021 = CARTESIAN_POINT ( 'NONE',  ( 105.0000000000000000, 110.0000000000000000, -43.00000000000000000 ) ) ;
#14022 = CARTESIAN_POINT ( 'NONE',  ( 181.8548138422181921, 40.70234375108393721, -5.444914386472297529 ) ) ;
#14023 = EDGE_CURVE ( 'NONE', #18276, #5473, #27337, .T. ) ;
#14024 = ORIENTED_EDGE ( 'NONE', *, *, #17684, .T. ) ;
#14025 = CARTESIAN_POINT ( 'NONE',  ( 104.4587341249999781, 1.846868145590750299, 5.000000001365592972 ) ) ;
#14026 = EDGE_LOOP ( 'NONE', ( #6738, #18079, #17091, #24750, #15568, #22022, #27670, #18458, #25149, #11975, #2295, #26333, #18411, #6101, #19529 ) ) ;
#14027 = CARTESIAN_POINT ( 'NONE',  ( -13.14917398115171743, 36.00000000000000711, -1.058935892997135975 ) ) ;
#14028 = CARTESIAN_POINT ( 'NONE',  ( 98.15313185440925281, 4.458734125000016313, 9.250000001365593860 ) ) ;
#14029 = CARTESIAN_POINT ( 'NONE',  ( 208.5748159460630688, 38.27148437500000711, -5.622872871577873966 ) ) ;
#14030 = AXIS2_PLACEMENT_3D ( 'NONE', #17813, #24229, #434 ) ;
#14031 = CARTESIAN_POINT ( 'NONE',  ( 65.00000000000000000, -7.395377635281828788, -7.517135062566165128E-15 ) ) ;
#14032 = CARTESIAN_POINT ( 'NONE',  ( 78.57481594606305464, 37.57695312716787583, -5.622872871577873966 ) ) ;
#14033 = DIRECTION ( 'NONE',  ( 0.000000000000000000, 1.000000000000000000, 0.000000000000000000 ) ) ;
#14034 = CARTESIAN_POINT ( 'NONE',  ( 97.50236033167492167, 102.3130555110000159, -46.72500000273119269 ) ) ;
#14035 = CARTESIAN_POINT ( 'NONE',  ( 2.493653234604083739E-15, 39.71015625216787015, 13.57481594606304576 ) ) ;
#14036 = ADVANCED_FACE ( 'NONE', ( #12441 ), #25443, .F. ) ;
#14037 = AXIS2_PLACEMENT_3D ( 'NONE', #15642, #24341, #15916 ) ;
#14038 = DIRECTION ( 'NONE',  ( -0.000000000000000000, 1.000000000000000000, -0.000000000000000000 ) ) ;
#14039 = CARTESIAN_POINT ( 'NONE',  ( -4.062583540577167973, 50.00000000116096288, 12.98908657125208777 ) ) ;
#14040 = CARTESIAN_POINT ( 'NONE',  ( 55.40115559117954547, 40.90078124999999432, -9.598844408820458085 ) ) ;
#14041 = CARTESIAN_POINT ( 'NONE',  ( 143.5748159460630688, 35.04687499999999289, -1.662435489736055892E-15 ) ) ;
#14042 = EDGE_CURVE ( 'NONE', #7134, #26108, #2064, .T. ) ;
#14043 = ORIENTED_EDGE ( 'NONE', *, *, #25412, .F. ) ;
#14044 = CARTESIAN_POINT ( 'NONE',  ( 92.99999999999998579, 110.0000000000000000, -51.00000000000000711 ) ) ;
#14045 = SHAPE_REPRESENTATION ( 'Vacuum Distribution Tubing Harness', ( #26844 ), #12238 ) ;
#14046 = CARTESIAN_POINT ( 'NONE',  ( 2.414731522848535132E-15, 33.01289062608393721, 13.14518615778179544 ) ) ;
#14047 = CARTESIAN_POINT ( 'NONE',  ( -13.57481594606304576, 34.00507812716787015, 5.622872871577880183 ) ) ;
#14048 = CARTESIAN_POINT ( 'NONE',  ( 97.92893218813451028, -4.999999999999989342, 7.312500002731185944 ) ) ;
#14049 = CARTESIAN_POINT ( 'NONE',  ( 143.1451861577818079, 34.60039062608392868, -1.609821015232357215E-15 ) ) ;
#14050 = CARTESIAN_POINT ( 'NONE',  ( 65.00000000000000000, 39.95820312608393010, 13.14518615778179544 ) ) ;
#14051 = EDGE_LOOP ( 'NONE', ( #20783, #19, #16689, #14223 ) ) ;
#14052 = CARTESIAN_POINT ( 'NONE',  ( 94.99999999999995737, 1.387778780781445676E-14, 15.00000000000000000 ) ) ;
#14053 = CARTESIAN_POINT ( 'NONE',  ( 9.295050272127046043, 39.46210937608393010, -9.295050272127046043 ) ) ;
#14054 = CARTESIAN_POINT ( 'NONE',  ( 13.14518615778179722, 33.26093750108393721, -5.444914386472297529 ) ) ;
#14055 = DIRECTION ( 'NONE',  ( -0.000000000000000000, 1.000000000000000000, -0.000000000000000000 ) ) ;
#14056 = CARTESIAN_POINT ( 'NONE',  ( 91.91746824999997045, 107.3738262389971680, -53.77499999726882862 ) ) ;
#14057 = EDGE_LOOP ( 'NONE', ( #22845, #23586, #12470, #15228 ) ) ;
#14058 = CARTESIAN_POINT ( 'NONE',  ( 5.622872871577871301, 40.05742187716786873, -13.57481594606304753 ) ) ;
#14059 = CARTESIAN_POINT ( 'NONE',  ( 103.5355339059327093, 82.75000000273119838, -3.535533905932755072 ) ) ;
#14060 = CARTESIAN_POINT ( 'NONE',  ( 143.0420085811497302, 36.00000000000001421, -3.640726557254540197 ) ) ;
#14061 = DIRECTION ( 'NONE',  ( -0.000000000000000000, -1.000000000000000000, -0.000000000000000000 ) ) ;
#14062 =( GEOMETRIC_REPRESENTATION_CONTEXT ( 3 ) GLOBAL_UNCERTAINTY_ASSIGNED_CONTEXT ( ( #21825 ) ) GLOBAL_UNIT_ASSIGNED_CONTEXT ( ( #8294, #14832, #10138 ) ) REPRESENTATION_CONTEXT ( 'NONE', 'WORKASPACE' ) );
#14063 = CARTESIAN_POINT ( 'NONE',  ( 116.8975291782781198, 36.00000000000000000, -1.608626461598027246 ) ) ;
#14064 = CARTESIAN_POINT ( 'NONE',  ( 92.99999999999997158, 107.7255621263696810, -47.89999999999999147 ) ) ;
#14065 = DIRECTION ( 'NONE',  ( -0.000000000000000000, 4.625929269271485914E-16, 1.000000000000000000 ) ) ;
#14066 = CARTESIAN_POINT ( 'NONE',  ( -5.622872871577873077, 34.79882812499998579, 13.57481594606304753 ) ) ;
#14067 = CARTESIAN_POINT ( 'NONE',  ( -9.598844408820458085, 32.96328124999999432, -9.598844408820458085 ) ) ;
#14068 = CARTESIAN_POINT ( 'NONE',  ( 9.295050272127046043, 34.10429687608393579, -9.295050272127046043 ) ) ;
#14069 = CARTESIAN_POINT ( 'NONE',  ( -9.295050272127044266, 33.50898437608393010, 9.295050272127047819 ) ) ;
#14070 = CARTESIAN_POINT ( 'NONE',  ( 181.4251840539369596, 32.26874999999999716, 0.000000000000000000 ) ) ;
#14071 = EDGE_CURVE ( 'NONE', #24017, #11839, #28004, .T. ) ;
#14072 = CARTESIAN_POINT ( 'NONE',  ( -9.598844408820454532, 35.64218750216787868, 9.598844408820459861 ) ) ;
#14073 = LINE ( 'NONE', #17934, #22693 ) ;
#14074 = CARTESIAN_POINT ( 'NONE',  ( 104.9999999999999716, 1.449011120738813565E-14, 34.79898987322334136 ) ) ;
#14075 = CARTESIAN_POINT ( 'NONE',  ( 78.14518615778179367, 32.16953125108393152, 5.444914386472293977 ) ) ;
#14076 = CARTESIAN_POINT ( 'NONE',  ( 108.0825317500000153, 110.0000000000000000, -54.37500000273119838 ) ) ;
#14077 = CARTESIAN_POINT ( 'NONE',  ( 84.99999999999998579, 125.0000000000000000, 14.99999999999999112 ) ) ;
#14078 = CARTESIAN_POINT ( 'NONE',  ( 99.99999999999998579, 123.5500000010924850, -2.066987299999998751 ) ) ;
#14079 = DIRECTION ( 'NONE',  ( -0.000000000000000000, 1.000000000000000000, 0.000000000000000000 ) ) ;
#14080 = CARTESIAN_POINT ( 'NONE',  ( 107.0000000000000000, 110.0000000000000000, -47.49999999453763877 ) ) ;
#14081 = CARTESIAN_POINT ( 'NONE',  ( 135.4449143864723055, 34.94765625108394147, -13.14518615778179900 ) ) ;
#14082 = ORIENTED_EDGE ( 'NONE', *, *, #3331, .F. ) ;
#14083 = CARTESIAN_POINT ( 'NONE',  ( 104.9999999999999574, 80.56250000000004263, -2.071067811865491937 ) ) ;
#14084 = MECHANICAL_DESIGN_GEOMETRIC_PRESENTATION_REPRESENTATION (  '', ( #18176 ), #22749 ) ;
#14085 = CARTESIAN_POINT ( 'NONE',  ( 200.6228728715778686, 36.88242187716787157, -13.57481594606304753 ) ) ;
#14086 = CARTESIAN_POINT ( 'NONE',  ( 103.1528011352953342, 82.06250000136559208, -3.152801135295383084 ) ) ;
#14087 = CARTESIAN_POINT ( 'NONE',  ( 95.00000000000000000, 91.50000000000000000, -7.551217303480904118E-15 ) ) ;
#14088 = AXIS2_PLACEMENT_3D ( 'NONE', #15971, #13825, #22549 ) ;
#14089 = CARTESIAN_POINT ( 'NONE',  ( 65.00000000000000000, 39.71015625216787015, 13.57481594606304576 ) ) ;
#14090 = CARTESIAN_POINT ( 'NONE',  ( 108.0825317499999869, 112.6261737610028320, -46.52499999726882152 ) ) ;
#14091 = CARTESIAN_POINT ( 'NONE',  ( 189.5550856135277229, 40.10703125108393152, 13.14518615778179722 ) ) ;
#14092 = CARTESIAN_POINT ( 'NONE',  ( 5.622872871577871301, 40.05742187716786873, -13.57481594606304753 ) ) ;
#14093 = ORIENTED_EDGE ( 'NONE', *, *, #8997, .T. ) ;
#14094 = CARTESIAN_POINT ( 'NONE',  ( 102.0710678118654329, 5.000000000000018652, 10.68749999999999822 ) ) ;
#14095 = ORIENTED_EDGE ( 'NONE', *, *, #15422, .T. ) ;
#14096 = CARTESIAN_POINT ( 'NONE',  ( 13.14518615778179900, 36.33671875108394289, 5.444914386472293977 ) ) ;
#14097 = CARTESIAN_POINT ( 'NONE',  ( 200.6228728715778686, 32.61601562716786873, 13.57481594606304576 ) ) ;
#14098 = CARTESIAN_POINT ( 'NONE',  ( -9.295050272127046043, 34.10429687608393579, -9.295050272127046043 ) ) ;
#14099 = DIRECTION ( 'NONE',  ( 0.000000000000000000, -0.000000000000000000, 1.000000000000000000 ) ) ;
#14100 = CARTESIAN_POINT ( 'NONE',  ( -5.444914386472297529, 31.87187500108393223, -13.14518615778179900 ) ) ;
#14101 = CARTESIAN_POINT ( 'NONE',  ( 104.3262379212492590, 104.0454443415356991, -49.80000000546237970 ) ) ;
#14102 = CARTESIAN_POINT ( 'NONE',  ( 95.54126587499999346, 90.74999999863439371, -1.846868145590737864 ) ) ;
#14103 = CARTESIAN_POINT ( 'NONE',  ( 102.4999999999999716, 123.8500000000000085, -1.035533905932742638 ) ) ;
#14104 = DIRECTION ( 'NONE',  ( 1.000000000000000000, 0.000000000000000000, 0.000000000000000000 ) ) ;
#14105 = CARTESIAN_POINT ( 'NONE',  ( 74.59884440882045453, 36.83281250216787583, -9.598844408820458085 ) ) ;
#14106 = CARTESIAN_POINT ( 'NONE',  ( 104.4587341249999781, -1.846868145590721655, 7.125000001365592084 ) ) ;
#14107 = CARTESIAN_POINT ( 'NONE',  ( 104.3262379212492590, 115.9545556584642867, -53.20000000546237118 ) ) ;
#14108 = CARTESIAN_POINT ( 'NONE',  ( 101.8468681455907046, -4.458734124999987891, 8.750000001365592084 ) ) ;
#14109 = CARTESIAN_POINT ( 'NONE',  ( 104.3262379212492590, 115.9545556584642867, -49.20000000546238539 ) ) ;
#14110 = CARTESIAN_POINT ( 'NONE',  ( 104.4587341249999781, 91.56249999863440792, -6.938893903907228378E-15 ) ) ;
#14111 = CARTESIAN_POINT ( 'NONE',  ( 99.99999999999995737, -4.999999999999990230, 9.250000000000000000 ) ) ;
#14112 = CARTESIAN_POINT ( 'NONE',  ( 93.46109445667489979, 105.2492070361643215, -55.42499999726882720 ) ) ;
#14113 = CARTESIAN_POINT ( 'NONE',  ( 13.14518615778179900, 33.16171875108393863, 5.444914386472293977 ) ) ;
#14114 = ORIENTED_EDGE ( 'NONE', *, *, #15237, .F. ) ;
#14115 = LINE ( 'NONE', #24821, #17730 ) ;
#14116 = CARTESIAN_POINT ( 'NONE',  ( -9.598844408820458085, 37.72578124999999005, -9.598844408820458085 ) ) ;
#14117 = CARTESIAN_POINT ( 'NONE',  ( 181.8548138422181921, 33.45937500108392726, 5.444914386472304635 ) ) ;
#14118 =( BOUNDED_CURVE ( )  B_SPLINE_CURVE ( 2, ( #7163, #24853, #15859, #24568, #13715, #22436, #2904, #777, #12662 ),
 .UNSPECIFIED., .F., .T. ) 
 B_SPLINE_CURVE_WITH_KNOTS ( ( 3, 2, 2, 2, 3 ),
 ( 0.03571428571428574700, 0.04464285714285718548, 0.05357142857142861703, 0.06250000000000005551, 0.07142857142857149400 ),
 .UNSPECIFIED. ) 
 CURVE ( )  GEOMETRIC_REPRESENTATION_ITEM ( )  RATIONAL_B_SPLINE_CURVE ( ( 0.9999999999999996669, 0.9238795325112870716, 1.000000000000000000, 0.9238795325112867385, 1.000000000000000000, 0.9238795325112867385, 1.000000000000000000, 0.9238795325112861834, 1.000000000000000666 ) ) 
 REPRESENTATION_ITEM ( '' )  );
#14119 = ORIENTED_EDGE ( 'NONE', *, *, #26215, .T. ) ;
#14120 = CARTESIAN_POINT ( 'NONE',  ( 192.4704160048314634, 49.99999999938371786, -13.34625891065977932 ) ) ;
#14121 = CARTESIAN_POINT ( 'NONE',  ( 96.84719886470459471, 3.152801135295383084, 6.562500001365592084 ) ) ;
#14122 = VECTOR ( 'NONE', #3321, 1000.000000000000000 ) ;
#14123 = EDGE_CURVE ( 'NONE', #12623, #4367, #16046, .T. ) ;
#14124 = ORIENTED_EDGE ( 'NONE', *, *, #14355, .F. ) ;
#14125 = CARTESIAN_POINT ( 'NONE',  ( 99.99999999999998579, 101.5015231886685854, -44.87500000273119838 ) ) ;
#14126 = CARTESIAN_POINT ( 'NONE',  ( -5.444914386472297529, 38.02343750108394005, -13.14518615778179900 ) ) ;
#14127 = CARTESIAN_POINT ( 'NONE',  ( 11.10484805054756841, 36.02027164848242791, -8.092840767093349541 ) ) ;
#14128 = CARTESIAN_POINT ( 'NONE',  ( 0.000000000000000000, 20.00000000000000000, 0.000000000000000000 ) ) ;
#14129 = CARTESIAN_POINT ( 'NONE',  ( 124.5550856135277087, 38.02343750108394005, -13.14518615778179900 ) ) ;
#14130 = CARTESIAN_POINT ( 'NONE',  ( 9.295050272127046043, 37.27929687608394005, -9.295050272127046043 ) ) ;
#14131 = CARTESIAN_POINT ( 'NONE',  ( 5.444914386472297529, 32.36796875108393579, -13.14518615778179900 ) ) ;
#14132 = CARTESIAN_POINT ( 'NONE',  ( 101.8468681455907330, 93.37499999863439371, 4.458734124999979898 ) ) ;
#14133 = CYLINDRICAL_SURFACE ( 'NONE', #6402, 4.999999999999989342 ) ;
#14134 = ORIENTED_EDGE ( 'NONE', *, *, #6697, .F. ) ;
#14135 = CARTESIAN_POINT ( 'NONE',  ( 13.57481594606304931, 38.27148437716787299, 5.622872871577868636 ) ) ;
#14136 = DIRECTION ( 'NONE',  ( -0.000000000000000000, -0.000000000000000000, -1.000000000000000000 ) ) ;
#14137 = CARTESIAN_POINT ( 'NONE',  ( 96.84719886470459471, -3.152801135295355994, 7.812500001365592084 ) ) ;
#14138 = CARTESIAN_POINT ( 'NONE',  ( 96.84719886470459471, 81.81250000136559208, 3.152801135295355994 ) ) ;
#14139 = PLANE ( 'NONE',  #16307 ) ;
#14140 = VECTOR ( 'NONE', #27786, 1000.000000000000000 ) ;
#14141 = FACE_OUTER_BOUND ( 'NONE', #7443, .T. ) ;
#14142 = CARTESIAN_POINT ( 'NONE',  ( 99.99999999999998579, 128.0000000000000000, -5.204170427930421283E-15 ) ) ;
#14143 = ORIENTED_EDGE ( 'NONE', *, *, #20668, .T. ) ;
#14144 = CARTESIAN_POINT ( 'NONE',  ( 2.414731522848535132E-15, 34.60039062608393579, 13.14518615778179544 ) ) ;
#14145 = CARTESIAN_POINT ( 'NONE',  ( 98.53841926354351699, 123.0500000010924850, 1.461580736456455920 ) ) ;
#14146 = CARTESIAN_POINT ( 'NONE',  ( 104.4587341249999923, 93.62499999863439371, -1.846868145590737198 ) ) ;
#14147 = CARTESIAN_POINT ( 'NONE',  ( 5.622872871577786924, 31.82226562716788365, 13.57481594606313813 ) ) ;
#14148 = CARTESIAN_POINT ( 'NONE',  ( 106.5389055433250860, 105.2492070361643215, -47.07499999726882578 ) ) ;
#14149 = AXIS2_PLACEMENT_3D ( 'NONE', #9472, #18173, #26886 ) ;
#14150 = CARTESIAN_POINT ( 'NONE',  ( -13.57481594606304576, 34.64999999999999147, 0.000000000000000000 ) ) ;
#14151 = CARTESIAN_POINT ( 'NONE',  ( 13.14518615778179900, 33.75703125108393010, 5.444914386472293977 ) ) ;
#14152 = ORIENTED_EDGE ( 'NONE', *, *, #1829, .T. ) ;
#14153 = LINE ( 'NONE', #6271, #22090 ) ;
#14154 = CARTESIAN_POINT ( 'NONE',  ( 104.9999999999999858, -2.071067811865442643, 0.5625000027311864992 ) ) ;
#14155 = CARTESIAN_POINT ( 'NONE',  ( 2.142451790973463043E-15, 11.00000000000000355, -17.49444650053485972 ) ) ;
#14156 = CARTESIAN_POINT ( 'NONE',  ( 208.1451861577817795, 33.26093750108393721, -5.444914386472297529 ) ) ;
#14157 = VERTEX_POINT ( 'NONE', #18877 ) ;
#14158 = CARTESIAN_POINT ( 'NONE',  ( 107.0000000000000142, 112.2744378736303332, -54.90000000000000568 ) ) ;
#14159 = CARTESIAN_POINT ( 'NONE',  ( 2.169956583107089276, 49.99999999883884527, -13.43548448457782918 ) ) ;
#14160 = DIRECTION ( 'NONE',  ( -1.000000000000000000, 0.000000000000000000, 0.000000000000000000 ) ) ;
#14161 = ADVANCED_FACE ( 'NONE', ( #5925 ), #2487, .T. ) ;
#14162 = CARTESIAN_POINT ( 'NONE',  ( 120.4011555911795455, 37.03125000216787299, -9.598844408820458085 ) ) ;
#14163 = EDGE_CURVE ( 'NONE', #10337, #5311, #26256, .T. ) ;
#14164 = FACE_OUTER_BOUND ( 'NONE', #2639, .T. ) ;
#14165 = CARTESIAN_POINT ( 'NONE',  ( 99.99999999999997158, 117.3602355696678643, -46.99999999453763877 ) ) ;
#14166 = CARTESIAN_POINT ( 'NONE',  ( 185.7049497278729575, 37.67617187608393436, 9.295050272127047819 ) ) ;
#14167 = ORIENTED_EDGE ( 'NONE', *, *, #24502, .T. ) ;
#14168 =( BOUNDED_CURVE ( )  B_SPLINE_CURVE ( 2, ( #6167, #3755, #14834, #23557, #10705, #21424, #1622, #19410, #14567, #25267, #5757, #23283, #14425, #1903, #3617, #1484, #10281, #18990, #27699, #19278, #8162, #25553, #2178, #17838, #37, #464, #24115, #13251, #11265, #17700, #9146, #25970, #24256, #22125, #12971, #15693, #2604, #23833, #9008, #19986, #322 ),
 .UNSPECIFIED., .F., .T. ) 
 B_SPLINE_CURVE_WITH_KNOTS ( ( 3, 2, 2, 2, 2, 2, 2, 2, 2, 2, 2, 2, 2, 2, 2, 2, 2, 2, 2, 2, 3 ),
 ( 0.000000000000000000, 0.04166666666666666435, 0.08333333333333332871, 0.1250000000000000000, 0.1666666666666666574, 0.2083333333333333426, 0.2500000000000000000, 0.2916666666666666852, 0.3333333333333333148, 0.3750000000000000000, 0.4166666666666666852, 0.4583333333333332593, 0.5000000000000000000, 0.5416666666666666297, 0.5833333333333333703, 0.6250000000000000000, 0.6666666666666666297, 0.7083333333333333703, 0.7500000000000000000, 0.7916666666666666297, 0.8333333333333333703 ),
 .UNSPECIFIED. ) 
 CURVE ( )  GEOMETRIC_REPRESENTATION_ITEM ( )  RATIONAL_B_SPLINE_CURVE ( ( 1.000000000000000000, 0.9238795325112867385, 1.000000000000000000, 0.9238795325112867385, 1.000000000000000000, 0.9238795325112867385, 1.000000000000000000, 0.9238795325112867385, 1.000000000000000000, 0.9238795325112867385, 1.000000000000000000, 0.9238795325112867385, 1.000000000000000000, 0.9238795325112867385, 1.000000000000000000, 0.9238795325112867385, 1.000000000000000000, 0.9238795325112867385, 1.000000000000000000, 0.9238795325112867385, 1.000000000000000000, 0.9238795325112867385, 1.000000000000000000, 0.9238795325112867385, 1.000000000000000000, 0.9238795325112867385, 1.000000000000000000, 0.9238795325112867385, 1.000000000000000000, 0.9238795325112867385, 1.000000000000000000, 0.9238795325112867385, 1.000000000000000000, 0.9238795325112867385, 1.000000000000000000, 0.9238795325112867385, 1.000000000000000000, 0.9238795325112867385, 1.000000000000000000, 0.9238795325112867385, 1.000000000000000000 ) ) 
 REPRESENTATION_ITEM ( '' )  );
#14169 = SURFACE_STYLE_FILL_AREA ( #27311 ) ;
#14170 = CARTESIAN_POINT ( 'NONE',  ( 95.54126587499995082, -1.846868145590724986, 0.5000000013655920839 ) ) ;
#14171 = CARTESIAN_POINT ( 'NONE',  ( -1.271138771240642784, 36.00000000000000000, -13.43002483374384681 ) ) ;
#14172 = CARTESIAN_POINT ( 'NONE',  ( 204.5988444088204403, 38.32109374999999574, -9.598844408820458085 ) ) ;
#14173 = ADVANCED_FACE ( 'NONE', ( #2352 ), #19670, .T. ) ;
#14174 = CARTESIAN_POINT ( 'NONE',  ( 1.137167824540872951, 35.99999999999998579, 13.09590655363602707 ) ) ;
#14175 = CARTESIAN_POINT ( 'NONE',  ( 70.44491438647230552, 32.26875000108393721, 13.14518615778179189 ) ) ;
#14176 = CARTESIAN_POINT ( 'NONE',  ( 104.9999999999999858, -2.071067811865442643, 5.437500000000001776 ) ) ;
#14177 = CARTESIAN_POINT ( 'NONE',  ( -9.295050272127046043, 40.65273437608393436, -9.295050272127046043 ) ) ;
#14178 = CARTESIAN_POINT ( 'NONE',  ( -8.312177448680279460E-16, 40.10703125216787157, -13.57481594606304576 ) ) ;
#14179 = CARTESIAN_POINT ( 'NONE',  ( 94.33688103937537051, 114.1144967660473242, -48.70000000546237828 ) ) ;
#14180 = CARTESIAN_POINT ( 'NONE',  ( 9.180175813648009608, 50.00000000000000000, 9.999999999999980460 ) ) ;
#14181 = CARTESIAN_POINT ( 'NONE',  ( 130.0000000000000000, 34.84843749999999574, 13.57481594606304576 ) ) ;
#14182 = ORIENTED_EDGE ( 'NONE', *, *, #22553, .T. ) ;
#14183 = ORIENTED_EDGE ( 'NONE', *, *, #4113, .F. ) ;
#14184 = CARTESIAN_POINT ( 'NONE',  ( 102.0710678118654187, 84.68750000000000000, -5.000000000000015987 ) ) ;
#14185 = CARTESIAN_POINT ( 'NONE',  ( -8.049105076161786076E-16, 33.40976562608393863, -13.14518615778179544 ) ) ;
#14186 = CARTESIAN_POINT ( 'NONE',  ( 9.598844408820459861, 34.25312500216787015, 9.598844408820456309 ) ) ;
#14187 = CARTESIAN_POINT ( 'NONE',  ( 94.99999999999995737, 2.071067811865491048, 4.062500002731185056 ) ) ;
#14188 = CARTESIAN_POINT ( 'NONE',  ( 116.8548138422182063, 40.70234375108393721, -5.444914386472297529 ) ) ;
#14189 = CARTESIAN_POINT ( 'NONE',  ( 70.62287287157786864, 32.11992187716787583, -13.57481594606304753 ) ) ;
#14190 = CARTESIAN_POINT ( 'NONE',  ( 13.57481594606304576, 37.52734375216787299, -1.662435489736055892E-15 ) ) ;
#14191 = CARTESIAN_POINT ( 'NONE',  ( -13.14518615778179900, 37.32890625108393579, -5.444914386472297529 ) ) ;
#14192 = EDGE_CURVE ( 'NONE', #27535, #19618, #4827, .T. ) ;
#14193 = CARTESIAN_POINT ( 'NONE',  ( 9.295050272127046043, 32.51679687608393721, -9.295050272127046043 ) ) ;
#14194 = FACE_OUTER_BOUND ( 'NONE', #27324, .T. ) ;
#14195 = CARTESIAN_POINT ( 'NONE',  ( 102.4976396683250783, 102.3130555110000159, -51.27499999726882152 ) ) ;
#14196 = ORIENTED_EDGE ( 'NONE', *, *, #13135, .T. ) ;
#14197 = CARTESIAN_POINT ( 'NONE',  ( 13.14518615778179900, 40.20625000108393010, -5.444914386472297529 ) ) ;
#14198 = DIRECTION ( 'NONE',  ( -0.000000000000000000, 1.000000000000000000, -0.000000000000000000 ) ) ;
#14199 = CARTESIAN_POINT ( 'NONE',  ( 65.00000000000000000, -7.395377635281828788, -13.57481594606305109 ) ) ;
#14200 = EDGE_CURVE ( 'NONE', #28009, #9895, #18094, .T. ) ;
#14201 = FACE_OUTER_BOUND ( 'NONE', #26550, .T. ) ;
#14202 = CARTESIAN_POINT ( 'NONE',  ( 107.0000000000000142, 107.7255621263696526, -47.10000000000000142 ) ) ;
#14203 = CARTESIAN_POINT ( 'NONE',  ( 96.84719886470459471, -3.152801135295355994, 13.56250000136559208 ) ) ;
#14204 = CARTESIAN_POINT ( 'NONE',  ( -5.622872871577873077, 34.00507812499999716, 13.57481594606304753 ) ) ;
#14205 = ORIENTED_EDGE ( 'NONE', *, *, #18185, .F. ) ;
#14206 = CARTESIAN_POINT ( 'NONE',  ( 107.0000000000000142, 107.7255621263696668, -49.59999999453765440 ) ) ;
#14207 =( BOUNDED_CURVE ( )  B_SPLINE_CURVE ( 2, ( #717, #6968, #143, #17378, #11092, #2291, #2847, #15663, #11516 ),
 .UNSPECIFIED., .F., .F. ) 
 B_SPLINE_CURVE_WITH_KNOTS ( ( 3, 2, 2, 2, 3 ),
 ( 0.6874999999999997780, 0.6979166666666665186, 0.7083333333333333703, 0.7187500000000001110, 0.7291666666666668517 ),
 .UNSPECIFIED. ) 
 CURVE ( )  GEOMETRIC_REPRESENTATION_ITEM ( )  RATIONAL_B_SPLINE_CURVE ( ( 1.000000000000001554, 0.9238795325112850731, 1.000000000000000000, 0.9238795325112867385, 1.000000000000000000, 0.9238795325112867385, 1.000000000000000000, 0.9238795325112850731, 1.000000000000001554 ) ) 
 REPRESENTATION_ITEM ( '' )  );
#14208 = CARTESIAN_POINT ( 'NONE',  ( -9.598844408820458085, 40.10703124999999147, -9.598844408820458085 ) ) ;
#14209 = CARTESIAN_POINT ( 'NONE',  ( 5.444914386472302859, 32.07031250108393294, 13.14518615778179189 ) ) ;
#14210 = CARTESIAN_POINT ( 'NONE',  ( 13.14518615778179722, 35.44375000108393436, -5.444914386472297529 ) ) ;
#14211 = VECTOR ( 'NONE', #17899, 999.9999999999998863 ) ;
#14212 = EDGE_CURVE ( 'NONE', #9199, #1383, #966, .T. ) ;
#14213 = CARTESIAN_POINT ( 'NONE',  ( 9.598844408820459861, 34.25312500216787015, 9.598844408820456309 ) ) ;
#14214 = CARTESIAN_POINT ( 'NONE',  ( 97.92893218813443923, 80.18750000000001421, 4.999999999999927169 ) ) ;
#14215 = CARTESIAN_POINT ( 'NONE',  ( 95.54126587499995082, 83.50000000136560629, 1.846868145590724986 ) ) ;
#14216 = CARTESIAN_POINT ( 'NONE',  ( 65.00000000000000000, 40.55351562608393579, -13.14518615778179544 ) ) ;
#14217 = CARTESIAN_POINT ( 'NONE',  ( 99.99999999999998579, 90.25000000000000000, -4.999999999999997335 ) ) ;
#14218 = CARTESIAN_POINT ( 'NONE',  ( 97.83688103937537051, 103.3426043859339103, -46.60000000000000853 ) ) ;
#14219 = CARTESIAN_POINT ( 'NONE',  ( 0.000000000000000000, 40.99999999999999289, 0.000000000000000000 ) ) ;
#14220 = CARTESIAN_POINT ( 'NONE',  ( -9.598844408820458085, 33.75703124999999005, -9.598844408820458085 ) ) ;
#14221 = CARTESIAN_POINT ( 'NONE',  ( 91.91746824999998466, 110.0000000000000000, -51.87499999726882294 ) ) ;
#14222 = CARTESIAN_POINT ( 'NONE',  ( 143.1451861577818079, 34.79882812608394005, -1.609821015232357215E-15 ) ) ;
#14223 = ORIENTED_EDGE ( 'NONE', *, *, #6047, .F. ) ;
#14224 = DIRECTION ( 'NONE',  ( -1.000000000000000000, 0.000000000000000000, 2.385244779468110248E-16 ) ) ;
#14225 = CARTESIAN_POINT ( 'NONE',  ( 95.54126587499995082, 83.50000000136560629, 1.846868145590724986 ) ) ;
#14226 = CARTESIAN_POINT ( 'NONE',  ( 124.5550856135277087, 38.81718750108393579, -13.14518615778179900 ) ) ;
#14227 = CARTESIAN_POINT ( 'NONE',  ( 65.00000000000000000, 39.31328125216787583, -13.57481594606304576 ) ) ;
#14228 = CARTESIAN_POINT ( 'NONE',  ( 102.1631189606246153, 116.6573956140660897, -53.60000000000000853 ) ) ;
#14229 = CARTESIAN_POINT ( 'NONE',  ( 185.7049497278729575, 40.05742187608393579, 9.295050272127047819 ) ) ;
#14230 = CARTESIAN_POINT ( 'NONE',  ( -13.57481594606304753, 39.46210937716787726, -5.622872871577873077 ) ) ;
#14231 = ORIENTED_EDGE ( 'NONE', *, *, #5465, .T. ) ;
#14232 = VECTOR ( 'NONE', #2250, 1000.000000000000000 ) ;
#14233 = CARTESIAN_POINT ( 'NONE',  ( 96.46446609406721961, 3.535533905932755072, 8.875000000000000000 ) ) ;
#14234 = ORIENTED_EDGE ( 'NONE', *, *, #9321, .F. ) ;
#14235 = CARTESIAN_POINT ( 'NONE',  ( -9.295050272127046043, 34.30273437608393294, -9.295050272127046043 ) ) ;
#14236 = CARTESIAN_POINT ( 'NONE',  ( 189.3771271284221314, 31.42539062716787157, -13.57481594606304753 ) ) ;
#14237 = FACE_OUTER_BOUND ( 'NONE', #12300, .T. ) ;
#14238 = EDGE_CURVE ( 'NONE', #8092, #12157, #6425, .T. ) ;
#14239 = CARTESIAN_POINT ( 'NONE',  ( 103.5355339059327093, 3.535533905932755072, 12.75000000273118594 ) ) ;
#14240 = CARTESIAN_POINT ( 'NONE',  ( 120.7049497278729575, 40.45429687608393721, -9.295050272127046043 ) ) ;
#14241 = FACE_OUTER_BOUND ( 'NONE', #22438, .T. ) ;
#14242 = FACE_OUTER_BOUND ( 'NONE', #1058, .T. ) ;
#14243 = CARTESIAN_POINT ( 'NONE',  ( 104.4587341249999923, 91.37499999863442213, -1.846868145590737198 ) ) ;
#14244 = CARTESIAN_POINT ( 'NONE',  ( 99.99999999999998579, 124.1500000010924651, 2.066987299999980099 ) ) ;
#14245 = CARTESIAN_POINT ( 'NONE',  ( 204.5988444088204687, 39.71015624999999716, 9.598844408820456309 ) ) ;
#14246 = CARTESIAN_POINT ( 'NONE',  ( 117.0005117698093784, 35.99999999999999289, 1.999176114741889165 ) ) ;
#14247 = CARTESIAN_POINT ( 'NONE',  ( 98.15313185440925281, 4.458734125000016313, 7.500000001365592084 ) ) ;
#14248 = CARTESIAN_POINT ( 'NONE',  ( 55.70494972787295751, 40.45429687608393721, -9.295050272127046043 ) ) ;
#14249 = CARTESIAN_POINT ( 'NONE',  ( 98.15313185440923860, -4.458734124999987891, 10.62500000136559208 ) ) ;
#14250 = CARTESIAN_POINT ( 'NONE',  ( 99.99999999999998579, 102.6397644303321215, -50.00000000546236834 ) ) ;
#14251 = CARTESIAN_POINT ( 'NONE',  ( 98.15313185440925281, 94.87499999863440792, -4.458734124999994997 ) ) ;
#14252 = CARTESIAN_POINT ( 'NONE',  ( -8.312177448680279460E-16, 40.00781250000000000, -13.57481594606304576 ) ) ;
#14253 = CARTESIAN_POINT ( 'NONE',  ( 91.91746824999997045, 107.3738262389971680, -53.52499999726882862 ) ) ;
#14254 = CARTESIAN_POINT ( 'NONE',  ( 9.295050272127046043, 33.31054687608394005, -9.295050272127046043 ) ) ;
#14255 = AXIS2_PLACEMENT_3D ( 'NONE', #6308, #27090, #7541 ) ;
#14256 = ORIENTED_EDGE ( 'NONE', *, *, #2205, .F. ) ;
#14257 = CARTESIAN_POINT ( 'NONE',  ( 103.1528011352953342, 82.06250000136559208, 3.152801135295355106 ) ) ;
#14258 =( BOUNDED_CURVE ( )  B_SPLINE_CURVE ( 2, ( #18635, #27339, #14059, #3248, #981, #27474, #26918, #7362, #18351 ),
 .UNSPECIFIED., .F., .T. ) 
 B_SPLINE_CURVE_WITH_KNOTS ( ( 3, 2, 2, 2, 3 ),
 ( 0.2500000000000002220, 0.2750000000000002442, 0.3000000000000002665, 0.3250000000000002887, 0.3500000000000003109 ),
 .UNSPECIFIED. ) 
 CURVE ( )  GEOMETRIC_REPRESENTATION_ITEM ( )  RATIONAL_B_SPLINE_CURVE ( ( 0.9999999999999993339, 0.9238795325112874046, 1.000000000000000000, 0.9238795325112867385, 1.000000000000000000, 0.9238795325112867385, 1.000000000000000000, 0.9238795325112857393, 1.000000000000001110 ) ) 
 REPRESENTATION_ITEM ( '' )  );
#14259 = CARTESIAN_POINT ( 'NONE',  ( 99.99999999999998579, 90.00000000000000000, -2.999999999999996447 ) ) ;
#14260 = CARTESIAN_POINT ( 'NONE',  ( 200.4449143864723055, 33.95546875108393436, -13.14518615778179900 ) ) ;
#14261 = ORIENTED_EDGE ( 'NONE', *, *, #2536, .T. ) ;
#14262 = CARTESIAN_POINT ( 'NONE',  ( 188.5871333237481053, 50.00000000108477849, -11.99502265407749668 ) ) ;
#14263 = CARTESIAN_POINT ( 'NONE',  ( 96.84719886470459471, 3.152801135295383084, 8.562500001365592084 ) ) ;
#14264 = ORIENTED_EDGE ( 'NONE', *, *, #15422, .F. ) ;
#14265 = CARTESIAN_POINT ( 'NONE',  ( 108.0825317500000011, 112.6261737610028320, -48.27500000273119696 ) ) ;
#14266 = CARTESIAN_POINT ( 'NONE',  ( 13.14518615778179900, 32.16953125108393152, 5.444914386472293977 ) ) ;
#14267 = CARTESIAN_POINT ( 'NONE',  ( 181.4251840539369596, 38.71796875216787726, 0.000000000000000000 ) ) ;
#14268 = CARTESIAN_POINT ( 'NONE',  ( -13.14518615778179722, 40.50390625108394005, -5.444914386472297529 ) ) ;
#14269 = CARTESIAN_POINT ( 'NONE',  ( 13.14518615778179722, 38.81718750108393579, -5.444914386472297529 ) ) ;
#14270 = AXIS2_PLACEMENT_3D ( 'NONE', #15310, #6079, #4219 ) ;
#14271 = CARTESIAN_POINT ( 'NONE',  ( 5.444914386472302859, 32.86406250108392868, 13.14518615778179189 ) ) ;
#14272 = CARTESIAN_POINT ( 'NONE',  ( 104.4587341249999923, 91.62499999863440792, -1.846868145590737198 ) ) ;
#14273 = CARTESIAN_POINT ( 'NONE',  ( 102.4999999999999858, 123.0000000000000000, -8.724596124144689908E-15 ) ) ;
#14274 = CARTESIAN_POINT ( 'NONE',  ( 95.67376207875072680, 104.0454443415356991, -50.70000000000000284 ) ) ;
#14275 = CARTESIAN_POINT ( 'NONE',  ( 5.444914386472297529, 32.56640625108394005, -13.14518615778179900 ) ) ;
#14276 = CARTESIAN_POINT ( 'NONE',  ( 99.99999999999995737, 4.458734125000016313, 3.437500001365592972 ) ) ;
#14277 = CARTESIAN_POINT ( 'NONE',  ( 96.84719886470459471, 83.81250000136560629, 3.152801135295355994 ) ) ;
#14278 = CARTESIAN_POINT ( 'NONE',  ( -5.444914386472297529, 35.64218750108392442, -13.14518615778179900 ) ) ;
#14279 = DIRECTION ( 'NONE',  ( 0.000000000000000000, 0.000000000000000000, 1.000000000000000000 ) ) ;
#14280 = DIRECTION ( 'NONE',  ( -0.000000000000000000, -0.000000000000000000, -1.000000000000000000 ) ) ;
#14281 = ORIENTED_EDGE ( 'NONE', *, *, #10867, .F. ) ;
#14282 = CARTESIAN_POINT ( 'NONE',  ( 13.14518615778179544, 34.79882812608394005, -1.609821015232357215E-15 ) ) ;
#14283 = EDGE_CURVE ( 'NONE', #9015, #10849, #24588, .T. ) ;
#14284 =( BOUNDED_CURVE ( )  B_SPLINE_CURVE ( 2, ( #14052, #3101, #22773, #11340, #9642, #7502, #26626, #1114, #16196 ),
 .UNSPECIFIED., .F., .T. ) 
 B_SPLINE_CURVE_WITH_KNOTS ( ( 3, 2, 2, 2, 3 ),
 ( 0.000000000000000000, 0.008928571428571436749, 0.01785714285714287350, 0.02678571428571431198, 0.03571428571428574700 ),
 .UNSPECIFIED. ) 
 CURVE ( )  GEOMETRIC_REPRESENTATION_ITEM ( )  RATIONAL_B_SPLINE_CURVE ( ( 1.000000000000000000, 0.9238795325112867385, 1.000000000000000000, 0.9238795325112867385, 1.000000000000000000, 0.9238795325112867385, 1.000000000000000000, 0.9238795325112864054, 1.000000000000000222 ) ) 
 REPRESENTATION_ITEM ( '' )  );
#14285 = CARTESIAN_POINT ( 'NONE',  ( 97.93301270000000613, 124.5500000010924850, -9.540979117872439019E-15 ) ) ;
#14286 = CARTESIAN_POINT ( 'NONE',  ( 101.8468681455907330, 94.74999999863439371, -4.458734124999994997 ) ) ;
#14287 = CARTESIAN_POINT ( 'NONE',  ( 0.000000000000000000, 40.99999999999999289, 0.000000000000000000 ) ) ;
#14288 = CARTESIAN_POINT ( 'NONE',  ( -9.598844408820458085, 40.10703124999999147, -9.598844408820458085 ) ) ;
#14289 = DIRECTION ( 'NONE',  ( 0.000000000000000000, 0.000000000000000000, 1.000000000000000000 ) ) ;
#14290 = CARTESIAN_POINT ( 'NONE',  ( 9.295050272127047819, 32.11992187608393579, 9.295050272127046043 ) ) ;
#14291 = ORIENTED_EDGE ( 'NONE', *, *, #8444, .T. ) ;
#14292 = CARTESIAN_POINT ( 'NONE',  ( 97.83688103937535629, 116.6573956140660897, -45.40000000000001279 ) ) ;
#14293 = CARTESIAN_POINT ( 'NONE',  ( 51.85481384221820633, 36.73359375108393010, -5.444914386472297529 ) ) ;
#14294 = LINE ( 'NONE', #16306, #3238 ) ;
#14295 = LINE ( 'NONE', #4045, #3029 ) ;
#14296 = ORIENTED_EDGE ( 'NONE', *, *, #18321, .T. ) ;
#14297 = CARTESIAN_POINT ( 'NONE',  ( 65.00000000000000000, 37.22968749999999716, 13.57481594606304576 ) ) ;
#14298 = CARTESIAN_POINT ( 'NONE',  ( 97.92893218813452449, 91.56249999726881583, 4.999999999999991118 ) ) ;
#14299 = CARTESIAN_POINT ( 'NONE',  ( 94.99999999999995737, 1.387778780781445676E-14, 2.999999999999999112 ) ) ;
#14300 = CARTESIAN_POINT ( 'NONE',  ( 139.5988444088204403, 39.21406250216787015, -9.598844408820458085 ) ) ;
#14301 = CARTESIAN_POINT ( 'NONE',  ( 97.83688103937538472, 116.6573956140660897, -44.90000000546237402 ) ) ;
#14302 = CARTESIAN_POINT ( 'NONE',  ( 92.99999999999998579, 112.2744378736303190, -46.59999999453763309 ) ) ;
#14303 = CARTESIAN_POINT ( 'NONE',  ( 208.1451861577817795, 39.51171875108392584, 5.444914386472293977 ) ) ;
#14304 = ORIENTED_EDGE ( 'NONE', *, *, #28137, .F. ) ;
#14305 = CARTESIAN_POINT ( 'NONE',  ( 99.99999999999995737, -4.458734124999988779, 1.687500001365591418 ) ) ;
#14306 = DIRECTION ( 'NONE',  ( -0.8660254037844418162, 0.000000000000000000, -0.4999999999999947264 ) ) ;
#14307 = CARTESIAN_POINT ( 'NONE',  ( 9.598844408820456309, 39.90859374999999432, -9.598844408820458085 ) ) ;
#14308 = CARTESIAN_POINT ( 'NONE',  ( 0.000000000000000000, 21.36169591142201440, 0.000000000000000000 ) ) ;
#14309 = CARTESIAN_POINT ( 'NONE',  ( 99.99999999999998579, 110.0000000000000000, -45.00000000000000711 ) ) ;
#14310 = CARTESIAN_POINT ( 'NONE',  ( 5.444914386472297529, 39.71015625108393010, -13.14518615778179900 ) ) ;
#14311 = CARTESIAN_POINT ( 'NONE',  ( 9.295050272127047819, 36.08867187608392868, 9.295050272127046043 ) ) ;
#14312 = CIRCLE ( 'NONE', #27546, 4.999999999999999112 ) ;
#14313 = CARTESIAN_POINT ( 'NONE',  ( 217.9999999999999716, 80.00000000000000000, -13.00000000000000000 ) ) ;
#14314 = DIRECTION ( 'NONE',  ( -0.000000000000000000, -0.000000000000000000, -1.000000000000000000 ) ) ;
#14315 = CARTESIAN_POINT ( 'NONE',  ( 135.6228728715778971, 33.31054687499999289, 13.57481594606304576 ) ) ;
#14316 = VERTEX_POINT ( 'NONE', #15837 ) ;
#14317 = VERTEX_POINT ( 'NONE', #4742 ) ;
#14318 = CARTESIAN_POINT ( 'NONE',  ( 78.57481594606305464, 36.63437499999999858, -1.662435489736055892E-15 ) ) ;
#14319 = PRODUCT_DEFINITION_CONTEXT ( 'detailed design', #22453, 'design' ) ;
#14320 = CARTESIAN_POINT ( 'NONE',  ( -9.598844408820458085, 38.51953124999999289, -9.598844408820458085 ) ) ;
#14321 = CARTESIAN_POINT ( 'NONE',  ( -9.598844408820458085, 31.47500000216787441, -9.598844408820458085 ) ) ;
#14322 = CARTESIAN_POINT ( 'NONE',  ( 94.99999999999995737, 1.387778780781445676E-14, 5.125000002731184168 ) ) ;
#14323 = CARTESIAN_POINT ( 'NONE',  ( 135.4449143864723055, 38.61875000108393152, 13.14518615778179189 ) ) ;
#14324 = CARTESIAN_POINT ( 'NONE',  ( 78.14518615778179367, 37.77539062608393294, -1.609821015232357215E-15 ) ) ;
#14325 = B_SPLINE_CURVE_WITH_KNOTS ( 'NONE', 3,
 ( #18986, #22998, #25413, #25550, #5471, #18848, #5614, #20860, #18716, #14423, #23139, #3468, #22860, #1342, #3614, #12273, #12548, #12414 ),
 .UNSPECIFIED., .F., .F.,
 ( 4, 2, 2, 2, 2, 2, 2, 2, 4 ),
 ( 0.000000000000000000, 0.004618502246277170556, 0.006927753369415742823, 0.009237004492554316826, 0.01039163005412362291, 0.01154625561569293073, 0.01385550673883149779, 0.01616475786197006659, 0.01847400898510863712 ),
 .UNSPECIFIED. ) ;
#14326 = ORIENTED_EDGE ( 'NONE', *, *, #10987, .T. ) ;
#14327 = PLANE ( 'NONE',  #24336 ) ;
#14328 = CARTESIAN_POINT ( 'NONE',  ( -9.295050272127046043, 38.86679687608393863, -9.295050272127046043 ) ) ;
#14329 = CARTESIAN_POINT ( 'NONE',  ( 97.50000000000000000, 123.4500000021849502, -1.035533905932742416 ) ) ;
#14330 = CARTESIAN_POINT ( 'NONE',  ( 2.493653234604083739E-15, 35.64218749999999147, 13.57481594606304576 ) ) ;
#14331 = CARTESIAN_POINT ( 'NONE',  ( 99.99999999999997158, 118.4984768113314146, -54.37499999726881583 ) ) ;
#14332 = VECTOR ( 'NONE', #3080, 1000.000000000000000 ) ;
#14333 = CARTESIAN_POINT ( 'NONE',  ( 2.493653234604083739E-15, 34.05468749999999289, 13.57481594606304576 ) ) ;
#14334 = LINE ( 'NONE', #7509, #27272 ) ;
#14335 = CARTESIAN_POINT ( 'NONE',  ( 139.4320061696339508, 36.00000000000000000, 9.391769196590345814 ) ) ;
#14336 = CARTESIAN_POINT ( 'NONE',  ( 98.96446609406727646, 124.0499999999999972, -2.499999999999997780 ) ) ;
#14337 = CARTESIAN_POINT ( 'NONE',  ( 97.93301269999999192, 123.0000000010925163, 0.8561741729129329626 ) ) ;
#14338 = CARTESIAN_POINT ( 'NONE',  ( 126.5797791878282226, 36.00000000000000711, -13.02105590829171256 ) ) ;
#14339 = EDGE_CURVE ( 'NONE', #8588, #5516, #2200, .T. ) ;
#14340 = CARTESIAN_POINT ( 'NONE',  ( 185.4011555911795597, 39.61093750216787868, 9.598844408820459861 ) ) ;
#14341 = CARTESIAN_POINT ( 'NONE',  ( 96.84719886470459471, 3.152801135295383084, 12.31250000136559208 ) ) ;
#14342 = CARTESIAN_POINT ( 'NONE',  ( 204.1801758136480203, 50.00000000000000000, -10.00000000000000000 ) ) ;
#14343 = VECTOR ( 'NONE', #4750, 1000.000000000000000 ) ;
#14344 = CIRCLE ( 'NONE', #18477, 4.999999999999989342 ) ;
#14345 = EDGE_LOOP ( 'NONE', ( #1352, #11883, #19375, #8900 ) ) ;
#14346 = CARTESIAN_POINT ( 'NONE',  ( -13.15267690958718205, 36.00000000000000711, 0.5874252385153145850 ) ) ;
#14347 = CARTESIAN_POINT ( 'NONE',  ( -13.57481594606304576, 39.41249999999999432, 0.000000000000000000 ) ) ;
#14348 = CARTESIAN_POINT ( 'NONE',  ( -5.444914386472299306, 33.55859375108393294, 13.14518615778179722 ) ) ;
#14349 = CARTESIAN_POINT ( 'NONE',  ( -9.598844408820458085, 32.26875000216787726, -9.598844408820458085 ) ) ;
#14350 = CARTESIAN_POINT ( 'NONE',  ( 104.9999999999999716, 1.449011120738813565E-14, 2.499999999999998668 ) ) ;
#14351 = CARTESIAN_POINT ( 'NONE',  ( 96.84719886470459471, 83.56250000136560629, -3.152801135295383084 ) ) ;
#14352 = CARTESIAN_POINT ( 'NONE',  ( 65.00000000000000000, 40.15664062608393436, 13.14518615778179544 ) ) ;
#14353 = CARTESIAN_POINT ( 'NONE',  ( 91.91746824999998466, 107.3738262389971538, -45.27500000273118985 ) ) ;
#14354 = CARTESIAN_POINT ( 'NONE',  ( 108.0825317500000153, 110.0000000000000000, -44.12500000273119127 ) ) ;
#14355 = EDGE_CURVE ( 'NONE', #20160, #2344, #1433, .T. ) ;
#14356 = CARTESIAN_POINT ( 'NONE',  ( 99.14382582708707048, 123.3000000010924708, 2.066987299999979211 ) ) ;
#14357 = CARTESIAN_POINT ( 'NONE',  ( 13.57481594606304753, 33.50898437499999716, -5.622872871577873966 ) ) ;
#14358 = CARTESIAN_POINT ( 'NONE',  ( 99.99999999999997158, 102.6397644303321215, -47.99999999453763877 ) ) ;
#14359 = CARTESIAN_POINT ( 'NONE',  ( 139.2950502721270425, 34.10429687608393579, -9.295050272127046043 ) ) ;
#14360 = ORIENTED_EDGE ( 'NONE', *, *, #7090, .F. ) ;
#14361 = CARTESIAN_POINT ( 'NONE',  ( 104.9999999999999716, 1.449011120738813565E-14, 7.500000000000000000 ) ) ;
#14362 = ADVANCED_FACE ( 'NONE', ( #13402 ), #11270, .F. ) ;
#14363 = CARTESIAN_POINT ( 'NONE',  ( 95.00000000000000000, 94.50000000000000000, -7.551217303480904118E-15 ) ) ;
#14364 = CARTESIAN_POINT ( 'NONE',  ( 99.99999999999995737, 83.18750000136560629, -4.458734125000016313 ) ) ;
#14365 = CARTESIAN_POINT ( 'NONE',  ( 116.8548138422182063, 39.01562500108393294, 5.444914386472304635 ) ) ;
#14366 = CARTESIAN_POINT ( 'NONE',  ( 55.40115559117954547, 40.20625000216787726, -9.598844408820458085 ) ) ;
#14367 = EDGE_CURVE ( 'NONE', #6540, #19007, #6708, .T. ) ;
#14368 = CARTESIAN_POINT ( 'NONE',  ( 102.4976396683250783, 102.3130555110000159, -55.02499999726882152 ) ) ;
#14369 = CARTESIAN_POINT ( 'NONE',  ( 5.622872871577871301, 37.67617187716787441, -13.57481594606304753 ) ) ;
#14370 = EDGE_LOOP ( 'NONE', ( #21521, #12178, #12159, #22746 ) ) ;
#14371 = CARTESIAN_POINT ( 'NONE',  ( 99.99999999999995737, 5.000000000000018652, 9.749999999999998224 ) ) ;
#14372 = EDGE_CURVE ( 'NONE', #7460, #27733, #26263, .T. ) ;
#14373 = ORIENTED_EDGE ( 'NONE', *, *, #21548, .F. ) ;
#14374 = CARTESIAN_POINT ( 'NONE',  ( -9.295050272127044266, 32.11992187608393579, 9.295050272127047819 ) ) ;
#14375 = CARTESIAN_POINT ( 'NONE',  ( 189.5550856135277229, 39.11484375108394573, 13.14518615778179722 ) ) ;
#14376 =( BOUNDED_CURVE ( )  B_SPLINE_CURVE ( 2, ( #22620, #5229, #14040, #3090, #11757 ),
 .UNSPECIFIED., .F., .F. ) 
 B_SPLINE_CURVE_WITH_KNOTS ( ( 3, 2, 3 ),
 ( 0.000000000000000000, 0.01041666666666679446, 0.02083333333333358892 ),
 .UNSPECIFIED. ) 
 CURVE ( )  GEOMETRIC_REPRESENTATION_ITEM ( )  RATIONAL_B_SPLINE_CURVE ( ( 1.000000000000000000, 0.9238795325112867385, 1.000000000000000000, 0.9238795325112848511, 1.000000000000001776 ) ) 
 REPRESENTATION_ITEM ( '' )  );
#14377 = CARTESIAN_POINT ( 'NONE',  ( 94.99999999999995737, -2.071067811865466624, 13.18750000273118594 ) ) ;
#14378 = CARTESIAN_POINT ( 'NONE',  ( 130.0000000000000000, 38.76757812608393294, -13.14518615778179544 ) ) ;
#14379 = CARTESIAN_POINT ( 'NONE',  ( -13.14518615778179189, 32.07031250108393294, 5.444914386472304635 ) ) ;
#14380 = CARTESIAN_POINT ( 'NONE',  ( 97.92893218813451028, 5.000000000000018652, 11.93750000273118950 ) ) ;
#14381 = CARTESIAN_POINT ( 'NONE',  ( 103.1528011352953484, 94.18749999863440792, 3.152801135295352886 ) ) ;
#14382 = CARTESIAN_POINT ( 'NONE',  ( 98.96446609406727646, 124.0499999999999972, -2.499999999999997780 ) ) ;
#14383 = CARTESIAN_POINT ( 'NONE',  ( 208.5748159460630120, 40.55351562499998863, 5.622872871577869525 ) ) ;
#14384 = ADVANCED_FACE ( 'NONE', ( #24124 ), #9850, .T. ) ;
#14385 = SHAPE_DEFINITION_REPRESENTATION ( #8744, #14947 ) ;
#14386 = CARTESIAN_POINT ( 'NONE',  ( 103.1528011352953342, -3.152801135295355106, 9.062500001365592084 ) ) ;
#14387 = DIRECTION ( 'NONE',  ( 1.000000000000000000, 0.000000000000000000, 0.000000000000000000 ) ) ;
#14388 = CARTESIAN_POINT ( 'NONE',  ( 96.84719886470459471, 3.152801135295383084, 5.312500001365592972 ) ) ;
#14389 = CARTESIAN_POINT ( 'NONE',  ( 93.00000000000001421, 112.2744378736303332, -46.60000000546238397 ) ) ;
#14390 = CARTESIAN_POINT ( 'NONE',  ( 103.1528011352953484, 94.68749999863440792, -3.152801135295366208 ) ) ;
#14391 = AXIS2_PLACEMENT_3D ( 'NONE', #81, #23598, #16894 ) ;
#14392 = CARTESIAN_POINT ( 'NONE',  ( 94.99999999999995737, -2.071067811865466624, 9.062500000000000000 ) ) ;
#14393 = PLANE ( 'NONE',  #22118 ) ;
#14394 = CARTESIAN_POINT ( 'NONE',  ( -13.57481594606304576, 40.99999999999999289, 0.000000000000000000 ) ) ;
#14395 = EDGE_LOOP ( 'NONE', ( #27438, #13597 ) ) ;
#14396 = CARTESIAN_POINT ( 'NONE',  ( 104.4587341249999781, 84.25000000136559208, -1.846868145590750299 ) ) ;
#14397 = EDGE_CURVE ( 'NONE', #1506, #18417, #11693, .T. ) ;
#14398 = ORIENTED_EDGE ( 'NONE', *, *, #2854, .F. ) ;
#14399 = EDGE_CURVE ( 'NONE', #24537, #2527, #13973, .T. ) ;
#14400 = EDGE_LOOP ( 'NONE', ( #12274, #6240, #8773, #11440 ) ) ;
#14401 = VECTOR ( 'NONE', #15675, 1000.000000000000000 ) ;
#14402 = CARTESIAN_POINT ( 'NONE',  ( 188.9140557840131862, 54.65299103241510181, -15.00000000000000000 ) ) ;
#14403 = CARTESIAN_POINT ( 'NONE',  ( 101.8468681455906903, 4.458734125000016313, 8.375000001365592084 ) ) ;
#14404 = EDGE_LOOP ( 'NONE', ( #25290, #25358, #7254, #10590 ) ) ;
#14405 = CARTESIAN_POINT ( 'NONE',  ( 91.91746824999998466, 107.3738262389971538, -45.27500000273118985 ) ) ;
#14406 = CARTESIAN_POINT ( 'NONE',  ( -5.444914386472299306, 31.97109375108393436, 13.14518615778179722 ) ) ;
#14407 = AXIS2_PLACEMENT_3D ( 'NONE', #10081, #1837, #7955 ) ;
#14408 = CARTESIAN_POINT ( 'NONE',  ( 51.85481384221820633, 40.55351562608393579, 0.000000000000000000 ) ) ;
#14409 = CARTESIAN_POINT ( 'NONE',  ( -13.14518615778179544, 38.17226562608393436, 0.000000000000000000 ) ) ;
#14410 = CARTESIAN_POINT ( 'NONE',  ( 104.9952793366501709, 116.8754121666685393, -45.82500000273119412 ) ) ;
#14411 = AXIS2_PLACEMENT_3D ( 'NONE', #22754, #9202, #16027 ) ;
#14412 = CARTESIAN_POINT ( 'NONE',  ( 116.8548138422182205, 38.37070312608393152, 0.000000000000000000 ) ) ;
#14413 = CARTESIAN_POINT ( 'NONE',  ( -8.049105076161786076E-16, 33.21132812608393436, -13.14518615778179544 ) ) ;
#14414 = CARTESIAN_POINT ( 'NONE',  ( 78.57481594606304043, 38.96601562499999005, 5.622872871577869525 ) ) ;
#14415 = CARTESIAN_POINT ( 'NONE',  ( 65.00000000000000000, 38.02343749999999289, 13.57481594606304576 ) ) ;
#14416 =( BOUNDED_CURVE ( )  B_SPLINE_CURVE ( 2, ( #407, #15343, #21931, #8527, #2548, #15199, #22209, #17212, #6657 ),
 .UNSPECIFIED., .F., .F. ) 
 B_SPLINE_CURVE_WITH_KNOTS ( ( 3, 2, 2, 2, 3 ),
 ( 0.6041666666666668517, 0.6145833333333334814, 0.6250000000000001110, 0.6354166666666667407, 0.6458333333333333703 ),
 .UNSPECIFIED. ) 
 CURVE ( )  GEOMETRIC_REPRESENTATION_ITEM ( )  RATIONAL_B_SPLINE_CURVE ( ( 0.9999999999999983347, 0.9238795325112884038, 1.000000000000000000, 0.9238795325112867385, 1.000000000000000000, 0.9238795325112867385, 1.000000000000000000, 0.9238795325112867385, 1.000000000000000000 ) ) 
 REPRESENTATION_ITEM ( '' )  );
#14417 = CARTESIAN_POINT ( 'NONE',  ( -5.444914386472297529, 32.66562500108393863, -13.14518615778179900 ) ) ;
#14418 = CARTESIAN_POINT ( 'NONE',  ( 98.15313185440923860, -4.458734124999987891, 2.875000001365592528 ) ) ;
#14419 = AXIS2_PLACEMENT_3D ( 'NONE', #21837, #23965, #11111 ) ;
#14420 = CARTESIAN_POINT ( 'NONE',  ( 95.54126587499996504, 82.75000000136560629, 1.846868145590724986 ) ) ;
#14421 = CARTESIAN_POINT ( 'NONE',  ( -5.444914386472299306, 35.93984375108392726, 13.14518615778179722 ) ) ;
#14422 = LINE ( 'NONE', #16288, #19951 ) ;
#14423 = CARTESIAN_POINT ( 'NONE',  ( 66.50101912430496043, 53.60014735326988955, 14.99999999999997868 ) ) ;
#14424 = ORIENTED_EDGE ( 'NONE', *, *, #18554, .T. ) ;
#14425 = CARTESIAN_POINT ( 'NONE',  ( 99.99999999999998579, 123.9500000010924765, 2.066987299999980099 ) ) ;
#14426 = CARTESIAN_POINT ( 'NONE',  ( 101.8468681455907330, 95.37499999863440792, 4.458734124999980786 ) ) ;
#14427 = CARTESIAN_POINT ( 'NONE',  ( 208.1451861577818079, 36.33671875108393579, 5.444914386472293977 ) ) ;
#14428 = CARTESIAN_POINT ( 'NONE',  ( 95.00472066334982912, 103.1245878333314323, -53.57499999726881157 ) ) ;
#14429 = EDGE_CURVE ( 'NONE', #3560, #27809, #12738, .T. ) ;
#14430 = FACE_OUTER_BOUND ( 'NONE', #19132, .T. ) ;
#14431 = CARTESIAN_POINT ( 'NONE',  ( -9.295050272127044266, 31.92148437608393508, 9.295050272127047819 ) ) ;
#14432 = ORIENTED_EDGE ( 'NONE', *, *, #13459, .F. ) ;
#14433 = CARTESIAN_POINT ( 'NONE',  ( 65.00000000000000000, 38.96601562608393721, -13.14518615778179544 ) ) ;
#14434 = CARTESIAN_POINT ( 'NONE',  ( 13.57481594606304576, 32.76484375216787015, -1.662435489736055892E-15 ) ) ;
#14435 = CARTESIAN_POINT ( 'NONE',  ( 2.493653234604083739E-15, 39.61093749999999147, 13.57481594606304576 ) ) ;
#14436 = ORIENTED_EDGE ( 'NONE', *, *, #14042, .F. ) ;
#14437 = CARTESIAN_POINT ( 'NONE',  ( 70.62287287157795390, 37.27929687499999289, 13.57481594606297115 ) ) ;
#14438 = LINE ( 'NONE', #6045, #22261 ) ;
#14439 = LINE ( 'NONE', #23156, #21808 ) ;
#14440 = CLOSED_SHELL ( 'NONE', ( #19809, #8129, #15389, #1600, #2032, #13509, #16799, #26605, #13109, #9984, #11184, #12179, #22755, #10536, #23450, #17122, #16804, #3928, #3055, #4118, #25810 ) ) ;
#14441 = AXIS2_PLACEMENT_3D ( 'NONE', #19698, #8866, #17558 ) ;
#14442 = CARTESIAN_POINT ( 'NONE',  ( 124.3771271284221314, 34.10429687716786873, 13.57481594606304753 ) ) ;
#14443 = CARTESIAN_POINT ( 'NONE',  ( 99.99999999999998579, 102.6397644303321215, -44.00000000546237544 ) ) ;
#14444 = CARTESIAN_POINT ( 'NONE',  ( 13.57481594606304576, 31.97109375216787441, -1.662435489736055892E-15 ) ) ;
#14445 = CARTESIAN_POINT ( 'NONE',  ( 189.5550856135277229, 37.72578125108395142, 13.14518615778179722 ) ) ;
#14446 = ORIENTED_EDGE ( 'NONE', *, *, #2887, .T. ) ;
#14447 = CARTESIAN_POINT ( 'NONE',  ( 96.84719886470459471, 3.152801135295383084, 14.56250000136559208 ) ) ;
#14448 = CARTESIAN_POINT ( 'NONE',  ( 96.84719886470459471, 3.152801135295383084, 13.56250000136559386 ) ) ;
#14449 = CARTESIAN_POINT ( 'NONE',  ( 5.622872871577780707, 38.37070312499999858, -13.57481594606313990 ) ) ;
#14450 = DIRECTION ( 'NONE',  ( 0.000000000000000000, 0.000000000000000000, 1.000000000000000000 ) ) ;
#14451 = LINE ( 'NONE', #8045, #22627 ) ;
#14452 = CARTESIAN_POINT ( 'NONE',  ( 135.6228728715779823, 40.05742187716787583, -13.57481594606294095 ) ) ;
#14453 = CARTESIAN_POINT ( 'NONE',  ( -5.444914386472299306, 40.10703125108393152, 13.14518615778179722 ) ) ;
#14454 = CARTESIAN_POINT ( 'NONE',  ( 97.92893218813456713, 80.81250000000000000, -5.000000000000067502 ) ) ;
#14455 = CARTESIAN_POINT ( 'NONE',  ( 13.45411265623082109, 36.00000000000000000, 0.6772748633563333565 ) ) ;
#14456 = CARTESIAN_POINT ( 'NONE',  ( 99.99999999999995737, 82.75000000000000000, -5.000000000000018652 ) ) ;
#14457 = CARTESIAN_POINT ( 'NONE',  ( 124.3771271284221314, 32.11992187499999574, -13.57481594606304753 ) ) ;
#14458 = ORIENTED_EDGE ( 'NONE', *, *, #7410, .F. ) ;
#14459 = EDGE_LOOP ( 'NONE', ( #1570, #4473, #22230, #24737 ) ) ;
#14460 = CARTESIAN_POINT ( 'NONE',  ( 70.62287287157801074, 36.78320312499999289, -13.57481594606290898 ) ) ;
#14461 = CARTESIAN_POINT ( 'NONE',  ( -5.622872871577873077, 38.76757812500000000, 13.57481594606304753 ) ) ;
#14462 = CARTESIAN_POINT ( 'NONE',  ( -8.312177448680279460E-16, 32.16953125216787157, -13.57481594606304576 ) ) ;
#14463 = EDGE_LOOP ( 'NONE', ( #12611, #578, #8368, #5919 ) ) ;
#14464 = CARTESIAN_POINT ( 'NONE',  ( 97.92893218813451028, -4.999999999999989342, 4.312500002731185056 ) ) ;
#14465 = CARTESIAN_POINT ( 'NONE',  ( 130.0000000000000000, 39.36289062608393152, 13.14518615778179544 ) ) ;
#14466 = CARTESIAN_POINT ( 'NONE',  ( 55.70494972787295751, 35.69179687608393436, -9.295050272127046043 ) ) ;
#14467 = B_SPLINE_CURVE_WITH_KNOTS ( 'NONE', 3,
 ( #15712, #15990, #20284, #24705, #11567, #770, #11138, #4904, #9444, #21613, #13566, #2765, #23748, #18143, #26857, #19853, #7303, #5185, #340, #13848, #22573, #3040, #19326, #28030, #8496, #24276, #25887, #20149, #15030, #4224, #11429 ),
 .UNSPECIFIED., .F., .F.,
 ( 4, 2, 2, 2, 2, 2, 2, 2, 2, 2, 1, 2, 2, 2, 2, 4 ),
 ( 0.000000000000000000, 0.001647793485000502694, 0.003295586970001005388, 0.004943380455001507648, 0.005767277197501759212, 0.006591173940002010775, 0.008238967425002545128, 0.009886760910003079481, 0.01318234788000417941, 0.01483014136500472938, 0.01647793485000527761, 0.01812572833500582931, 0.01977352182000637754, 0.02306910879000747400, 0.02471690227500801876, 0.02636469576000856352 ),
 .UNSPECIFIED. ) ;
#14468 = DIRECTION ( 'NONE',  ( 0.000000000000000000, -0.000000000000000000, 1.000000000000000000 ) ) ;
#14469 = CARTESIAN_POINT ( 'NONE',  ( -9.295050272127044266, 34.30273437608393294, 9.295050272127047819 ) ) ;
#14470 = DIRECTION ( 'NONE',  ( 0.000000000000000000, 0.000000000000000000, 1.000000000000000000 ) ) ;
#14471 = CARTESIAN_POINT ( 'NONE',  ( 101.0355339059327378, 123.7500000021849615, 2.499999999999977796 ) ) ;
#14472 = DIRECTION ( 'NONE',  ( 0.000000000000000000, 0.000000000000000000, 1.000000000000000000 ) ) ;
#14473 = DIRECTION ( 'NONE',  ( -5.782411586589357392E-17, -0.000000000000000000, -1.000000000000000000 ) ) ;
#14474 = EDGE_CURVE ( 'NONE', #18889, #2926, #8551, .T. ) ;
#14475 = ORIENTED_EDGE ( 'NONE', *, *, #8803, .T. ) ;
#14476 = CARTESIAN_POINT ( 'NONE',  ( 200.6228728715778971, 40.45429687500001137, 13.57481594606306174 ) ) ;
#14477 = CARTESIAN_POINT ( 'NONE',  ( -13.14518615778179900, 38.12265625108393152, -5.444914386472297529 ) ) ;
#14478 = CARTESIAN_POINT ( 'NONE',  ( 97.50000000000000000, 124.1499999999999915, -1.035533905932742416 ) ) ;
#14479 = CARTESIAN_POINT ( 'NONE',  ( 99.99999999999998579, 123.6069999999781572, 2.499999999999978684 ) ) ;
#14480 = AXIS2_PLACEMENT_3D ( 'NONE', #22479, #534, #2673 ) ;
#14481 = CARTESIAN_POINT ( 'NONE',  ( 98.53841926354351699, 122.8500000010924680, -1.461580736456474794 ) ) ;
#14482 = DIRECTION ( 'NONE',  ( -0.000000000000000000, -1.000000000000000000, -0.000000000000000000 ) ) ;
#14483 = DIRECTION ( 'NONE',  ( -0.000000000000000000, -0.000000000000000000, -1.000000000000000000 ) ) ;
#14484 = CARTESIAN_POINT ( 'NONE',  ( 95.54126587499996504, 1.387778780781445676E-14, 14.43750000136559208 ) ) ;
#14485 = CARTESIAN_POINT ( 'NONE',  ( 102.1631189606246295, 103.3426043859339103, -47.90000000546238113 ) ) ;
#14486 = CARTESIAN_POINT ( 'NONE',  ( 97.83688103937537051, 103.3426043859339103, -50.09999999453764019 ) ) ;
#14487 = CARTESIAN_POINT ( 'NONE',  ( 5.444914386472297529, 32.56640625108394005, -13.14518615778179900 ) ) ;
#14488 = CARTESIAN_POINT ( 'NONE',  ( 13.14518615778179722, 33.06250000108393294, -5.444914386472297529 ) ) ;
#14489 = CARTESIAN_POINT ( 'NONE',  ( -9.598844408820458085, 33.06250000216787299, -9.598844408820458085 ) ) ;
#14490 = CARTESIAN_POINT ( 'NONE',  ( 189.3771271284221882, 36.48554687716787726, 13.57481594606311504 ) ) ;
#14491 = CARTESIAN_POINT ( 'NONE',  ( 101.8468681455906903, 84.37500000136562051, -4.458734125000016313 ) ) ;
#14492 = CARTESIAN_POINT ( 'NONE',  ( 51.85481384221820633, 38.37070312608393152, 0.000000000000000000 ) ) ;
#14493 = CARTESIAN_POINT ( 'NONE',  ( 108.0825317500000011, 107.3738262389971538, -50.47500000273118559 ) ) ;
#14494 = CARTESIAN_POINT ( 'NONE',  ( 94.33688103937535629, 105.8855032339526758, -46.80000000000001847 ) ) ;
#14495 = CARTESIAN_POINT ( 'NONE',  ( 97.93301269999999192, 123.0000000010925163, 0.8561741729129329626 ) ) ;
#14496 = FACE_OUTER_BOUND ( 'NONE', #17985, .T. ) ;
#14497 = CARTESIAN_POINT ( 'NONE',  ( 99.99999999999997158, 102.6397644303321215, -51.99999999453763877 ) ) ;
#14498 = CARTESIAN_POINT ( 'NONE',  ( 139.5988444088204687, 40.50390624999999289, 9.598844408820456309 ) ) ;
#14499 = EDGE_LOOP ( 'NONE', ( #25346, #13113, #20338, #20697 ) ) ;
#14500 = DIRECTION ( 'NONE',  ( 0.000000000000000000, 0.000000000000000000, 1.000000000000000000 ) ) ;
#14501 = CARTESIAN_POINT ( 'NONE',  ( 5.444914386472302859, 40.20625000108394431, 13.14518615778179189 ) ) ;
#14502 = CARTESIAN_POINT ( 'NONE',  ( 9.598844408820459861, 39.01562500216787299, 9.598844408820456309 ) ) ;
#14503 = CARTESIAN_POINT ( 'NONE',  ( 130.0000000000000000, 40.35507812608393152, -13.14518615778179544 ) ) ;
#14504 = CARTESIAN_POINT ( 'NONE',  ( 78.57481594606304043, 36.78320312716786589, -5.622872871577873077 ) ) ;
#14505 = VECTOR ( 'NONE', #16933, 1000.000000000000000 ) ;
#14506 = CARTESIAN_POINT ( 'NONE',  ( 99.99999999999997158, 101.5015231886685854, -53.12499999726883004 ) ) ;
#14507 = CARTESIAN_POINT ( 'NONE',  ( 9.598844408820459861, 35.84062500216786873, 9.598844408820456309 ) ) ;
#14508 = ORIENTED_EDGE ( 'NONE', *, *, #18939, .T. ) ;
#14509 = CARTESIAN_POINT ( 'NONE',  ( 94.99999999999995737, 2.071067811865491048, 8.937500000000000000 ) ) ;
#14510 = CARTESIAN_POINT ( 'NONE',  ( 94.99999999999997158, 2.071067811865471953, 1.937500000000000888 ) ) ;
#14511 = CARTESIAN_POINT ( 'NONE',  ( -5.444914386472299306, 33.75703125108393721, 13.14518615778179722 ) ) ;
#14512 = CARTESIAN_POINT ( 'NONE',  ( 208.1451861577818079, 40.15664062608393436, -1.609821015232357215E-15 ) ) ;
#14513 = EDGE_CURVE ( 'NONE', #3914, #22274, #15671, .T. ) ;
#14514 = CARTESIAN_POINT ( 'NONE',  ( 104.9999999999999716, 1.449011120738813565E-14, 13.62500000273118417 ) ) ;
#14515 = CARTESIAN_POINT ( 'NONE',  ( 143.1451861577818363, 36.93203125108394147, 5.444914386472293977 ) ) ;
#14516 = CARTESIAN_POINT ( 'NONE',  ( -5.444914386472297529, 33.45937500108394147, -13.14518615778179900 ) ) ;
#14517 = EDGE_CURVE ( 'NONE', #18933, #8752, #9000, .T. ) ;
#14518 = CARTESIAN_POINT ( 'NONE',  ( -15.00000000000000000, 50.00000000000000000, 10.00000000000000000 ) ) ;
#14519 = CARTESIAN_POINT ( 'NONE',  ( -20.00000000000000000, 80.00000000000000000, 13.00000000000000178 ) ) ;
#14520 = CARTESIAN_POINT ( 'NONE',  ( 97.50236033167492167, 102.3130555110000159, -48.97500000273119269 ) ) ;
#14521 = CARTESIAN_POINT ( 'NONE',  ( 101.4615807364564546, 123.4500000010924765, 1.461580736456455476 ) ) ;
#14522 = CARTESIAN_POINT ( 'NONE',  ( 195.0000000000000000, 36.83281249999999574, -13.57481594606304576 ) ) ;
#14523 = SHAPE_DEFINITION_REPRESENTATION ( #18345, #19878 ) ;
#14524 = CARTESIAN_POINT ( 'NONE',  ( 128.9781962812409120, 36.00000000000000711, 13.11239906893445095 ) ) ;
#14525 = CARTESIAN_POINT ( 'NONE',  ( 95.54126587499995082, 1.846868145590750077, 1.625000001365592972 ) ) ;
#14526 = CARTESIAN_POINT ( 'NONE',  ( 51.85481384221820633, 38.22187500108393010, 5.444914386472304635 ) ) ;
#14527 = CARTESIAN_POINT ( 'NONE',  ( 99.99999999999995737, -4.458734124999988779, 7.687500001365592084 ) ) ;
#14528 = CARTESIAN_POINT ( 'NONE',  ( 102.1631189606246295, 116.6573956140660897, -51.10000000546237686 ) ) ;
#14529 = CARTESIAN_POINT ( 'NONE',  ( 98.15313185440925281, 93.87499999863439371, -4.458734124999994997 ) ) ;
#14530 = CARTESIAN_POINT ( 'NONE',  ( 99.99999999999995737, 85.00000000000000000, 2.999999999999990674 ) ) ;
#14531 = VECTOR ( 'NONE', #18331, 1000.000000000000000 ) ;
#14532 = DIRECTION ( 'NONE',  ( 5.782411586589357392E-17, -0.000000000000000000, 1.000000000000000000 ) ) ;
#14533 = CARTESIAN_POINT ( 'NONE',  ( 6.944423624769117787, 31.75150628229955529, -11.16113343896966370 ) ) ;
#14534 = ADVANCED_FACE ( 'NONE', ( #8269 ), #23256, .F. ) ;
#14535 = ORIENTED_EDGE ( 'NONE', *, *, #10885, .T. ) ;
#14536 = CARTESIAN_POINT ( 'NONE',  ( 96.84719886470459471, 81.56250000136559208, -3.152801135295383084 ) ) ;
#14537 = CARTESIAN_POINT ( 'NONE',  ( 98.23223304703363112, 124.2000000021849502, -1.767766952966370209 ) ) ;
#14538 = ORIENTED_EDGE ( 'NONE', *, *, #80, .T. ) ;
#14539 = ORIENTED_EDGE ( 'NONE', *, *, #4744, .F. ) ;
#14540 =( BOUNDED_CURVE ( )  B_SPLINE_CURVE ( 2, ( #1069, #26867, #11293, #24716, #4914, #5194, #13574, #9738, #2773 ),
 .UNSPECIFIED., .F., .F. ) 
 B_SPLINE_CURVE_WITH_KNOTS ( ( 3, 2, 2, 2, 3 ),
 ( 0.4791666666666667962, 0.4895833333333333703, 0.5000000000000000000, 0.5104166666666665186, 0.5208333333333332593 ),
 .UNSPECIFIED. ) 
 CURVE ( )  GEOMETRIC_REPRESENTATION_ITEM ( )  RATIONAL_B_SPLINE_CURVE ( ( 0.9999999999999992228, 0.9238795325112875156, 1.000000000000000000, 0.9238795325112867385, 1.000000000000000000, 0.9238795325112867385, 1.000000000000000000, 0.9238795325112875156, 0.9999999999999992228 ) ) 
 REPRESENTATION_ITEM ( '' )  );
#14541 = DIRECTION ( 'NONE',  ( -0.000000000000000000, 1.000000000000000000, 0.000000000000000000 ) ) ;
#14542 = CARTESIAN_POINT ( 'NONE',  ( 95.54126587499995082, 1.846868145590750077, 6.625000001365592084 ) ) ;
#14543 = EDGE_CURVE ( 'NONE', #20304, #27010, #8423, .T. ) ;
#14544 = ORIENTED_EDGE ( 'NONE', *, *, #1856, .T. ) ;
#14545 = CARTESIAN_POINT ( 'NONE',  ( 106.5389055433251002, 114.7507929638356785, -48.17500000273120264 ) ) ;
#14546 = CARTESIAN_POINT ( 'NONE',  ( -5.444914386472299306, 34.35234375108392868, 13.14518615778179722 ) ) ;
#14547 = CARTESIAN_POINT ( 'NONE',  ( 195.0000000000000000, 38.91640625216786731, 13.57481594606304576 ) ) ;
#14548 = CARTESIAN_POINT ( 'NONE',  ( -13.14518615778179544, 38.96601562608393721, 0.000000000000000000 ) ) ;
#14549 = CARTESIAN_POINT ( 'NONE',  ( 104.9952793366501709, 103.1245878333314465, -48.42500000273120264 ) ) ;
#14550 = CARTESIAN_POINT ( 'NONE',  ( 124.5550856135277087, 39.01562500108394005, -13.14518615778179722 ) ) ;
#14551 = CARTESIAN_POINT ( 'NONE',  ( -9.295050272127046043, 32.51679687608393721, -9.295050272127046043 ) ) ;
#14552 = EDGE_CURVE ( 'NONE', #3810, #19205, #17095, .T. ) ;
#14553 = EDGE_LOOP ( 'NONE', ( #26985, #23038, #27697 ) ) ;
#14554 = CARTESIAN_POINT ( 'NONE',  ( 51.42518405393695957, 36.98164062499999005, -5.622872871577873077 ) ) ;
#14555 = DIRECTION ( 'NONE',  ( 0.000000000000000000, 0.000000000000000000, 1.000000000000000000 ) ) ;
#14556 = EDGE_CURVE ( 'NONE', #13477, #22034, #8406, .T. ) ;
#14557 = CARTESIAN_POINT ( 'NONE',  ( -13.57481594606304753, 37.08085937716787583, -5.622872871577872189 ) ) ;
#14558 = CARTESIAN_POINT ( 'NONE',  ( 103.1528011352953342, -3.152801135295355106, 2.812500001365592528 ) ) ;
#14559 = CARTESIAN_POINT ( 'NONE',  ( 94.99999999999997158, 2.071067811865471953, 4.062500002731185944 ) ) ;
#14560 = CARTESIAN_POINT ( 'NONE',  ( 101.8468681455907046, 4.458734125000016313, 3.375000001365592972 ) ) ;
#14561 = CARTESIAN_POINT ( 'NONE',  ( 101.8468681455907046, 82.37500000136563472, -4.458734125000016313 ) ) ;
#14562 = CARTESIAN_POINT ( 'NONE',  ( 13.14518615778179544, 33.80664062608393294, -1.609821015232357215E-15 ) ) ;
#14563 = CARTESIAN_POINT ( 'NONE',  ( -8.049105076161786076E-16, 39.75976562608394005, -13.14518615778179544 ) ) ;
#14564 = CARTESIAN_POINT ( 'NONE',  ( 0.000000000000000000, 30.99999999999999645, 0.000000000000000000 ) ) ;
#14565 = ORIENTED_EDGE ( 'NONE', *, *, #16531, .T. ) ;
#14566 = DIRECTION ( 'NONE',  ( -0.000000000000000000, 1.000000000000000000, -0.000000000000000000 ) ) ;
#14567 = CARTESIAN_POINT ( 'NONE',  ( 102.0669872999999797, 124.1500000010924794, -9.794112055954760458E-15 ) ) ;
#14568 = CARTESIAN_POINT ( 'NONE',  ( 99.99999999999998579, 94.31249999863440792, 4.458734124999981674 ) ) ;
#14569 = CARTESIAN_POINT ( 'NONE',  ( 65.00000000000000000, -7.395377635281828788, 13.57481594606303688 ) ) ;
#14570 = CARTESIAN_POINT ( 'NONE',  ( 108.0825317499999869, 112.6261737610028320, -54.77499999726881441 ) ) ;
#14571 = ORIENTED_EDGE ( 'NONE', *, *, #17313, .F. ) ;
#14572 = CARTESIAN_POINT ( 'NONE',  ( 78.14518615778179367, 37.18007812608393436, -1.609821015232357215E-15 ) ) ;
#14573 = CARTESIAN_POINT ( 'NONE',  ( 98.53841926354351699, 123.0500000010924850, -1.461580736456474794 ) ) ;
#14574 = CARTESIAN_POINT ( 'NONE',  ( 130.0000000000000000, 36.03906250000000000, -13.57481594606304576 ) ) ;
#14575 = ORIENTED_EDGE ( 'NONE', *, *, #21090, .F. ) ;
#14576 = CARTESIAN_POINT ( 'NONE',  ( 99.99999999999995737, 5.000000000000018652, 1.875000002731185056 ) ) ;
#14577 = FACE_OUTER_BOUND ( 'NONE', #1406, .T. ) ;
#14578 = CARTESIAN_POINT ( 'NONE',  ( 108.0825317500000153, 110.0000000000000000, -54.12500000273119838 ) ) ;
#14579 = CARTESIAN_POINT ( 'NONE',  ( 116.4251840539369454, 33.11210937716786873, -5.622872871577873077 ) ) ;
#14580 =( BOUNDED_SURFACE ( )  B_SPLINE_SURFACE ( 3, 2, ( 
 ( #24134, #4610, #13268 ),
 ( #20002, #914, #11136 ),
 ( #15988, #5325, #24559 ),
 ( #11425, #6878, #24844 ),
 ( #16136, #15709, #22423 ),
 ( #15850, #2894, #2619 ),
 ( #13987, #9584, #13563 ),
 ( #17996, #18288, #5041 ),
 ( #19851, #22571, #26561 ),
 ( #338, #9300, #13705 ),
 ( #11282, #3037, #26994 ),
 ( #482, #11707, #22712 ),
 ( #7440, #9025, #26705 ),
 ( #9164, #17717, #26419 ),
 ( #20431, #15563, #17856 ),
 ( #2762, #11563, #7013 ),
 ( #24273, #4754, #13414 ),
 ( #22140, #24411, #766 ),
 ( #20144, #4901, #22286 ),
 ( #9440, #625, #7154 ) ),
 .UNSPECIFIED., .F., .F., .F. ) 
 B_SPLINE_SURFACE_WITH_KNOTS ( ( 4, 2, 2, 2, 2, 2, 2, 2, 2, 4 ),
 ( 3, 3 ),
 ( 0.009073803551359473779, 0.01139250602759182655, 0.01371120850382417933, 0.01602991098005653037, 0.01834861345628888488, 0.01950796469440506387, 0.02066731593252123939, 0.02298601840875359043, 0.02530472088498594146, 0.02762342336121829597 ),
 ( 0.000000000000000000, 1.000000000000000000 ),
 .UNSPECIFIED. ) 
 GEOMETRIC_REPRESENTATION_ITEM ( )  RATIONAL_B_SPLINE_SURFACE ( (
 ( 1.000000000000000000, 0.7071067811865476838, 1.000000000000000000),
 ( 1.000000000000000000, 0.7344871497828565632, 1.000000000000000000),
 ( 1.000000000000000000, 0.7612510203319298174, 1.000000000000000000),
 ( 1.000000000000000000, 0.8116663633843581582, 1.000000000000000000),
 ( 1.000000000000000000, 0.8353358059749911302, 1.000000000000000000),
 ( 1.000000000000000000, 0.8764699612587956157, 1.000000000000000000),
 ( 1.000000000000000000, 0.8939017358718738260, 1.000000000000000000),
 ( 1.000000000000000000, 0.9185314935647551637, 1.000000000000000000),
 ( 1.000000000000000000, 0.9256439951239044950, 1.000000000000000000),
 ( 1.000000000000000000, 0.9261623622476727880, 1.000000000000000000),
 ( 1.000000000000000000, 0.9246301385978410448, 1.000000000000000000),
 ( 1.000000000000000000, 0.9183304321348457755, 1.000000000000000000),
 ( 1.000000000000000000, 0.9135987334167977592, 1.000000000000000000),
 ( 1.000000000000000000, 0.8954110486040547379, 1.000000000000000000),
 ( 1.000000000000000000, 0.8779877431162230739, 1.000000000000000000),
 ( 1.000000000000000000, 0.8366182664711283579, 1.000000000000000000),
 ( 1.000000000000000000, 0.8126941604016590937, 1.000000000000000000),
 ( 1.000000000000000000, 0.7617527316304667506, 1.000000000000000000),
 ( 1.000000000000000000, 0.7347103785792968855, 1.000000000000000000),
 ( 1.000000000000000000, 0.7071067811865466846, 1.000000000000000000) ) ) 
 REPRESENTATION_ITEM ( '' )  SURFACE ( )  );
#14581 = DIRECTION ( 'NONE',  ( 0.000000000000000000, 0.000000000000000000, 1.000000000000000000 ) ) ;
#14582 = CARTESIAN_POINT ( 'NONE',  ( 107.0000000000000000, 112.2744378736303190, -47.39999999453763735 ) ) ;
#14583 = EDGE_CURVE ( 'NONE', #26363, #6724, #8480, .T. ) ;
#14584 = CARTESIAN_POINT ( 'NONE',  ( 200.4449143864723055, 38.12265625108393152, -13.14518615778179900 ) ) ;
#14585 = ORIENTED_EDGE ( 'NONE', *, *, #9159, .F. ) ;
#14586 = CARTESIAN_POINT ( 'NONE',  ( 104.4587341249999781, -1.846868145590721655, 13.12500000136559208 ) ) ;
#14587 = CARTESIAN_POINT ( 'NONE',  ( 96.46446609406726225, 92.49999999726880162, 3.535533905932723986 ) ) ;
#14588 = CARTESIAN_POINT ( 'NONE',  ( 96.84719886470459471, 84.31250000136560629, -3.152801135295383084 ) ) ;
#14589 = CARTESIAN_POINT ( 'NONE',  ( 13.57481594606304931, 34.30273437716787299, 5.622872871577868636 ) ) ;
#14590 = CARTESIAN_POINT ( 'NONE',  ( 102.0019607628501888, 122.9999999999999858, 1.533685529140143444 ) ) ;
#14591 = CIRCLE ( 'NONE', #19162, 4.999999999999997335 ) ;
#14592 = CARTESIAN_POINT ( 'NONE',  ( 99.99999999999995737, 85.00000000000000000, -1.387778780781445676E-14 ) ) ;
#14593 = CARTESIAN_POINT ( 'NONE',  ( 7.754123975994470896, 35.99999999999999289, 10.77549638133777421 ) ) ;
#14594 = SPHERICAL_SURFACE ( 'NONE', #8586, 5.000000000000000000 ) ;
#14595 = CARTESIAN_POINT ( 'NONE',  ( 91.91746824999998466, 110.0000000000000000, -49.62499999726882294 ) ) ;
#14596 = VERTEX_POINT ( 'NONE', #16958 ) ;
#14597 = PRODUCT_DEFINITION_CONTEXT ( 'detailed design', #25524, 'design' ) ;
#14598 = CARTESIAN_POINT ( 'NONE',  ( -13.14518615778179189, 32.07031250108393294, 5.444914386472304635 ) ) ;
#14599 = CARTESIAN_POINT ( 'NONE',  ( 13.57481594606304753, 32.02070312716787015, -5.622872871577873077 ) ) ;
#14600 = CARTESIAN_POINT ( 'NONE',  ( 104.9999999999999574, -2.071067811865462627, 4.562500002731185944 ) ) ;
#14601 = CARTESIAN_POINT ( 'NONE',  ( 124.5550856135277087, 40.10703125108393152, 13.14518615778179722 ) ) ;
#14602 = CARTESIAN_POINT ( 'NONE',  ( 78.14518615778179367, 35.34453125108392868, 5.444914386472293977 ) ) ;
#14603 = VECTOR ( 'NONE', #19185, 1000.000000000000000 ) ;
#14604 = DIRECTION ( 'NONE',  ( -1.000000000000000000, 0.000000000000000000, 0.000000000000000000 ) ) ;
#14605 = CARTESIAN_POINT ( 'NONE',  ( 5.444914386472297529, 34.74921875108394431, -13.14518615778179900 ) ) ;
#14606 = CARTESIAN_POINT ( 'NONE',  ( 51.42518405393695957, 36.23749999999999005, 0.000000000000000000 ) ) ;
#14607 = CARTESIAN_POINT ( 'NONE',  ( 193.9781962812411393, 35.99999999999997158, 13.11239906893446516 ) ) ;
#14608 = ORIENTED_EDGE ( 'NONE', *, *, #1945, .F. ) ;
#14609 = DIRECTION ( 'NONE',  ( 1.000000000000000000, -0.000000000000000000, -7.228014483236696740E-18 ) ) ;
#14610 = CARTESIAN_POINT ( 'NONE',  ( 13.14518615778179900, 38.61875000108393152, -5.444914386472297529 ) ) ;
#14611 = CARTESIAN_POINT ( 'NONE',  ( 143.4955014123171395, 36.00000000000000000, -0.9550757908099576365 ) ) ;
#14612 = CARTESIAN_POINT ( 'NONE',  ( 99.99999999999998579, 123.6000000000000085, 2.499999999999978684 ) ) ;
#14613 = DIRECTION ( 'NONE',  ( -0.000000000000000000, 1.000000000000000000, -0.000000000000000000 ) ) ;
#14614 = CARTESIAN_POINT ( 'NONE',  ( 99.99999999999998579, 124.5500000010924708, -2.066987299999998751 ) ) ;
#14615 = DIRECTION ( 'NONE',  ( 0.000000000000000000, 1.000000000000000000, 0.000000000000000000 ) ) ;
#14616 = CARTESIAN_POINT ( 'NONE',  ( 95.54126587499996504, 1.387778780781445676E-14, 11.43750000136559208 ) ) ;
#14617 = CARTESIAN_POINT ( 'NONE',  ( 105.0000000000000000, 110.0000000000000000, -45.00000000000000711 ) ) ;
#14618 = ORIENTED_EDGE ( 'NONE', *, *, #18246, .T. ) ;
#14619 = CARTESIAN_POINT ( 'NONE',  ( 107.0000000000000284, 107.7255621263696952, -53.10000000000001563 ) ) ;
#14620 = CARTESIAN_POINT ( 'NONE',  ( 9.295050272127047819, 32.31835937608393294, 9.295050272127046043 ) ) ;
#14621 = CARTESIAN_POINT ( 'NONE',  ( -5.444914386472297529, 34.05468750108393294, -13.14518615778179722 ) ) ;
#14622 = CARTESIAN_POINT ( 'NONE',  ( 13.57481594606304753, 34.40195312716787157, -5.622872871577873077 ) ) ;
#14623 = CARTESIAN_POINT ( 'NONE',  ( 181.4251840539369596, 36.38632812716788578, 5.622872871577880183 ) ) ;
#14624 = CARTESIAN_POINT ( 'NONE',  ( 99.99999999999995737, 80.18750000136559208, -4.458734125000016313 ) ) ;
#14625 = CARTESIAN_POINT ( 'NONE',  ( 55.70494972787295751, 36.88242187608393152, 9.295050272127047819 ) ) ;
#14626 = CARTESIAN_POINT ( 'NONE',  ( 108.0825317500000011, 107.3738262389971538, -46.47500000273117848 ) ) ;
#14627 = LINE ( 'NONE', #8362, #11842 ) ;
#14628 = CARTESIAN_POINT ( 'NONE',  ( 100.8561741729129153, 122.9000000010924936, -2.066987299999999195 ) ) ;
#14629 = CARTESIAN_POINT ( 'NONE',  ( 102.1844659708856540, 123.0000000000000284, 1.259047450927248235 ) ) ;
#14630 = CARTESIAN_POINT ( 'NONE',  ( 93.00000000000000000, 112.2744378736303332, -52.59999999453764019 ) ) ;
#14631 = CARTESIAN_POINT ( 'NONE',  ( 124.5550856135277087, 32.66562500108393863, -13.14518615778179900 ) ) ;
#14632 = ORIENTED_EDGE ( 'NONE', *, *, #13327, .T. ) ;
#14633 = CARTESIAN_POINT ( 'NONE',  ( 2.493653234604083739E-15, 33.26093749999999716, 13.57481594606304576 ) ) ;
#14634 = EDGE_CURVE ( 'NONE', #27806, #7689, #25658, .T. ) ;
#14635 = CARTESIAN_POINT ( 'NONE',  ( 13.14518615778179900, 39.61093750108393863, -5.444914386472297529 ) ) ;
#14636 = CARTESIAN_POINT ( 'NONE',  ( 101.8468681455906903, 81.12500000136559208, -4.458734125000016313 ) ) ;
#14637 = CARTESIAN_POINT ( 'NONE',  ( 143.1451861577818079, 40.15664062608393436, -1.609821015232357215E-15 ) ) ;
#14638 = CARTESIAN_POINT ( 'NONE',  ( 55.40115559117954547, 37.22968750216787726, 9.598844408820459861 ) ) ;
#14639 = CARTESIAN_POINT ( 'NONE',  ( 99.99999999999997158, 101.5015231886685854, -55.12499999726880873 ) ) ;
#14640 = CARTESIAN_POINT ( 'NONE',  ( 13.57481594606304576, 34.35234375216787583, -1.662435489736055892E-15 ) ) ;
#14641 = EDGE_LOOP ( 'NONE', ( #6322, #27013, #6688, #18092 ) ) ;
#14642 = CARTESIAN_POINT ( 'NONE',  ( 104.9999999999999716, 1.449011120738813565E-14, 8.499999999999998224 ) ) ;
#14643 = CARTESIAN_POINT ( 'NONE',  ( -8.312177448680279460E-16, 33.65781249999999147, -13.57481594606304576 ) ) ;
#14644 = CARTESIAN_POINT ( 'NONE',  ( -13.14518615778179189, 32.07031250108393294, 5.444914386472304635 ) ) ;
#14645 = CARTESIAN_POINT ( 'NONE',  ( 195.0000000000000000, 36.38632812608393152, -13.14518615778179544 ) ) ;
#14646 = CARTESIAN_POINT ( 'NONE',  ( 102.0710678118654329, 5.000000000000018652, 13.81250000273118950 ) ) ;
#14647 = CARTESIAN_POINT ( 'NONE',  ( 135.4449143864723339, 37.13046875108393152, -13.14518615778179722 ) ) ;
#14648 = CARTESIAN_POINT ( 'NONE',  ( 181.4251840539369596, 37.92421875216787441, 0.000000000000000000 ) ) ;
#14649 = CARTESIAN_POINT ( 'NONE',  ( 143.5748159460630688, 37.47773437500001137, -5.622872871577873966 ) ) ;
#14650 = CARTESIAN_POINT ( 'NONE',  ( 101.8468681455907330, 94.49999999863439371, -4.458734124999994997 ) ) ;
#14651 = CARTESIAN_POINT ( 'NONE',  ( 55.40115559117954547, 37.13046874999999147, 9.598844408820459861 ) ) ;
#14652 = CARTESIAN_POINT ( 'NONE',  ( 5.444914386472302859, 40.00781250108393294, 13.14518615778179189 ) ) ;
#14653 = CARTESIAN_POINT ( 'NONE',  ( 208.5748159460630120, 39.06523437499998863, -5.622872871577873077 ) ) ;
#14654 = CARTESIAN_POINT ( 'NONE',  ( 59.37712712842198926, 39.56132812500000284, 13.57481594606290720 ) ) ;
#14655 = CARTESIAN_POINT ( 'NONE',  ( 99.99999999999995737, -4.458734124999988779, 1.937500001365591640 ) ) ;
#14656 = CARTESIAN_POINT ( 'NONE',  ( 74.29505027212704249, 38.46992187608393010, 9.295050272127046043 ) ) ;
#14657 = CARTESIAN_POINT ( 'NONE',  ( 96.84719886470459471, -3.152801135295355994, 7.562500001365592084 ) ) ;
#14658 = CARTESIAN_POINT ( 'NONE',  ( 93.00000000000001421, 112.2744378736303332, -48.60000000546237686 ) ) ;
#14659 = CARTESIAN_POINT ( 'NONE',  ( 95.54126587499999346, 93.12499999863439371, 1.846868145590722543 ) ) ;
#14660 = DIRECTION ( 'NONE',  ( 0.000000000000000000, 1.000000000000000000, 0.000000000000000000 ) ) ;
#14661 = CARTESIAN_POINT ( 'NONE',  ( -13.57481594606304576, 40.20624999999999005, 0.000000000000000000 ) ) ;
#14662 = CARTESIAN_POINT ( 'NONE',  ( 130.0000000000000000, 40.15664062608393436, 13.14518615778179544 ) ) ;
#14663 = VERTEX_POINT ( 'NONE', #23670 ) ;
#14664 = CARTESIAN_POINT ( 'NONE',  ( 98.15313185440925281, 83.87500000136560629, 4.458734124999987891 ) ) ;
#14665 = CARTESIAN_POINT ( 'NONE',  ( 103.1528011352953484, 90.43749999863440792, -3.152801135295366208 ) ) ;
#14666 = VERTEX_POINT ( 'NONE', #13664 ) ;
#14667 = VECTOR ( 'NONE', #20652, 1000.000000000000000 ) ;
#14668 = EDGE_CURVE ( 'NONE', #10173, #14872, #19957, .T. ) ;
#14669 = ORIENTED_EDGE ( 'NONE', *, *, #25348, .T. ) ;
#14670 = CARTESIAN_POINT ( 'NONE',  ( 9.598844408820459861, 32.56640625000000000, 9.598844408820456309 ) ) ;
#14671 = CARTESIAN_POINT ( 'NONE',  ( 104.4587341249999781, 1.846868145590750299, 7.250000001365591196 ) ) ;
#14672 = EDGE_LOOP ( 'NONE', ( #11730, #17395, #17721 ) ) ;
#14673 = CARTESIAN_POINT ( 'NONE',  ( 91.91746824999998466, 107.3738262389971538, -49.27500000273118985 ) ) ;
#14674 = CARTESIAN_POINT ( 'NONE',  ( -13.14518615778179900, 34.15390625108393863, -5.444914386472297529 ) ) ;
#14675 = CARTESIAN_POINT ( 'NONE',  ( 185.4011555911795313, 37.03125000216787299, -9.598844408820458085 ) ) ;
#14676 = CARTESIAN_POINT ( 'NONE',  ( 99.99999999999997158, 117.3602355696678643, -53.50000000000001421 ) ) ;
#14677 = CYLINDRICAL_SURFACE ( 'NONE', #4403, 13.57481594606304576 ) ;
#14678 = CARTESIAN_POINT ( 'NONE',  ( 197.2761468445513060, 51.46995505939148785, 14.99999999999995559 ) ) ;
#14679 = CARTESIAN_POINT ( 'NONE',  ( 143.1451861577818079, 37.97382812608393721, -1.609821015232357215E-15 ) ) ;
#14680 = CARTESIAN_POINT ( 'NONE',  ( -5.444914386472297529, 31.67343750108393863, -13.14518615778179900 ) ) ;
#14681 = ORIENTED_EDGE ( 'NONE', *, *, #24668, .F. ) ;
#14682 = CARTESIAN_POINT ( 'NONE',  ( 51.42518405393695957, 36.28710937499999289, 5.622872871577880183 ) ) ;
#14683 = CARTESIAN_POINT ( 'NONE',  ( 99.99999999999998579, 129.0000000000000000, -5.204170427930421283E-15 ) ) ;
#14684 = AXIS2_PLACEMENT_3D ( 'NONE', #6864, #26407, #15551 ) ;
#14685 = CARTESIAN_POINT ( 'NONE',  ( 207.2511908804448240, 36.00000000000000711, 5.405483146087288304 ) ) ;
#14686 = EDGE_CURVE ( 'NONE', #19382, #11554, #20890, .T. ) ;
#14687 = CARTESIAN_POINT ( 'NONE',  ( 95.54126587499995082, 1.846868145590750077, 5.375000001365592972 ) ) ;
#14688 = CARTESIAN_POINT ( 'NONE',  ( 13.14518615778179900, 34.05468750108394005, -5.444914386472297529 ) ) ;
#14689 = CARTESIAN_POINT ( 'NONE',  ( 104.4587341249999781, -1.846868145590721655, 4.125000001365592084 ) ) ;
#14690 = CARTESIAN_POINT ( 'NONE',  ( -9.180175813647991845, 50.00000000000000000, -9.999999999999998224 ) ) ;
#14691 = CARTESIAN_POINT ( 'NONE',  ( -5.444914386472299306, 32.76484375108393010, 13.14518615778179722 ) ) ;
#14692 = CARTESIAN_POINT ( 'NONE',  ( 5.444914386472302859, 38.61875000108393152, 13.14518615778179189 ) ) ;
#14693 = DIRECTION ( 'NONE',  ( 1.000000000000000000, 0.000000000000000000, 0.000000000000000000 ) ) ;
#14694 = ORIENTED_EDGE ( 'NONE', *, *, #27950, .F. ) ;
#14695 = CARTESIAN_POINT ( 'NONE',  ( -9.295050272127046043, 31.92148437608393508, -9.295050272127046043 ) ) ;
#14696 =( BOUNDED_CURVE ( )  B_SPLINE_CURVE ( 2, ( #4821, #26483, #4964, #13626, #20911, #9785, #25459, #27201, #7653 ),
 .UNSPECIFIED., .F., .F. ) 
 B_SPLINE_CURVE_WITH_KNOTS ( ( 3, 2, 2, 2, 3 ),
 ( 0.3125000000000002220, 0.3229166666666668517, 0.3333333333333334259, 0.3437500000000000555, 0.3541666666666666852 ),
 .UNSPECIFIED. ) 
 CURVE ( )  GEOMETRIC_REPRESENTATION_ITEM ( )  RATIONAL_B_SPLINE_CURVE ( ( 0.9999999999999983347, 0.9238795325112884038, 1.000000000000000000, 0.9238795325112867385, 1.000000000000000000, 0.9238795325112867385, 1.000000000000000000, 0.9238795325112867385, 1.000000000000000000 ) ) 
 REPRESENTATION_ITEM ( '' )  );
#14698 = EDGE_CURVE ( 'NONE', #7889, #13118, #7692, .T. ) ;
#14697 = CARTESIAN_POINT ( 'NONE',  ( 99.99999999999997158, 102.6397644303321215, -53.99999999453763877 ) ) ;
#14699 = CARTESIAN_POINT ( 'NONE',  ( 104.4587341249999781, 93.56249999863440792, -6.938893903907228378E-15 ) ) ;
#14700 = CARTESIAN_POINT ( 'NONE',  ( 13.57481594606304753, 32.02070312716787015, -5.622872871577873966 ) ) ;
#14701 = CARTESIAN_POINT ( 'NONE',  ( 100.6702820041304136, 123.0000000000000142, -2.125135801581156336 ) ) ;
#14702 = EDGE_CURVE ( 'NONE', #10337, #16728, #18095, .T. ) ;
#14703 = CARTESIAN_POINT ( 'NONE',  ( 96.46446609406726225, 93.37500000000000000, -3.535533905932738197 ) ) ;
#14704 = EDGE_LOOP ( 'NONE', ( #17891, #16556, #4417, #25582 ) ) ;
#14705 = CARTESIAN_POINT ( 'NONE',  ( 70.44491438647229131, 37.32890625108393579, -13.14518615778179722 ) ) ;
#14706 = EDGE_CURVE ( 'NONE', #16151, #3976, #9515, .T. ) ;
#14707 = FACE_OUTER_BOUND ( 'NONE', #21311, .T. ) ;
#14708 = CIRCLE ( 'NONE', #19725, 4.999999999999999112 ) ;
#14709 = ORIENTED_EDGE ( 'NONE', *, *, #19574, .F. ) ;
#14710 = CARTESIAN_POINT ( 'NONE',  ( 103.5355339059327093, 3.535533905932755072, 1.750000002731184834 ) ) ;
#14711 = CARTESIAN_POINT ( 'NONE',  ( 116.4251840539369596, 37.77539062499998579, -5.622872871577872189 ) ) ;
#14712 = FACE_OUTER_BOUND ( 'NONE', #6273, .T. ) ;
#14713 = EDGE_CURVE ( 'NONE', #17592, #1875, #3137, .T. ) ;
#14714 = CARTESIAN_POINT ( 'NONE',  ( 120.4011555911795455, 35.64218750216787868, 9.598844408820459861 ) ) ;
#14715 = CARTESIAN_POINT ( 'NONE',  ( 94.99999999999995737, 1.387778780781445676E-14, 34.79898987322334136 ) ) ;
#14716 = CYLINDRICAL_SURFACE ( 'NONE', #5057, 13.57481594606304576 ) ;
#14717 = CARTESIAN_POINT ( 'NONE',  ( 195.0000000000000000, 38.96601562608393721, -13.14518615778179544 ) ) ;
#14718 = ORIENTED_EDGE ( 'NONE', *, *, #23600, .T. ) ;
#14719 = ORIENTED_EDGE ( 'NONE', *, *, #8283, .F. ) ;
#14720 = CARTESIAN_POINT ( 'NONE',  ( -13.14518615778179544, 40.75195312608393294, 0.000000000000000000 ) ) ;
#14721 =( NAMED_UNIT ( * ) PLANE_ANGLE_UNIT ( ) SI_UNIT ( $, .RADIAN. ) );
#14722 = DIRECTION ( 'NONE',  ( 0.000000000000000000, 0.000000000000000000, -1.000000000000000000 ) ) ;
#14723 = CARTESIAN_POINT ( 'NONE',  ( -9.598844408820458085, 40.10703124999999147, -9.598844408820458085 ) ) ;
#14724 = CARTESIAN_POINT ( 'NONE',  ( 0.000000000000000000, -7.395377635281828788, 0.000000000000000000 ) ) ;
#14725 = CARTESIAN_POINT ( 'NONE',  ( 78.57481594606305464, 39.95820312716787726, -5.622872871577873966 ) ) ;
#14726 = CYLINDRICAL_SURFACE ( 'NONE', #21835, 13.57481594606304576 ) ;
#14727 = DIRECTION ( 'NONE',  ( -0.000000000000000000, -1.000000000000000000, -0.000000000000000000 ) ) ;
#14728 = CARTESIAN_POINT ( 'NONE',  ( 12.25119088044423776, 36.00000000000000711, 5.405483146088369217 ) ) ;
#14729 = PLANE ( 'NONE',  #15388 ) ;
#14730 = CARTESIAN_POINT ( 'NONE',  ( 108.0825317499999869, 107.3738262389971538, -46.72499999726881015 ) ) ;
#14731 = VERTEX_POINT ( 'NONE', #24368 ) ;
#14732 = CARTESIAN_POINT ( 'NONE',  ( -5.622872871577873077, 40.35507812499998437, 13.57481594606304753 ) ) ;
#14733 = CARTESIAN_POINT ( 'NONE',  ( 2.414731522848535132E-15, 39.95820312608393010, 13.14518615778179544 ) ) ;
#14734 = CARTESIAN_POINT ( 'NONE',  ( 97.92893218813451028, -4.999999999999989342, 2.312500002731185500 ) ) ;
#14735 = CARTESIAN_POINT ( 'NONE',  ( 124.5550856135277087, 39.80937500108392868, -13.14518615778179900 ) ) ;
#14736 = CARTESIAN_POINT ( 'NONE',  ( 51.85481384221820633, 36.63437500108393152, 5.444914386472304635 ) ) ;
#14737 = EDGE_CURVE ( 'NONE', #21429, #8864, #4044, .T. ) ;
#14738 = CARTESIAN_POINT ( 'NONE',  ( 181.8548138422182205, 39.16445312608393436, 0.000000000000000000 ) ) ;
#14739 =( BOUNDED_CURVE ( )  B_SPLINE_CURVE ( 2, ( #19165, #27868, #7913, #18617, #10310, #27452, #1516, #23448, #12583 ),
 .UNSPECIFIED., .F., .F. ) 
 B_SPLINE_CURVE_WITH_KNOTS ( ( 3, 2, 2, 2, 3 ),
 ( 0.5500000000000004885, 0.5750000000000003997, 0.6000000000000005329, 0.6250000000000005551, 0.6500000000000005773 ),
 .UNSPECIFIED. ) 
 CURVE ( )  GEOMETRIC_REPRESENTATION_ITEM ( )  RATIONAL_B_SPLINE_CURVE ( ( 0.9999999999999986677, 0.9238795325112880708, 1.000000000000000000, 0.9238795325112867385, 1.000000000000000000, 0.9238795325112867385, 1.000000000000000000, 0.9238795325112850731, 1.000000000000001776 ) ) 
 REPRESENTATION_ITEM ( '' )  );
#14740 = CARTESIAN_POINT ( 'NONE',  ( 99.99999999999995737, 1.387778780781445676E-14, 34.79898987322334136 ) ) ;
#14741 = CARTESIAN_POINT ( 'NONE',  ( 9.295050272127047819, 35.29492187608393294, 9.295050272127046043 ) ) ;
#14742 = LINE ( 'NONE', #25314, #23605 ) ;
#14743 = CARTESIAN_POINT ( 'NONE',  ( -13.57481594606304398, 38.76757812716787299, 5.622872871577880183 ) ) ;
#14744 = CARTESIAN_POINT ( 'NONE',  ( -13.14518615778179189, 39.80937500108392868, 5.444914386472304635 ) ) ;
#14745 = CARTESIAN_POINT ( 'NONE',  ( 3.797451868958014565, 54.08938259242987812, 14.99999999999999645 ) ) ;
#14746 = CARTESIAN_POINT ( 'NONE',  ( 99.99999999999998579, 124.3999999999999915, 2.499999999999978684 ) ) ;
#14747 = CARTESIAN_POINT ( 'NONE',  ( 100.8561741729129153, 122.9000000010924936, -2.066987299999999195 ) ) ;
#14748 = CARTESIAN_POINT ( 'NONE',  ( 99.14382582708708469, 124.1000000010924822, 2.066987299999979655 ) ) ;
#14749 = AXIS2_PLACEMENT_3D ( 'NONE', #21848, #26403, #26111 ) ;
#14750 = FILL_AREA_STYLE ('',( #11034 ) ) ;
#14751 = CARTESIAN_POINT ( 'NONE',  ( 104.9999999999999858, 2.071067811865486608, 12.56249999999999645 ) ) ;
#14752 = CARTESIAN_POINT ( 'NONE',  ( 96.46446609406721961, -3.535533905932727539, 13.25000000273118417 ) ) ;
#14753 = EDGE_LOOP ( 'NONE', ( #1355, #26805, #5775 ) ) ;
#14754 = CARTESIAN_POINT ( 'NONE',  ( 93.00000000000000000, 107.7255621263696668, -53.90000000000000568 ) ) ;
#14755 = CARTESIAN_POINT ( 'NONE',  ( -9.598844408820458085, 40.90078124999999432, -9.598844408820458085 ) ) ;
#14756 = CARTESIAN_POINT ( 'NONE',  ( -13.14518615778179544, 31.82226562608393650, 0.000000000000000000 ) ) ;
#14757 = CARTESIAN_POINT ( 'NONE',  ( 13.57481594606304576, 32.76484375216787015, -1.662435489736055892E-15 ) ) ;
#14758 = CARTESIAN_POINT ( 'NONE',  ( 97.92893218813451028, 5.000000000000018652, 2.937500002731185944 ) ) ;
#14759 = CARTESIAN_POINT ( 'NONE',  ( 99.99999999999995737, 81.18750000136559208, -4.458734125000016313 ) ) ;
#14760 = CARTESIAN_POINT ( 'NONE',  ( 74.29505027212704249, 38.86679687608393863, -9.295050272127046043 ) ) ;
#14761 = CARTESIAN_POINT ( 'NONE',  ( 104.9952793366501851, 116.8754121666685393, -46.07500000273119412 ) ) ;
#14762 = CARTESIAN_POINT ( 'NONE',  ( 107.0000000000000142, 110.0000000000000000, -47.50000000546238255 ) ) ;
#14763 =( REPRESENTATION_RELATIONSHIP ('NONE','NONE', #2411, #14947 ) REPRESENTATION_RELATIONSHIP_WITH_TRANSFORMATION ( #23101 )SHAPE_REPRESENTATION_RELATIONSHIP( ) );
#14764 = CARTESIAN_POINT ( 'NONE',  ( 101.4615807364564546, 122.6500000010924794, -1.461580736456474794 ) ) ;
#14765 = CARTESIAN_POINT ( 'NONE',  ( -9.598844408820458085, 40.90078124999999432, -9.598844408820458085 ) ) ;
#14766 = CARTESIAN_POINT ( 'NONE',  ( 107.0000000000000000, 107.7255621263696668, -51.59999999453763309 ) ) ;
#14767 = CARTESIAN_POINT ( 'NONE',  ( 143.1451861577818079, 32.46718750108393436, -5.444914386472297529 ) ) ;
#14768 = ORIENTED_EDGE ( 'NONE', *, *, #8072, .T. ) ;
#14769 = CARTESIAN_POINT ( 'NONE',  ( -0.7197605961091591009, 53.51499872091923748, -15.00000000000000000 ) ) ;
#14770 = CARTESIAN_POINT ( 'NONE',  ( 2.414731522848535132E-15, 38.56914062608393579, 13.14518615778179544 ) ) ;
#14771 = CARTESIAN_POINT ( 'NONE',  ( 2.493653234604083739E-15, 39.71015625216787015, 13.57481594606304576 ) ) ;
#14772 = CARTESIAN_POINT ( 'NONE',  ( 104.9999999999999858, 95.00000000000000000, -6.938893903907228378E-15 ) ) ;
#14773 = CARTESIAN_POINT ( 'NONE',  ( 55.40115559117954547, 36.43593750216787441, 9.598844408820459861 ) ) ;
#14774 = CYLINDRICAL_SURFACE ( 'NONE', #17516, 5.000000000000004441 ) ;
#14775 = CARTESIAN_POINT ( 'NONE',  ( 9.598844408820459861, 36.63437500216787157, 9.598844408820456309 ) ) ;
#14776 = VERTEX_POINT ( 'NONE', #26664 ) ;
#14777 = CARTESIAN_POINT ( 'NONE',  ( 102.0710678118654329, -4.999999999999989342, 3.312499999999999556 ) ) ;
#14778 = ORIENTED_EDGE ( 'NONE', *, *, #21514, .T. ) ;
#14779 = CARTESIAN_POINT ( 'NONE',  ( 181.8548138422182205, 37.37851562608393863, 0.000000000000000000 ) ) ;
#14780 = CARTESIAN_POINT ( 'NONE',  ( 13.57481594606304576, 35.93984375216787441, -1.662435489736055892E-15 ) ) ;
#14781 = CARTESIAN_POINT ( 'NONE',  ( 120.7049497278729575, 37.47773437608393010, 9.295050272127047819 ) ) ;
#14782 = DIRECTION ( 'NONE',  ( 5.782411586589357392E-17, -0.000000000000000000, 1.000000000000000000 ) ) ;
#14783 = LINE ( 'NONE', #1166, #18615 ) ;
#14784 = CARTESIAN_POINT ( 'NONE',  ( 95.54126587500000767, 92.81249999863440792, -7.484931351350258973E-15 ) ) ;
#14785 = CARTESIAN_POINT ( 'NONE',  ( 51.85481384221820633, 40.75195312608393294, 0.000000000000000000 ) ) ;
#14786 = CARTESIAN_POINT ( 'NONE',  ( 13.14518615778179544, 38.56914062608393579, -1.609821015232357215E-15 ) ) ;
#14787 = CARTESIAN_POINT ( 'NONE',  ( 189.3771271284221314, 36.38632812499999858, 13.57481594606304753 ) ) ;
#14788 = CONTEXT_DEPENDENT_SHAPE_REPRESENTATION ( #19149, #5143 ) ;
#14789 = CARTESIAN_POINT ( 'NONE',  ( 105.0000000000000000, 110.0000000000000000, -145.0000000000000284 ) ) ;
#14790 = CARTESIAN_POINT ( 'NONE',  ( 99.99999999999995737, -4.458734124999988779, 3.937500001365591640 ) ) ;
#14791 = CARTESIAN_POINT ( 'NONE',  ( 65.00000000000000000, 39.16445312608392726, 13.14518615778179544 ) ) ;
#14792 = CARTESIAN_POINT ( 'NONE',  ( 104.4587341249999639, 1.442382525525748735E-14, 5.937500001365592084 ) ) ;
#14793 = CARTESIAN_POINT ( 'NONE',  ( 94.33688103937537051, 114.1144967660473242, -44.70000000546237828 ) ) ;
#14794 = CARTESIAN_POINT ( 'NONE',  ( 104.4587341249999923, 91.24999999863439371, 1.846868145590726318 ) ) ;
#14795 = CARTESIAN_POINT ( 'NONE',  ( 116.4251840539369738, 39.46210937499999005, 5.622872871577880183 ) ) ;
#14796 = CARTESIAN_POINT ( 'NONE',  ( 9.598844408820456309, 39.11484374999999858, -9.598844408820458085 ) ) ;
#14797 = CARTESIAN_POINT ( 'NONE',  ( 143.1451861577818079, 39.56132812608393579, -1.609821015232357215E-15 ) ) ;
#14798 = ORIENTED_EDGE ( 'NONE', *, *, #22894, .T. ) ;
#14799 = CARTESIAN_POINT ( 'NONE',  ( 96.84719886470459471, 83.56250000136560629, -3.152801135295383084 ) ) ;
#14800 = VECTOR ( 'NONE', #11542, 1000.000000000000000 ) ;
#14801 = CARTESIAN_POINT ( 'NONE',  ( 0.000000000000000000, 20.53589838486225361, 0.000000000000000000 ) ) ;
#14802 = EDGE_LOOP ( 'NONE', ( #45, #14024, #23997, #7109 ) ) ;
#14803 = CARTESIAN_POINT ( 'NONE',  ( 104.3262379212492448, 115.9545556584642867, -45.70000000000001705 ) ) ;
#14804 = CARTESIAN_POINT ( 'NONE',  ( 55.70494972787295751, 35.89023437608393152, -9.295050272127046043 ) ) ;
#14805 = ORIENTED_EDGE ( 'NONE', *, *, #25389, .F. ) ;
#14806 = CARTESIAN_POINT ( 'NONE',  ( 104.9999999999999716, 1.449011120738813565E-14, 34.79898987322334136 ) ) ;
#14807 = CARTESIAN_POINT ( 'NONE',  ( 104.4587341249999639, 1.442382525525748735E-14, 4.187500001365592084 ) ) ;
#14808 = ORIENTED_EDGE ( 'NONE', *, *, #9386, .T. ) ;
#14809 = CARTESIAN_POINT ( 'NONE',  ( 9.295050272127046043, 34.10429687608393579, -9.295050272127046043 ) ) ;
#14810 = CARTESIAN_POINT ( 'NONE',  ( -13.14518615778179189, 33.45937500108392726, 5.444914386472304635 ) ) ;
#14811 = CARTESIAN_POINT ( 'NONE',  ( 200.6228728715778686, 36.58476562716787583, 13.57481594606304576 ) ) ;
#14812 = CARTESIAN_POINT ( 'NONE',  ( 13.14518615778179544, 40.15664062608393436, -1.609821015232357215E-15 ) ) ;
#14813 = CARTESIAN_POINT ( 'NONE',  ( 0.000000000000000000, 40.99999999999999289, 0.000000000000000000 ) ) ;
#14814 = CARTESIAN_POINT ( 'NONE',  ( 202.6219635342048662, 54.91641323977498246, 14.99999999999994671 ) ) ;
#14815 = PRODUCT_RELATED_PRODUCT_CATEGORY ( 'part', '', ( #7403 ) ) ;
#14816 = CARTESIAN_POINT ( 'NONE',  ( 139.2950502721270425, 39.46210937608393721, 9.295050272127046043 ) ) ;
#14817 = CARTESIAN_POINT ( 'NONE',  ( -13.14518615778179544, 39.16445312608393436, 0.000000000000000000 ) ) ;
#14818 = ADVANCED_FACE ( 'NONE', ( #5001 ), #19453, .T. ) ;
#14819 = VERTEX_POINT ( 'NONE', #24089 ) ;
#14820 = CARTESIAN_POINT ( 'NONE',  ( 78.57481594606304043, 36.68398437499999432, -5.622872871577873077 ) ) ;
#14821 = CIRCLE ( 'NONE', #17109, 11.57481594606304398 ) ;
#14822 = LINE ( 'NONE', #25672, #21427 ) ;
#14823 = CARTESIAN_POINT ( 'NONE',  ( 94.33688103937537051, 114.1144967660473242, -46.20000000000000284 ) ) ;
#14824 = CARTESIAN_POINT ( 'NONE',  ( 104.4587341249999639, 1.442382525525748735E-14, 3.937500001365591640 ) ) ;
#14825 = CARTESIAN_POINT ( 'NONE',  ( 93.46109445667491400, 105.2492070361643215, -52.92500000273119554 ) ) ;
#14826 = CARTESIAN_POINT ( 'NONE',  ( 95.54126587499996504, 1.846868145590750077, 2.625000001365592084 ) ) ;
#14827 = CARTESIAN_POINT ( 'NONE',  ( 95.54126587499996504, 80.68750000136559208, -1.387778780781445676E-14 ) ) ;
#14828 = CARTESIAN_POINT ( 'NONE',  ( -9.295050272127044266, 32.71523437608393436, 9.295050272127047819 ) ) ;
#14829 = CARTESIAN_POINT ( 'NONE',  ( 103.5355339059327093, 3.535533905932755072, 7.750000002731185056 ) ) ;
#14830 = CARTESIAN_POINT ( 'NONE',  ( 108.0825317500000011, 110.0000000000000000, -48.87499999726882294 ) ) ;
#14831 = ORIENTED_EDGE ( 'NONE', *, *, #11147, .F. ) ;
#14832 =( NAMED_UNIT ( * ) PLANE_ANGLE_UNIT ( ) SI_UNIT ( $, .RADIAN. ) );
#14833 = AXIS2_PLACEMENT_3D ( 'NONE', #24414, #11285, #17181 ) ;
#14834 = CARTESIAN_POINT ( 'NONE',  ( 98.53841926354351699, 124.4500000010924765, -1.461580736456474794 ) ) ;
#14835 = CARTESIAN_POINT ( 'NONE',  ( 93.00000000000000000, 110.0000000000000000, -46.00000000000000711 ) ) ;
#14836 = CARTESIAN_POINT ( 'NONE',  ( 97.92893218813451028, 80.31250000273122680, 4.999999999999989342 ) ) ;
#14837 = CARTESIAN_POINT ( 'NONE',  ( 97.50236033167490746, 102.3130555110000159, -55.47499999726881725 ) ) ;
#14838 = CARTESIAN_POINT ( 'NONE',  ( 130.0000000000000000, 38.12265625216787157, 13.57481594606304576 ) ) ;
#14839 = VECTOR ( 'NONE', #27335, 1000.000000000000000 ) ;
#14840 = ORIENTED_EDGE ( 'NONE', *, *, #9653, .T. ) ;
#14841 = CARTESIAN_POINT ( 'NONE',  ( 65.00000000000000000, 37.77539062608393294, 13.14518615778179544 ) ) ;
#14842 = DIRECTION ( 'NONE',  ( 0.000000000000000000, -0.000000000000000000, -1.000000000000000000 ) ) ;
#14843 = FACE_OUTER_BOUND ( 'NONE', #8738, .T. ) ;
#14844 = EDGE_CURVE ( 'NONE', #10542, #27857, #18270, .T. ) ;
#14845 = EDGE_LOOP ( 'NONE', ( #6928, #17514, #13524, #16380 ) ) ;
#14846 = CARTESIAN_POINT ( 'NONE',  ( 107.0000000000000142, 112.2744378736303332, -52.90000000000001279 ) ) ;
#14847 = CARTESIAN_POINT ( 'NONE',  ( -8.769389672081235432, 50.37710889402508485, -14.99999999999737099 ) ) ;
#14848 = CARTESIAN_POINT ( 'NONE',  ( 102.0669872999999797, 124.3500000010924822, -9.794112055954760458E-15 ) ) ;
#14849 = CARTESIAN_POINT ( 'NONE',  ( 116.4251840539369596, 35.59257812716788294, 5.622872871577880183 ) ) ;
#14850 =( BOUNDED_CURVE ( )  B_SPLINE_CURVE ( 2, ( #11121, #19835, #6857, #4738, #13397, #8113, #26058, #21651, #17362 ),
 .UNSPECIFIED., .F., .T. ) 
 B_SPLINE_CURVE_WITH_KNOTS ( ( 3, 2, 2, 2, 3 ),
 ( 0.1071428571428571092, 0.1160714285714285476, 0.1249999999999999861, 0.1339285714285714246, 0.1428571428571428492 ),
 .UNSPECIFIED. ) 
 CURVE ( )  GEOMETRIC_REPRESENTATION_ITEM ( )  RATIONAL_B_SPLINE_CURVE ( ( 1.000000000000000222, 0.9238795325112865164, 1.000000000000000000, 0.9238795325112867385, 1.000000000000000000, 0.9238795325112867385, 1.000000000000000000, 0.9238795325112867385, 1.000000000000000000 ) ) 
 REPRESENTATION_ITEM ( '' )  );
#14851 = VECTOR ( 'NONE', #19303, 1000.000000000000000 ) ;
#14852 = CARTESIAN_POINT ( 'NONE',  ( 70.44491438647230552, 39.41250000108393436, 13.14518615778179189 ) ) ;
#14853 = ADVANCED_FACE ( 'NONE', ( #4855 ), #17666, .T. ) ;
#14854 = CARTESIAN_POINT ( 'NONE',  ( 99.99999999999995737, 82.37500000273119838, 4.999999999999990230 ) ) ;
#14855 = CARTESIAN_POINT ( 'NONE',  ( 189.5550856135277229, 35.04687500108393294, -13.14518615778179900 ) ) ;
#14856 = ORIENTED_EDGE ( 'NONE', *, *, #6887, .F. ) ;
#14857 = ADVANCED_FACE ( 'NONE', ( #26516 ), #2578, .T. ) ;
#14858 = ORIENTED_EDGE ( 'NONE', *, *, #25852, .T. ) ;
#14859 = ORIENTED_EDGE ( 'NONE', *, *, #24118, .F. ) ;
#14860 = CARTESIAN_POINT ( 'NONE',  ( -5.444914386472299306, 32.76484375108393010, 13.14518615778179722 ) ) ;
#14861 = ADVANCED_FACE ( 'NONE', ( #27092 ), #9544, .F. ) ;
#14862 = LINE ( 'NONE', #18744, #20747 ) ;
#14863 = CARTESIAN_POINT ( 'NONE',  ( 95.00000000000000000, 92.31249999726880162, -2.071067811865479058 ) ) ;
#14864 = CARTESIAN_POINT ( 'NONE',  ( 107.0000000000000142, 110.0000000000000000, -51.50000000546237544 ) ) ;
#14865 = DIRECTION ( 'NONE',  ( -1.003171929053526103E-16, -0.5735764363510443831, -0.8191520442889929088 ) ) ;
#14866 = DIRECTION ( 'NONE',  ( -0.000000000000000000, -0.000000000000000000, -1.000000000000000000 ) ) ;
#14867 = DIRECTION ( 'NONE',  ( 0.000000000000000000, 0.000000000000000000, -1.000000000000000000 ) ) ;
#14868 = DIRECTION ( 'NONE',  ( -0.000000000000000000, -0.000000000000000000, -1.000000000000000000 ) ) ;
#14869 = CARTESIAN_POINT ( 'NONE',  ( 189.5550856135277229, 40.10703125108393152, 13.14518615778179722 ) ) ;
#14870 = CARTESIAN_POINT ( 'NONE',  ( 135.6228728715778971, 32.51679687499999716, 13.57481594606304576 ) ) ;
#14871 = EDGE_CURVE ( 'NONE', #26423, #27592, #22269, .T. ) ;
#14872 = VERTEX_POINT ( 'NONE', #12457 ) ;
#14873 = CARTESIAN_POINT ( 'NONE',  ( 5.622872871577878406, 38.86679687499999858, 13.57481594606304576 ) ) ;
#14874 = CARTESIAN_POINT ( 'NONE',  ( -5.622872871577873077, 31.42539062716787157, -13.57481594606304753 ) ) ;
#14875 = CARTESIAN_POINT ( 'NONE',  ( 102.0710678118654329, -4.999999999999989342, 0.4375000027311854445 ) ) ;
#14876 = CARTESIAN_POINT ( 'NONE',  ( 135.4449143864723055, 35.44375000108393436, 13.14518615778179189 ) ) ;
#14877 = CARTESIAN_POINT ( 'NONE',  ( 78.14518615778179367, 37.82500000108392868, -5.444914386472297529 ) ) ;
#14878 = CARTESIAN_POINT ( 'NONE',  ( 189.5550856135277229, 31.67343750108393863, -13.14518615778179900 ) ) ;
#14879 = DIRECTION ( 'NONE',  ( 0.000000000000000000, 0.000000000000000000, 1.000000000000000000 ) ) ;
#14880 = CARTESIAN_POINT ( 'NONE',  ( 5.444914386472302859, 35.24531250108393010, 13.14518615778179189 ) ) ;
#14881 = CARTESIAN_POINT ( 'NONE',  ( 136.9023785737939534, 51.13402819307182767, -14.99999999999871036 ) ) ;
#14882 = CARTESIAN_POINT ( 'NONE',  ( 99.99999999999995737, 5.000000000000018652, 9.875000002731185944 ) ) ;
#14883 = ADVANCED_FACE ( 'NONE', ( #1804 ), #7396, .T. ) ;
#14884 = CARTESIAN_POINT ( 'NONE',  ( 99.99999999999998579, 110.0000000000000000, -43.00000000000000000 ) ) ;
#14885 = CARTESIAN_POINT ( 'NONE',  ( 13.14518615778179544, 36.98164062608393010, -1.609821015232357215E-15 ) ) ;
#14886 = LINE ( 'NONE', #86, #20669 ) ;
#14887 = CARTESIAN_POINT ( 'NONE',  ( 99.99999999999998579, 124.1000000021849416, -2.499999999999997780 ) ) ;
#14888 = CARTESIAN_POINT ( 'NONE',  ( 103.5355339059327093, -3.535533905932726206, 10.37499999999999822 ) ) ;
#14889 = CARTESIAN_POINT ( 'NONE',  ( 102.0669873000000081, 124.3000000010924708, 0.8561741729129311862 ) ) ;
#14890 = CARTESIAN_POINT ( 'NONE',  ( 98.15313185440925281, 4.458734125000016313, 9.250000001365593860 ) ) ;
#14891 = CARTESIAN_POINT ( 'NONE',  ( 1.907364849565526780E-15, 30.99999999999999645, 15.57481594606304576 ) ) ;
#14892 = CARTESIAN_POINT ( 'NONE',  ( 102.4999999999999716, 123.8500000021849416, 1.035533905932722876 ) ) ;
#14893 = CARTESIAN_POINT ( 'NONE',  ( 103.1528011352953342, 3.152801135295383084, 11.06250000136559208 ) ) ;
#14894 = CARTESIAN_POINT ( 'NONE',  ( 9.295050272127047819, 33.70742187608393436, 9.295050272127046043 ) ) ;
#14895 = EDGE_CURVE ( 'NONE', #19984, #10588, #3861, .T. ) ;
#14896 = CARTESIAN_POINT ( 'NONE',  ( 9.295050272127047819, 38.46992187608393010, 9.295050272127046043 ) ) ;
#14897 = DIRECTION ( 'NONE',  ( -0.000000000000000000, 1.000000000000000000, -0.000000000000000000 ) ) ;
#14898 = CARTESIAN_POINT ( 'NONE',  ( 99.99999999999995737, 83.93750000136560629, 4.458734124999988779 ) ) ;
#14899 = CARTESIAN_POINT ( 'NONE',  ( 59.55508561352770158, 38.22187500108393010, -13.14518615778179900 ) ) ;
#14900 = CARTESIAN_POINT ( 'NONE',  ( 97.50236033167492167, 102.3130555110000159, -48.97500000273119269 ) ) ;
#14901 = CARTESIAN_POINT ( 'NONE',  ( 99.99999999999998579, 110.0000000000000000, -145.0000000000000284 ) ) ;
#14902 = EDGE_LOOP ( 'NONE', ( #18741, #7543, #4000, #25708 ) ) ;
#14903 = CARTESIAN_POINT ( 'NONE',  ( 95.27063293749995410, 1.387778780781445676E-14, 14.28125000204838813 ) ) ;
#14904 = CARTESIAN_POINT ( 'NONE',  ( -20.00000000000000355, 80.00000000000000000, -12.99999999999999822 ) ) ;
#14905 = CARTESIAN_POINT ( 'NONE',  ( 95.67376207875069838, 104.0454443415356991, -50.19999999453764161 ) ) ;
#14906 = CARTESIAN_POINT ( 'NONE',  ( 139.5988444088204687, 39.71015624999999716, 9.598844408820456309 ) ) ;
#14907 = VERTEX_POINT ( 'NONE', #16090 ) ;
#14908 = CARTESIAN_POINT ( 'NONE',  ( 130.0000000000000000, -7.395377635281828788, -1.503427012513233026E-14 ) ) ;
#14909 =( BOUNDED_CURVE ( )  B_SPLINE_CURVE ( 2, ( #21737, #10876, #4202, #6332, #26288, #22012, #17298, #4625, #19585, #6606, #28007 ),
 .UNSPECIFIED., .F., .F. ) 
 B_SPLINE_CURVE_WITH_KNOTS ( ( 3, 2, 2, 2, 2, 3 ),
 ( 0.4999999999999996669, 0.5199999999999996847, 0.5399999999999998135, 0.5599999999999998312, 0.5799999999999998490, 0.5999999999999998668 ),
 .UNSPECIFIED. ) 
 CURVE ( )  GEOMETRIC_REPRESENTATION_ITEM ( )  RATIONAL_B_SPLINE_CURVE ( ( 1.000000000000000888, 0.9510565162951527540, 1.000000000000000000, 0.9510565162951535312, 1.000000000000000000, 0.9510565162951535312, 1.000000000000000000, 0.9510565162951535312, 1.000000000000000000, 0.9510565162951537532, 0.9999999999999997780 ) ) 
 REPRESENTATION_ITEM ( '' )  );
#14910 = CARTESIAN_POINT ( 'NONE',  ( 107.0000000000000000, 110.0000000000000000, -48.00000000000001421 ) ) ;
#14911 = CARTESIAN_POINT ( 'NONE',  ( 98.15313185440925281, 80.25000000136559208, -4.458734125000016313 ) ) ;
#14912 = CARTESIAN_POINT ( 'NONE',  ( 143.1451861577818079, 37.03125000108393294, -5.444914386472297529 ) ) ;
#14913 = CARTESIAN_POINT ( 'NONE',  ( 74.59884440882045453, 38.42031250216787441, -9.598844408820458085 ) ) ;
#14914 = CARTESIAN_POINT ( 'NONE',  ( 93.46109445667489979, 114.7507929638356785, -51.82499999726881867 ) ) ;
#14915 = CARTESIAN_POINT ( 'NONE',  ( -13.57481594606304576, 36.33671875216787583, 0.000000000000000000 ) ) ;
#14916 = VECTOR ( 'NONE', #18915, 999.9999999999997726 ) ;
#14917 = CARTESIAN_POINT ( 'NONE',  ( 97.92893218813451028, -4.999999999999989342, 5.187500000000000888 ) ) ;
#14918 = CARTESIAN_POINT ( 'NONE',  ( 107.0000000000000142, 110.0000000000000000, -47.50000000546238255 ) ) ;
#14919 =( GEOMETRIC_REPRESENTATION_CONTEXT ( 3 ) GLOBAL_UNCERTAINTY_ASSIGNED_CONTEXT ( ( #25165 ) ) GLOBAL_UNIT_ASSIGNED_CONTEXT ( ( #10302, #14721, #19009 ) ) REPRESENTATION_CONTEXT ( 'NONE', 'WORKASPACE' ) );
#14920 = CARTESIAN_POINT ( 'NONE',  ( 204.2950502721270425, 36.88242187608393152, 9.295050272127046043 ) ) ;
#14921 = CARTESIAN_POINT ( 'NONE',  ( -8.312177448680279460E-16, 33.75703125216787726, -13.57481594606304576 ) ) ;
#14922 = EDGE_CURVE ( 'NONE', #5791, #5488, #14742, .T. ) ;
#14923 = CARTESIAN_POINT ( 'NONE',  ( 116.8548138422182205, 39.01562500108393294, 5.444914386472304635 ) ) ;
#14924 = ORIENTED_EDGE ( 'NONE', *, *, #239, .F. ) ;
#14925 = CARTESIAN_POINT ( 'NONE',  ( 97.50000000000000000, 122.7000000021849502, -9.540979117872439019E-15 ) ) ;
#14926 = CARTESIAN_POINT ( 'NONE',  ( 97.92893218813451028, 5.000000000000018652, 4.937500002731185944 ) ) ;
#14927 = CARTESIAN_POINT ( 'NONE',  ( 55.81982418635200816, 55.00000000000000000, 14.99999999999998401 ) ) ;
#14928 = CARTESIAN_POINT ( 'NONE',  ( 104.3262379212492448, 104.0454443415356991, -48.30000000000001137 ) ) ;
#14929 = CARTESIAN_POINT ( 'NONE',  ( -5.444914386472299306, 36.93203125108394147, 13.14518615778179722 ) ) ;
#14930 = CARTESIAN_POINT ( 'NONE',  ( 2.414731522848535132E-15, 39.95820312608393010, 13.14518615778179544 ) ) ;
#14931 = CARTESIAN_POINT ( 'NONE',  ( 204.5988444088204403, 38.32109374999999574, -9.598844408820458085 ) ) ;
#14932 = CARTESIAN_POINT ( 'NONE',  ( 101.8468681455906903, -4.458734124999987891, 4.000000001365592084 ) ) ;
#14933 = CARTESIAN_POINT ( 'NONE',  ( 78.14518615778179367, 37.72578125108393721, 5.444914386472293977 ) ) ;
#14934 = CARTESIAN_POINT ( 'NONE',  ( 103.1528011352953342, 3.152801135295383084, 6.062500001365592084 ) ) ;
#14935 = CARTESIAN_POINT ( 'NONE',  ( 66.13716782454086740, 35.99999999999998579, 13.09590655363602707 ) ) ;
#14936 = CARTESIAN_POINT ( 'NONE',  ( 95.54126587499999346, 94.87499999863440792, 1.846868145590722543 ) ) ;
#14937 = CARTESIAN_POINT ( 'NONE',  ( -8.125303917791095287, 36.00000000000000000, 10.34220695173585902 ) ) ;
#14938 = CARTESIAN_POINT ( 'NONE',  ( 2.493653234604083739E-15, 38.02343749999999289, 13.57481594606304576 ) ) ;
#14939 = CARTESIAN_POINT ( 'NONE',  ( 135.4449143864723055, 39.41250000108393436, 13.14518615778179189 ) ) ;
#14940 = VECTOR ( 'NONE', #13323, 1000.000000000000000 ) ;
#14941 = AXIS2_PLACEMENT_3D ( 'NONE', #1121, #7798, #16486 ) ;
#14942 = EDGE_LOOP ( 'NONE', ( #15929, #21672, #4, #2292 ) ) ;
#14943 = CARTESIAN_POINT ( 'NONE',  ( 101.8468681455906903, 80.00000000136559208, 4.458734124999987891 ) ) ;
#14944 = CIRCLE ( 'NONE', #20895, 13.57481594606304398 ) ;
#14945 = CARTESIAN_POINT ( 'NONE',  ( 2.493653234604083739E-15, 31.77265625216787370, 13.57481594606304576 ) ) ;
#14946 = EDGE_LOOP ( 'NONE', ( #9620, #8904, #2057, #18467 ) ) ;
#14947 = SHAPE_REPRESENTATION ( 'main air inlet', ( #26844 ), #10431 ) ;
#14948 = CARTESIAN_POINT ( 'NONE',  ( 204.5988444088204403, 37.62656250216787157, -9.598844408820458085 ) ) ;
#14949 = CARTESIAN_POINT ( 'NONE',  ( 51.85481384221820633, 35.19570312608393436, 0.000000000000000000 ) ) ;
#14950 = ORIENTED_EDGE ( 'NONE', *, *, #8563, .F. ) ;
#14951 = CARTESIAN_POINT ( 'NONE',  ( 120.8198241863519939, 55.00000000000000000, -15.00000000000000000 ) ) ;
#14952 = CARTESIAN_POINT ( 'NONE',  ( 96.84719886470459471, 3.152801135295383084, 4.562500001365592084 ) ) ;
#14953 = ORIENTED_EDGE ( 'NONE', *, *, #5353, .F. ) ;
#14954 = CARTESIAN_POINT ( 'NONE',  ( -20.00000000000000355, 55.00000000000000000, -9.999999999999998224 ) ) ;
#14955 = CARTESIAN_POINT ( 'NONE',  ( 13.14518615778179900, 38.02343750108395426, -5.444914386472297529 ) ) ;
#14956 = UNCERTAINTY_MEASURE_WITH_UNIT (LENGTH_MEASURE( 1.000000000000000082E-05 ), #13307, 'distance_accuracy_value', 'NONE');
#14957 = CARTESIAN_POINT ( 'NONE',  ( 195.0000000000000000, 36.53515625216787299, 13.57481594606304576 ) ) ;
#14958 = CARTESIAN_POINT ( 'NONE',  ( 13.14518615778179722, 37.03125000108393294, -5.444914386472297529 ) ) ;
#14959 = FACE_OUTER_BOUND ( 'NONE', #21401, .T. ) ;
#14960 = CARTESIAN_POINT ( 'NONE',  ( 130.0000000000000000, 39.75976562608394005, -13.14518615778179544 ) ) ;
#14961 = CARTESIAN_POINT ( 'NONE',  ( 9.295050272127047819, 37.08085937608393579, 9.295050272127046043 ) ) ;
#14962 = STYLED_ITEM ( 'NONE', ( #27175 ), #19902 ) ;
#14963 = CARTESIAN_POINT ( 'NONE',  ( 135.4449143864723055, 33.65781250108393152, 13.14518615778179189 ) ) ;
#14964 = CARTESIAN_POINT ( 'NONE',  ( 78.57481594606304043, 38.27148437500000711, -5.622872871577873077 ) ) ;
#14965 = CARTESIAN_POINT ( 'NONE',  ( 0.000000000000000000, 40.99999999999999289, 0.000000000000000000 ) ) ;
#14966 = VECTOR ( 'NONE', #6715, 1000.000000000000000 ) ;
#14967 = CARTESIAN_POINT ( 'NONE',  ( 95.54126587499996504, 1.387778780781445676E-14, 2.437500001365592084 ) ) ;
#14968 = FACE_OUTER_BOUND ( 'NONE', #23248, .T. ) ;
#14969 = CARTESIAN_POINT ( 'NONE',  ( 101.8468681455906903, 4.458734125000016313, 2.125000001365591640 ) ) ;
#14970 = CARTESIAN_POINT ( 'NONE',  ( 91.91746824999999887, 110.0000000000000000, -51.12500000273119127 ) ) ;
#14971 = CARTESIAN_POINT ( 'NONE',  ( 5.622872871577796694, 39.26367187716788010, -13.57481594606312036 ) ) ;
#14972 = CARTESIAN_POINT ( 'NONE',  ( 0.000000000000000000, 40.99999999999999289, 0.000000000000000000 ) ) ;
#14973 = CARTESIAN_POINT ( 'NONE',  ( -5.444914386472297529, 33.26093750108393721, -13.14518615778179900 ) ) ;
#14974 = CARTESIAN_POINT ( 'NONE',  ( -5.444914386472299306, 39.31328125108394289, 13.14518615778179722 ) ) ;
#14975 = CARTESIAN_POINT ( 'NONE',  ( 104.9952793366501709, 116.8754121666685393, -50.57499999726882578 ) ) ;
#14976 = EDGE_LOOP ( 'NONE', ( #1, #20746, #23843, #13800 ) ) ;
#14977 = CARTESIAN_POINT ( 'NONE',  ( -5.444914386472299306, 32.16953125108393152, 13.14518615778179722 ) ) ;
#14978 = CARTESIAN_POINT ( 'NONE',  ( 105.6631189606246295, 105.8855032339526758, -53.69999999453763451 ) ) ;
#14979 = CARTESIAN_POINT ( 'NONE',  ( 100.5910519820011473, 122.9999999999999432, 2.314246848314063243 ) ) ;
#14980 = CARTESIAN_POINT ( 'NONE',  ( 185.4011555911795597, 36.33671874999999574, 9.598844408820459861 ) ) ;
#14981 = CARTESIAN_POINT ( 'NONE',  ( 103.5355339059327093, 84.37500000000000000, 3.535533905932726206 ) ) ;
#14982 = EDGE_CURVE ( 'NONE', #23612, #28147, #7110, .T. ) ;
#14983 = CARTESIAN_POINT ( 'NONE',  ( 208.1451861577817795, 40.20625000108393010, -5.444914386472297529 ) ) ;
#14984 = ORIENTED_EDGE ( 'NONE', *, *, #12380, .F. ) ;
#14985 = CARTESIAN_POINT ( 'NONE',  ( 103.5355339059327093, -3.535533905932726206, 7.500000002731185944 ) ) ;
#14986 = CARTESIAN_POINT ( 'NONE',  ( 97.92893218813451028, 82.93750000273118417, -5.000000000000031974 ) ) ;
#14987 = CARTESIAN_POINT ( 'NONE',  ( 139.5988444088204403, 39.90859374999999432, -9.598844408820458085 ) ) ;
#14988 = ORIENTED_EDGE ( 'NONE', *, *, #22584, .F. ) ;
#14989 = CARTESIAN_POINT ( 'NONE',  ( 107.0000000000000142, 107.7255621263696526, -49.10000000000000853 ) ) ;
#14990 = CARTESIAN_POINT ( 'NONE',  ( 5.444914386472297529, 39.51171875108392584, -13.14518615778179900 ) ) ;
#14991 = CARTESIAN_POINT ( 'NONE',  ( 100.8561741729129153, 124.5000000010924737, -2.066987299999999195 ) ) ;
#14992 = CARTESIAN_POINT ( 'NONE',  ( 116.4251840539369454, 35.49335937716787015, -5.622872871577873077 ) ) ;
#14993 = DIRECTION ( 'NONE',  ( 0.000000000000000000, 1.000000000000000000, 0.000000000000000000 ) ) ;
#14994 = FACE_OUTER_BOUND ( 'NONE', #13545, .T. ) ;
#14995 = CARTESIAN_POINT ( 'NONE',  ( 181.8548138422181921, 34.35234375108393579, -5.444914386472297529 ) ) ;
#14996 = ORIENTED_EDGE ( 'NONE', *, *, #3729, .T. ) ;
#14997 = EDGE_LOOP ( 'NONE', ( #17703, #22320, #7940, #22098, #13694, #11199, #8030, #21001, #1642, #27257 ) ) ;
#14998 = CARTESIAN_POINT ( 'NONE',  ( 2.414731522848535132E-15, 39.36289062608393152, 13.14518615778179544 ) ) ;
#14999 = LINE ( 'NONE', #23306, #23024 ) ;
#15000 = CARTESIAN_POINT ( 'NONE',  ( 103.1528011352953342, 81.06250000136559208, -3.152801135295383084 ) ) ;
#15001 = CARTESIAN_POINT ( 'NONE',  ( 185.7049497278729575, 39.66054687608393436, -9.295050272127046043 ) ) ;
#15002 = CONICAL_SURFACE ( 'NONE', #2751, 23.85284712729792389, 0.9599310885968833640 ) ;
#15003 = CARTESIAN_POINT ( 'NONE',  ( -9.295050272127046043, 39.85898437608393152, -9.295050272127046043 ) ) ;
#15004 = CARTESIAN_POINT ( 'NONE',  ( 0.000000000000000000, 23.00000000000000000, 0.000000000000000000 ) ) ;
#15005 = FACE_BOUND ( 'NONE', #8837, .T. ) ;
#15006 = CARTESIAN_POINT ( 'NONE',  ( 0.000000000000000000, 36.00000000000000000, 0.000000000000000000 ) ) ;
#15007 = CARTESIAN_POINT ( 'NONE',  ( 106.5389055433250860, 114.7507929638356785, -48.42499999726882010 ) ) ;
#15008 = VERTEX_POINT ( 'NONE', #21895 ) ;
#15009 = COLOUR_RGB ( '', 0.08235294, 0.09019608, 0.10196078) ;
#15010 = CARTESIAN_POINT ( 'NONE',  ( 13.57481594606304753, 37.47773437500001137, -5.622872871577873077 ) ) ;
#15011 = CARTESIAN_POINT ( 'NONE',  ( 9.295050272127046043, 36.28710937608393294, -9.295050272127046043 ) ) ;
#15012 = CARTESIAN_POINT ( 'NONE',  ( 96.46446609406721961, -3.535533905932727539, 3.250000002731184612 ) ) ;
#15013 = CARTESIAN_POINT ( 'NONE',  ( 116.8548138422182063, 35.24531250108393721, 5.444914386472304635 ) ) ;
#15014 = CARTESIAN_POINT ( 'NONE',  ( 74.29505027212704249, 33.11210937608393579, -9.295050272127046043 ) ) ;
#15015 = CARTESIAN_POINT ( 'NONE',  ( 181.8548138422181921, 37.52734375108393294, -5.444914386472297529 ) ) ;
#15016 = ADVANCED_FACE ( 'NONE', ( #8623 ), #8764, .F. ) ;
#15017 = CARTESIAN_POINT ( 'NONE',  ( 92.99999999999997158, 107.7255621263696810, -46.40000000546236691 ) ) ;
#15018 = CARTESIAN_POINT ( 'NONE',  ( 13.14518615778179544, 36.98164062608393010, -1.609821015232357215E-15 ) ) ;
#15019 =( BOUNDED_SURFACE ( )  B_SPLINE_SURFACE ( 1, 2, ( 
 ( #16480, #10054, #7926, #27604, #27469, #3523, #16623, #25315, #12182, #12327, #7794, #14471, #23189, #25177, #3665, #21048, #5665, #14329, #23001, #14002, #7744, #18445, #7604, #24855, #1068, #3471, #20726, #13857, #20863, #18298, #16293, #16574, #1345, #18582, #27286, #16001, #22725, #16432, #26866, #3191, #20585 ),
 ( #14285, #7312, #1210, #25130, #24715, #5617, #9876, #5335, #12138, #10010, #20444, #24996, #18720, #5193, #5475, #27418, #7881, #9737, #11862, #2906, #5052, #20295, #27152, #13717, #22439, #3332, #11575, #782, #16147, #9452, #14145, #3051, #18152, #22864, #22582, #12002, #11718, #925, #9596, #27006, #7453 ) ),
 .UNSPECIFIED., .F., .F., .T. ) 
 B_SPLINE_SURFACE_WITH_KNOTS ( ( 2, 2 ),
 ( 3, 2, 2, 2, 2, 2, 2, 2, 2, 2, 2, 2, 2, 2, 2, 2, 2, 2, 2, 2, 3 ),
 ( 0.000000000000000000, 1.000000000000000000 ),
 ( 0.000000000000000000, 0.04166666666666666435, 0.08333333333333332871, 0.1250000000000000000, 0.1666666666666666574, 0.2083333333333333426, 0.2500000000000000000, 0.2916666666666666852, 0.3333333333333333148, 0.3750000000000000000, 0.4166666666666666852, 0.4583333333333333148, 0.5000000000000000000, 0.5416666666666666297, 0.5833333333333333703, 0.6250000000000000000, 0.6666666666666666297, 0.7083333333333333703, 0.7500000000000000000, 0.7916666666666666297, 0.8333333333333333703 ),
 .UNSPECIFIED. ) 
 GEOMETRIC_REPRESENTATION_ITEM ( )  RATIONAL_B_SPLINE_SURFACE ( (
 ( 1.000000000000000000, 0.9238795325112867385, 1.000000000000000000, 0.9238795325112867385, 1.000000000000000000, 0.9238795325112867385, 1.000000000000000000, 0.9238795325112867385, 1.000000000000000000, 0.9238795325112867385, 1.000000000000000000, 0.9238795325112867385, 1.000000000000000000, 0.9238795325112867385, 1.000000000000000000, 0.9238795325112867385, 1.000000000000000000, 0.9238795325112867385, 1.000000000000000000, 0.9238795325112867385, 1.000000000000000000, 0.9238795325112867385, 1.000000000000000000, 0.9238795325112867385, 1.000000000000000000, 0.9238795325112867385, 1.000000000000000000, 0.9238795325112867385, 1.000000000000000000, 0.9238795325112867385, 1.000000000000000000, 0.9238795325112867385, 1.000000000000000000, 0.9238795325112867385, 1.000000000000000000, 0.9238795325112867385, 1.000000000000000000, 0.9238795325112867385, 1.000000000000000000, 0.9238795325112867385, 1.000000000000000000),
 ( 1.000000000000000000, 0.9238795325112867385, 1.000000000000000000, 0.9238795325112867385, 1.000000000000000000, 0.9238795325112867385, 1.000000000000000000, 0.9238795325112867385, 1.000000000000000000, 0.9238795325112867385, 1.000000000000000000, 0.9238795325112867385, 1.000000000000000000, 0.9238795325112867385, 1.000000000000000000, 0.9238795325112867385, 1.000000000000000000, 0.9238795325112867385, 1.000000000000000000, 0.9238795325112867385, 1.000000000000000000, 0.9238795325112867385, 1.000000000000000000, 0.9238795325112867385, 1.000000000000000000, 0.9238795325112867385, 1.000000000000000000, 0.9238795325112867385, 1.000000000000000000, 0.9238795325112867385, 1.000000000000000000, 0.9238795325112867385, 1.000000000000000000, 0.9238795325112867385, 1.000000000000000000, 0.9238795325112867385, 1.000000000000000000, 0.9238795325112867385, 1.000000000000000000, 0.9238795325112867385, 1.000000000000000000) ) ) 
 REPRESENTATION_ITEM ( '' )  SURFACE ( )  );
#15020 = CARTESIAN_POINT ( 'NONE',  ( 121.7403884711141018, 50.00000000056351723, -10.79618466886180173 ) ) ;
#15021 = DIRECTION ( 'NONE',  ( 0.000000000000000000, 0.000000000000000000, 1.000000000000000000 ) ) ;
#15022 = CARTESIAN_POINT ( 'NONE',  ( 214.9999999999999716, 75.00000000000000000, -10.00000000000000000 ) ) ;
#15023 = CARTESIAN_POINT ( 'NONE',  ( 13.14518615778179544, 38.56914062608393579, -1.609821015232357215E-15 ) ) ;
#15024 = CARTESIAN_POINT ( 'NONE',  ( 96.46446609406721961, 3.535533905932755072, 10.87500000000000000 ) ) ;
#15025 = DIRECTION ( 'NONE',  ( -0.000000000000000000, -1.000000000000000000, -0.000000000000000000 ) ) ;
#15026 = CARTESIAN_POINT ( 'NONE',  ( 64.16107313071965734, 53.50081894914647762, 14.99999999999997868 ) ) ;
#15027 = CARTESIAN_POINT ( 'NONE',  ( 99.99999999999998579, 90.75000000000000000, 4.999999999999984013 ) ) ;
#15028 = ORIENTED_EDGE ( 'NONE', *, *, #21801, .T. ) ;
#15029 = CARTESIAN_POINT ( 'NONE',  ( 96.84719886470459471, 3.152801135295383084, 10.31250000136559208 ) ) ;
#15030 = CARTESIAN_POINT ( 'NONE',  ( 77.53142549111997539, 36.00000000000000000, -5.200562670743043903 ) ) ;
#15031 = ORIENTED_EDGE ( 'NONE', *, *, #20138, .T. ) ;
#15032 = CARTESIAN_POINT ( 'NONE',  ( 99.99999999999995737, 1.387778780781445676E-14, 0.000000000000000000 ) ) ;
#15033 = CARTESIAN_POINT ( 'NONE',  ( 95.54126587499995082, 1.846868145590750077, 11.37500000136559208 ) ) ;
#15034 = CARTESIAN_POINT ( 'NONE',  ( 55.40115559117954547, 37.82500000216787583, -9.598844408820458085 ) ) ;
#15035 = CARTESIAN_POINT ( 'NONE',  ( -13.14518615778179900, 38.12265625108393152, -5.444914386472297529 ) ) ;
#15036 = CARTESIAN_POINT ( 'NONE',  ( 100.0000000000000000, 110.0000000000000000, -45.00000000000000711 ) ) ;
#15037 = CARTESIAN_POINT ( 'NONE',  ( 95.54126587499996504, 79.68750000136559208, -1.387778780781445676E-14 ) ) ;
#15038 = CARTESIAN_POINT ( 'NONE',  ( 78.14518615778179367, 38.71796875108393721, 5.444914386472293977 ) ) ;
#15039 = CARTESIAN_POINT ( 'NONE',  ( 91.91746824999998466, 112.6261737610028320, -53.22500000273119269 ) ) ;
#15040 = CARTESIAN_POINT ( 'NONE',  ( -8.049105076161786076E-16, 39.56132812608393579, -13.14518615778179544 ) ) ;
#15041 = EDGE_LOOP ( 'NONE', ( #4862, #9091, #8003, #19956 ) ) ;
#15042 = CARTESIAN_POINT ( 'NONE',  ( 99.99999999999998579, 110.0000000000000000, -145.0000000000000284 ) ) ;
#15043 = CARTESIAN_POINT ( 'NONE',  ( -15.00000000000000000, 80.00000000000000000, 10.00000000000000000 ) ) ;
#15044 = CARTESIAN_POINT ( 'NONE',  ( 105.6631189606246295, 105.8855032339526758, -49.69999999453764161 ) ) ;
#15045 = CARTESIAN_POINT ( 'NONE',  ( 120.4011555911795455, 40.10703124999999147, -9.598844408820458085 ) ) ;
#15046 = ORIENTED_EDGE ( 'NONE', *, *, #19587, .F. ) ;
#15047 = CYLINDRICAL_SURFACE ( 'NONE', #21783, 5.000000000000004441 ) ;
#15048 = CARTESIAN_POINT ( 'NONE',  ( 13.14518615778179900, 37.13046875108393863, 5.444914386472293977 ) ) ;
#15049 = CARTESIAN_POINT ( 'NONE',  ( 13.57481594606304576, 36.73359375216787015, -1.662435489736055892E-15 ) ) ;
#15050 = CARTESIAN_POINT ( 'NONE',  ( 130.0000000000000000, 35.59257812608393579, -13.14518615778179544 ) ) ;
#15051 = ADVANCED_FACE ( 'NONE', ( #220 ), #10584, .T. ) ;
#15052 = CARTESIAN_POINT ( 'NONE',  ( 74.59884440882045453, 35.84062500216786873, 9.598844408820456309 ) ) ;
#15053 = CARTESIAN_POINT ( 'NONE',  ( 103.5355339059327093, 83.37500000000000000, 3.535533905932726206 ) ) ;
#15054 = CARTESIAN_POINT ( 'NONE',  ( -5.622872871577873077, 37.27929687716787299, 13.57481594606304753 ) ) ;
#15055 = EDGE_CURVE ( 'NONE', #27806, #6963, #20098, .T. ) ;
#15056 = CARTESIAN_POINT ( 'NONE',  ( 104.9999999999999574, -2.071067811865462627, 5.437499999999999112 ) ) ;
#15057 = DIRECTION ( 'NONE',  ( 0.000000000000000000, 0.000000000000000000, -1.000000000000000000 ) ) ;
#15058 = CARTESIAN_POINT ( 'NONE',  ( 181.8548138422182205, 38.17226562608393436, 0.000000000000000000 ) ) ;
#15059 = FACE_OUTER_BOUND ( 'NONE', #20455, .T. ) ;
#15060 = ADVANCED_FACE ( 'NONE', ( #22741 ), #16162, .T. ) ;
#15061 =( NAMED_UNIT ( * ) PLANE_ANGLE_UNIT ( ) SI_UNIT ( $, .RADIAN. ) );
#15062 = DIRECTION ( 'NONE',  ( 0.000000000000000000, 0.000000000000000000, 1.000000000000000000 ) ) ;
#15063 = DIRECTION ( 'NONE',  ( -0.000000000000000000, -1.000000000000000000, -0.000000000000000000 ) ) ;
#15064 = CARTESIAN_POINT ( 'NONE',  ( 2.493653234604083739E-15, 32.56640625216787299, 13.57481594606304576 ) ) ;
#15065 = CARTESIAN_POINT ( 'NONE',  ( -13.57481594606304753, 37.77539062499999289, -5.622872871577873077 ) ) ;
#15066 = CARTESIAN_POINT ( 'NONE',  ( 9.295050272127047819, 38.66835937608393436, 9.295050272127046043 ) ) ;
#15067 = CARTESIAN_POINT ( 'NONE',  ( 185.4011555911795597, 37.92421874999999432, 9.598844408820459861 ) ) ;
#15068 = CARTESIAN_POINT ( 'NONE',  ( 95.00472066334981491, 103.1245878333314465, -47.07500000273119412 ) ) ;
#15069 = DIRECTION ( 'NONE',  ( 1.000000000000000000, 0.000000000000000000, -5.782411586589357392E-17 ) ) ;
#15070 = CARTESIAN_POINT ( 'NONE',  ( 74.29505027212704249, 37.87460937608393152, -9.295050272127046043 ) ) ;
#15071 =( BOUNDED_CURVE ( )  B_SPLINE_CURVE ( 2, ( #16179, #22758, #1099, #7342, #11605 ),
 .UNSPECIFIED., .F., .T. ) 
 B_SPLINE_CURVE_WITH_KNOTS ( ( 3, 2, 3 ),
 ( 0.000000000000000000, 0.01041666666666679446, 0.02083333333333358892 ),
 .UNSPECIFIED. ) 
 CURVE ( )  GEOMETRIC_REPRESENTATION_ITEM ( )  RATIONAL_B_SPLINE_CURVE ( ( 1.000000000000000000, 0.9238795325112867385, 1.000000000000000000, 0.9238795325112848511, 1.000000000000001776 ) ) 
 REPRESENTATION_ITEM ( '' )  );
#15072 = CARTESIAN_POINT ( 'NONE',  ( 101.8468681455907046, -4.458734124999987891, 0.7500000013655925279 ) ) ;
#15073 = DIRECTION ( 'NONE',  ( -1.000000000000000000, 0.000000000000000000, 0.000000000000000000 ) ) ;
#15074 = CARTESIAN_POINT ( 'NONE',  ( 99.99999999999998579, 94.06249999863440792, 4.458734124999981674 ) ) ;
#15075 = CARTESIAN_POINT ( 'NONE',  ( 95.00000000000000000, 93.43749999726880162, 2.071067811865463959 ) ) ;
#15076 = CARTESIAN_POINT ( 'NONE',  ( -13.57481594606304753, 36.18789062499999432, -5.622872871577873077 ) ) ;
#15077 = CARTESIAN_POINT ( 'NONE',  ( 95.67376207875072680, 104.0454443415356991, -45.70000000000000284 ) ) ;
#15078 = VERTEX_POINT ( 'NONE', #797 ) ;
#15079 = CARTESIAN_POINT ( 'NONE',  ( 94.99999999999995737, 84.00000000000000000, -1.387778780781445676E-14 ) ) ;
#15080 = CARTESIAN_POINT ( 'NONE',  ( 103.1528011352953484, 95.18749999863440792, 3.152801135295352886 ) ) ;
#15081 = EDGE_LOOP ( 'NONE', ( #14205, #17585, #23555, #5056 ) ) ;
#15082 = CARTESIAN_POINT ( 'NONE',  ( 102.1631189606246153, 116.6573956140660897, -47.60000000000000853 ) ) ;
#15083 = CARTESIAN_POINT ( 'NONE',  ( 51.85481384221820633, 36.03906250108394005, 5.444914386472304635 ) ) ;
#15084 = EDGE_LOOP ( 'NONE', ( #27858, #14261, #27557, #6225 ) ) ;
#15085 = CARTESIAN_POINT ( 'NONE',  ( -13.57481594606304576, 33.16171875216787868, 0.000000000000000000 ) ) ;
#15086 = ADVANCED_FACE ( 'NONE', ( #17885 ), #13731, .F. ) ;
#15087 = CARTESIAN_POINT ( 'NONE',  ( 95.54126587499995082, -1.846868145590724986, 3.750000001365591640 ) ) ;
#15088 = VERTEX_POINT ( 'NONE', #13590 ) ;
#15089 = CARTESIAN_POINT ( 'NONE',  ( -9.295050272127044266, 34.50117187608393721, 9.295050272127047819 ) ) ;
#15090 = CARTESIAN_POINT ( 'NONE',  ( -5.444914386472297529, 40.60312500108393863, -13.14518615778179900 ) ) ;
#15091 = CARTESIAN_POINT ( 'NONE',  ( 185.4011555911795597, 36.43593750216787441, 9.598844408820459861 ) ) ;
#15092 = CARTESIAN_POINT ( 'NONE',  ( -8.049105076161786076E-16, 35.59257812608393579, -13.14518615778179544 ) ) ;
#15093 = CYLINDRICAL_SURFACE ( 'NONE', #13011, 13.57481594606304398 ) ;
#15094 = CARTESIAN_POINT ( 'NONE',  ( 193.8612318828944581, 50.00000000043882409, 13.56816686242560266 ) ) ;
#15095 = CARTESIAN_POINT ( 'NONE',  ( 116.8548138422182205, 36.78320312608393294, 0.000000000000000000 ) ) ;
#15096 = CARTESIAN_POINT ( 'NONE',  ( -5.444914386472299306, 36.93203125108394147, 13.14518615778179722 ) ) ;
#15097 = CARTESIAN_POINT ( 'NONE',  ( 143.1451861577818079, 33.85625000108393579, -5.444914386472297529 ) ) ;
#15098 = CARTESIAN_POINT ( 'NONE',  ( 59.37712712842213136, 33.21132812499999432, 13.57481594606304753 ) ) ;
#15099 = CARTESIAN_POINT ( 'NONE',  ( -13.14518615778179544, 40.75195312608393294, 0.000000000000000000 ) ) ;
#15100 = CARTESIAN_POINT ( 'NONE',  ( 95.54126587499995082, -1.846868145590724986, 2.500000001365592084 ) ) ;
#15101 = CARTESIAN_POINT ( 'NONE',  ( 197.2323271553383108, 36.00000000000000711, 12.98409812936874630 ) ) ;
#15102 = CARTESIAN_POINT ( 'NONE',  ( 103.1528011352953342, 3.152801135295383084, 4.062500001365592084 ) ) ;
#15103 = CARTESIAN_POINT ( 'NONE',  ( 0.000000000000000000, 40.99999999999999289, -13.57481594606304576 ) ) ;
#15104 = DIRECTION ( 'NONE',  ( 0.000000000000000000, 0.000000000000000000, 1.000000000000000000 ) ) ;
#15105 =( BOUNDED_CURVE ( )  B_SPLINE_CURVE ( 2, ( #20602, #7763, #20743, #5636, #9753, #20462, #943, #3491, #18867 ),
 .UNSPECIFIED., .F., .F. ) 
 B_SPLINE_CURVE_WITH_KNOTS ( ( 3, 2, 2, 2, 3 ),
 ( 0.5357142857142856984, 0.5446428571428570953, 0.5535714285714286031, 0.5625000000000000000, 0.5714285714285713969 ),
 .UNSPECIFIED. ) 
 CURVE ( )  GEOMETRIC_REPRESENTATION_ITEM ( )  RATIONAL_B_SPLINE_CURVE ( ( 1.000000000000000000, 0.9238795325112867385, 1.000000000000000000, 0.9238795325112867385, 1.000000000000000000, 0.9238795325112867385, 1.000000000000000000, 0.9238795325112867385, 1.000000000000000000 ) ) 
 REPRESENTATION_ITEM ( '' )  );
#15106 = CARTESIAN_POINT ( 'NONE',  ( 101.8468681455907046, 80.37500000136563472, -4.458734125000016313 ) ) ;
#15107 = CARTESIAN_POINT ( 'NONE',  ( -9.295050272127044266, 33.50898437608393010, 9.295050272127047819 ) ) ;
#15108 = CARTESIAN_POINT ( 'NONE',  ( 9.295050272127046043, 38.86679687608393863, -9.295050272127046043 ) ) ;
#15109 = CIRCLE ( 'NONE', #11951, 15.57481594606304576 ) ;
#15110 = CARTESIAN_POINT ( 'NONE',  ( 108.0825317499999869, 107.3738262389971538, -46.97499999726881015 ) ) ;
#15111 = VERTEX_POINT ( 'NONE', #6904 ) ;
#15112 = CARTESIAN_POINT ( 'NONE',  ( 99.99999999999998579, 90.00000000000000000, -6.938893903907228378E-15 ) ) ;
#15113 = CARTESIAN_POINT ( 'NONE',  ( 124.3771271284220319, 37.27929687716785878, 13.57481594606295161 ) ) ;
#15114 = CARTESIAN_POINT ( 'NONE',  ( 99.29898749929290602, 122.9999999999999858, 2.154550021601044030 ) ) ;
#15115 = FACE_OUTER_BOUND ( 'NONE', #11223, .T. ) ;
#15116 = CARTESIAN_POINT ( 'NONE',  ( 204.2950502721270425, 37.67617187608393436, 9.295050272127046043 ) ) ;
#15117 = ORIENTED_EDGE ( 'NONE', *, *, #984, .T. ) ;
#15118 = DIRECTION ( 'NONE',  ( 0.000000000000000000, 0.000000000000000000, -1.000000000000000000 ) ) ;
#15119 = FACE_OUTER_BOUND ( 'NONE', #24993, .T. ) ;
#15120 = CARTESIAN_POINT ( 'NONE',  ( 101.8468681455906903, 4.458734125000016313, 14.37500000136559386 ) ) ;
#15121 = VERTEX_POINT ( 'NONE', #15593 ) ;
#15122 = CARTESIAN_POINT ( 'NONE',  ( 94.33688103937537051, 105.8855032339526758, -53.80000000000000426 ) ) ;
#15123 = CARTESIAN_POINT ( 'NONE',  ( -5.444914386472299306, 38.32109375108394289, 13.14518615778179722 ) ) ;
#15124 = CARTESIAN_POINT ( 'NONE',  ( 98.53841926354351699, 123.0500000010924850, -1.461580736456474794 ) ) ;
#15125 = VECTOR ( 'NONE', #10911, 1000.000000000000000 ) ;
#15126 = CARTESIAN_POINT ( 'NONE',  ( 139.5988444088204687, 32.66562500216787157, 9.598844408820456309 ) ) ;
#15127 = CARTESIAN_POINT ( 'NONE',  ( 0.000000000000000000, 1.500000000000001332, 0.000000000000000000 ) ) ;
#15128 = DIRECTION ( 'NONE',  ( 0.000000000000000000, 0.000000000000000000, 1.000000000000000000 ) ) ;
#15129 = DIRECTION ( 'NONE',  ( 0.000000000000000000, 0.000000000000000000, -1.000000000000000000 ) ) ;
#15130 = CARTESIAN_POINT ( 'NONE',  ( 208.1451861577818079, 34.00507812608393721, -1.609821015232357215E-15 ) ) ;
#15131 = VERTEX_POINT ( 'NONE', #365 ) ;
#15132 = EDGE_CURVE ( 'NONE', #8293, #2910, #22454, .T. ) ;
#15133 = ORIENTED_EDGE ( 'NONE', *, *, #7065, .T. ) ;
#15134 = ORIENTED_EDGE ( 'NONE', *, *, #10867, .T. ) ;
#15135 = CARTESIAN_POINT ( 'NONE',  ( -8.049105076161786076E-16, 38.17226562608394147, -13.14518615778179544 ) ) ;
#15136 =( NAMED_UNIT ( * ) SI_UNIT ( $, .STERADIAN. ) SOLID_ANGLE_UNIT ( ) );
#15137 = EDGE_CURVE ( 'NONE', #12494, #17873, #24299, .T. ) ;
#15138 = CARTESIAN_POINT ( 'NONE',  ( 95.54126587499996504, -1.846868145590724986, 12.75000000136559208 ) ) ;
#15139 = CARTESIAN_POINT ( 'NONE',  ( 65.00000000000000000, 39.16445312608392726, 13.14518615778179544 ) ) ;
#15140 = CARTESIAN_POINT ( 'NONE',  ( 104.4587341249999781, 81.87500000136560629, 1.846868145590721655 ) ) ;
#15141 = CARTESIAN_POINT ( 'NONE',  ( 204.2950502721270425, 38.46992187608393010, 9.295050272127046043 ) ) ;
#15142 = CARTESIAN_POINT ( 'NONE',  ( 5.444914386472297529, 37.32890625108393579, -13.14518615778179722 ) ) ;
#15143 = CYLINDRICAL_SURFACE ( 'NONE', #3668, 23.00000000000001421 ) ;
#15144 = DIRECTION ( 'NONE',  ( 0.000000000000000000, 0.000000000000000000, -1.000000000000000000 ) ) ;
#15145 = CARTESIAN_POINT ( 'NONE',  ( 70.62287287157778337, 39.95820312499999716, -13.57481594606312036 ) ) ;
#15146 = CARTESIAN_POINT ( 'NONE',  ( 99.99999999999997158, 118.4984768113314004, -54.12499999726881583 ) ) ;
#15147 = ORIENTED_EDGE ( 'NONE', *, *, #19113, .F. ) ;
#15148 =( BOUNDED_CURVE ( )  B_SPLINE_CURVE ( 2, ( #731, #11673, #14240, #18394, #22961, #880, #7405, #16098, #27100, #7697, #3423, #16248, #24945, #5431, #22820, #16389, #1294, #12090, #23644, #25771, #6251, #4119, #23231, #8243, #18807, #27784, #5980, #5712, #12645, #16932, #25366, #14923, #12784, #18940, #10513, #21501, #14378, #1437, #18676, #12370, #3568, #21371, #12499, #8109, #27922, #16669, #16530, #25501, #23366, #27649, #1981, #25632, #3708, #17068, #6115, #8383, #23502, #1576, #27377, #23094, #21088, #12226, #14781, #20954, #7969, #10094, #1850, #3982, #16803, #14647, #5845, #7837, #27512, #14515, #10230, #19220, #25223, #3838, #1711, #21227, #10372, #19079, #25917, #24201, #13488, #8804, #8665, #4681, #6391, #28197, #4397, #19499, #26488 ),
 .UNSPECIFIED., .F., .F. ) 
 B_SPLINE_CURVE_WITH_KNOTS ( ( 3, 2, 2, 2, 2, 2, 2, 2, 2, 2, 2, 2, 2, 2, 2, 2, 2, 2, 2, 2, 2, 2, 2, 2, 2, 2, 2, 2, 2, 2, 2, 2, 2, 2, 2, 2, 2, 2, 2, 2, 2, 2, 2, 2, 2, 2, 3 ),
 ( 0.000000000000000000, 0.01041666666666666609, 0.02083333333333333218, 0.03125000000000000000, 0.04166666666666666435, 0.05208333333333333565, 0.06250000000000000000, 0.07291666666666667129, 0.08333333333333332871, 0.09375000000000000000, 0.1041666666666666713, 0.1145833333333333287, 0.1250000000000000000, 0.1354166666666666574, 0.1458333333333333426, 0.1562500000000000278, 0.1666666666666666574, 0.1770833333333333426, 0.1875000000000000000, 0.1979166666666666574, 0.2083333333333333426, 0.2187499999999999722, 0.2291666666666666574, 0.2395833333333333426, 0.2500000000000000000, 0.2604166666666666852, 0.2708333333333333148, 0.2812500000000000000, 0.2916666666666666852, 0.3020833333333333148, 0.3125000000000000555, 0.3229166666666666852, 0.3333333333333333148, 0.3437500000000000000, 0.3541666666666666852, 0.3645833333333333148, 0.3750000000000000000, 0.3854166666666666852, 0.3958333333333333148, 0.4062500000000000000, 0.4166666666666666852, 0.4270833333333333148, 0.4374999999999999445, 0.4479166666666666852, 0.4583333333333333148, 0.4687500000000000000, 0.4779971559588573893 ),
 .UNSPECIFIED. ) 
 CURVE ( )  GEOMETRIC_REPRESENTATION_ITEM ( )  RATIONAL_B_SPLINE_CURVE ( ( 1.000000000000000000, 0.9238795325112867385, 1.000000000000000000, 0.9238795325112867385, 1.000000000000000000, 0.9238795325112867385, 1.000000000000000000, 0.9238795325112867385, 1.000000000000000000, 0.9238795325112867385, 1.000000000000000000, 0.9238795325112867385, 1.000000000000000000, 0.9238795325112867385, 1.000000000000000000, 0.9238795325112867385, 1.000000000000000000, 0.9238795325112867385, 1.000000000000000000, 0.9238795325112867385, 1.000000000000000000, 0.9238795325112867385, 1.000000000000000000, 0.9238795325112867385, 1.000000000000000000, 0.9238795325112867385, 1.000000000000000000, 0.9238795325112867385, 1.000000000000000000, 0.9238795325112867385, 1.000000000000000000, 0.9238795325112867385, 1.000000000000000000, 0.9238795325112867385, 1.000000000000000000, 0.9238795325112867385, 1.000000000000000000, 0.9238795325112867385, 1.000000000000000000, 0.9238795325112867385, 1.000000000000000000, 0.9238795325112867385, 1.000000000000000000, 0.9238795325112867385, 1.000000000000000000, 0.9238795325112867385, 1.000000000000000000, 0.9238795325112867385, 1.000000000000000000, 0.9238795325112867385, 1.000000000000000000, 0.9238795325112867385, 1.000000000000000000, 0.9238795325112867385, 1.000000000000000000, 0.9238795325112867385, 1.000000000000000000, 0.9238795325112867385, 1.000000000000000000, 0.9238795325112867385, 1.000000000000000000, 0.9238795325112867385, 1.000000000000000000, 0.9238795325112867385, 1.000000000000000000, 0.9238795325112867385, 1.000000000000000000, 0.9238795325112867385, 1.000000000000000000, 0.9238795325112867385, 1.000000000000000000, 0.9238795325112867385, 1.000000000000000000, 0.9238795325112867385, 1.000000000000000000, 0.9238795325112867385, 1.000000000000000000, 0.9238795325112867385, 1.000000000000000000, 0.9238795325112867385, 1.000000000000000000, 0.9238795325112867385, 1.000000000000000000, 0.9238795325112867385, 1.000000000000000000, 0.9238795325112867385, 1.000000000000000000, 0.9238795325112867385, 1.000000000000000000, 0.9238795325112867385, 1.000000000000000000, 0.9324258078851906939, 0.9848264816800322841 ) ) 
 REPRESENTATION_ITEM ( '' )  );
#15149 = CARTESIAN_POINT ( 'NONE',  ( 2.493653234604083739E-15, 37.22968749999999716, 13.57481594606304576 ) ) ;
#15150 = CARTESIAN_POINT ( 'NONE',  ( 2.414731522848535132E-15, 38.37070312608393152, 13.14518615778179544 ) ) ;
#15151 = CARTESIAN_POINT ( 'NONE',  ( 103.5355339059327093, -3.535533905932726206, 3.500000002731184612 ) ) ;
#15152 = CARTESIAN_POINT ( 'NONE',  ( 139.2950502721270425, 34.89804687608393863, -9.295050272127046043 ) ) ;
#15153 = CARTESIAN_POINT ( 'NONE',  ( 70.44491438647230552, 34.74921875108394431, -13.14518615778179900 ) ) ;
#15154 = CARTESIAN_POINT ( 'NONE',  ( 204.2950502721270425, 37.08085937608393579, 9.295050272127046043 ) ) ;
#15155 = CARTESIAN_POINT ( 'NONE',  ( 103.5355338419364699, 95.00000000000001421, -3.535533969929001596 ) ) ;
#15156 = CARTESIAN_POINT ( 'NONE',  ( 6.944423797152705191, 31.55306878032414986, -11.16113333171310451 ) ) ;
#15157 = CARTESIAN_POINT ( 'NONE',  ( 181.8473230904129139, 36.00000000000000711, 0.5874252385153372336 ) ) ;
#15158 = CARTESIAN_POINT ( 'NONE',  ( 94.99999999999995737, 1.387778780781445676E-14, 10.12500000273118594 ) ) ;
#15159 = CARTESIAN_POINT ( 'NONE',  ( 9.295050272127047819, 32.31835937608393294, 9.295050272127046043 ) ) ;
#15160 = CARTESIAN_POINT ( 'NONE',  ( 99.99999999999998579, 101.5015231886685712, -52.62500000273118417 ) ) ;
#15161 = CARTESIAN_POINT ( 'NONE',  ( -8.049105076161786076E-16, 36.38632812608393152, -13.14518615778179544 ) ) ;
#15162 = CARTESIAN_POINT ( 'NONE',  ( 98.23223304703363112, 124.1000000000000085, -1.767766952966370209 ) ) ;
#15163 = CARTESIAN_POINT ( 'NONE',  ( 102.4999999999999858, 122.3000000021849587, -9.847140817659276890E-15 ) ) ;
#15164 = CARTESIAN_POINT ( 'NONE',  ( 59.63450343195739833, 54.48174559707608466, 14.99999999999998046 ) ) ;
#15165 = B_SPLINE_CURVE_WITH_KNOTS ( 'NONE', 3,
 ( #18854, #27562, #8023, #16722, #5901, #1625, #25556, #27702, #6035, #8165, #23420, #14701, #3893, #4175, #12837, #6576, #17701, #8720 ),
 .UNSPECIFIED., .F., .F.,
 ( 4, 2, 2, 2, 2, 2, 2, 2, 4 ),
 ( 0.000000000000000000, 0.0005599264814053035114, 0.001119852962810607023, 0.001679779444215910534, 0.002239705925621214046, 0.002799632407026517340, 0.003359558888431821069, 0.003919485369837124797, 0.004479411851242428091 ),
 .UNSPECIFIED. ) ;
#15166 = EDGE_CURVE ( 'NONE', #22369, #2045, #13872, .T. ) ;
#15167 = DIRECTION ( 'NONE',  ( -0.000000000000000000, 1.000000000000000000, -0.000000000000000000 ) ) ;
#15168 = CARTESIAN_POINT ( 'NONE',  ( 98.15313185440925281, 4.458734125000016313, 8.250000001365592084 ) ) ;
#15169 = VERTEX_POINT ( 'NONE', #22599 ) ;
#15170 = CARTESIAN_POINT ( 'NONE',  ( 102.4999999999999858, 122.3000000021849587, -9.847140817659276890E-15 ) ) ;
#15171 = CARTESIAN_POINT ( 'NONE',  ( 99.99999999999995737, 4.458734125000016313, 11.18750000136559208 ) ) ;
#15172 = CARTESIAN_POINT ( 'NONE',  ( 123.5491206573346830, 50.00000000106874154, 11.97362904075384016 ) ) ;
#15173 = CARTESIAN_POINT ( 'NONE',  ( 13.14518615778179900, 38.61875000108393152, -5.444914386472297529 ) ) ;
#15174 = DIRECTION ( 'NONE',  ( -5.782411586589357392E-17, 0.000000000000000000, -1.000000000000000000 ) ) ;
#15175 = CARTESIAN_POINT ( 'NONE',  ( 98.15313185440925281, 81.87500000136559208, 4.458734124999987891 ) ) ;
#15176 = CARTESIAN_POINT ( 'NONE',  ( 74.29505027212704249, 36.28710937608393294, 9.295050272127046043 ) ) ;
#15177 = CARTESIAN_POINT ( 'NONE',  ( 93.46109445667491400, 114.7507929638356785, -49.32500000273120122 ) ) ;
#15178 = CARTESIAN_POINT ( 'NONE',  ( 97.92893218813451028, 5.000000000000018652, 11.81250000000000000 ) ) ;
#15179 = ORIENTED_EDGE ( 'NONE', *, *, #20148, .F. ) ;
#15180 = FACE_OUTER_BOUND ( 'NONE', #14976, .T. ) ;
#15181 = DIRECTION ( 'NONE',  ( 0.000000000000000000, 1.000000000000000000, 0.000000000000000000 ) ) ;
#15182 = CARTESIAN_POINT ( 'NONE',  ( 104.9999999999999716, 82.50000000000000000, -1.449011120738813565E-14 ) ) ;
#15183 = CARTESIAN_POINT ( 'NONE',  ( 143.5748159460630404, 37.37851562499999858, 5.622872871577869525 ) ) ;
#15184 = VERTEX_POINT ( 'NONE', #18169 ) ;
#15185 = DIRECTION ( 'NONE',  ( 0.000000000000000000, 1.000000000000000000, 0.000000000000000000 ) ) ;
#15186 = CARTESIAN_POINT ( 'NONE',  ( 5.444914386472302859, 35.44375000108393436, 13.14518615778179189 ) ) ;
#15187 = CARTESIAN_POINT ( 'NONE',  ( -5.622872871577873077, 36.98164062716787015, -13.57481594606304753 ) ) ;
#15188 =( BOUNDED_CURVE ( )  B_SPLINE_CURVE ( 2, ( #1315, #27668, #14537, #21248, #10111 ),
 .UNSPECIFIED., .F., .T. ) 
 B_SPLINE_CURVE_WITH_KNOTS ( ( 3, 2, 3 ),
 ( 0.000000000000000000, 0.04166666666666653945, 0.08333333333333307891 ),
 .UNSPECIFIED. ) 
 CURVE ( )  GEOMETRIC_REPRESENTATION_ITEM ( )  RATIONAL_B_SPLINE_CURVE ( ( 1.000000000000000000, 0.9238795325112867385, 1.000000000000000000, 0.9238795325112871826, 0.9999999999999995559 ) ) 
 REPRESENTATION_ITEM ( '' )  );
#15189 = CARTESIAN_POINT ( 'NONE',  ( 143.1451861577818079, 36.23750000108393010, -5.444914386472297529 ) ) ;
#15190 = CARTESIAN_POINT ( 'NONE',  ( 78.57481594606305464, 34.35234375216787583, -1.662435489736055892E-15 ) ) ;
#15191 = CARTESIAN_POINT ( 'NONE',  ( 112.9999999999999858, 0.000000000000000000, -8.673617379884035472E-16 ) ) ;
#15192 = CARTESIAN_POINT ( 'NONE',  ( -5.622872871577873077, 33.80664062716786589, -13.57481594606304753 ) ) ;
#15193 = CARTESIAN_POINT ( 'NONE',  ( 102.0710678118654329, 5.000000000000018652, 5.687500000000000000 ) ) ;
#15194 = CARTESIAN_POINT ( 'NONE',  ( 108.0825317499999869, 107.3738262389971680, -48.97499999726881725 ) ) ;
#15195 = EDGE_CURVE ( 'NONE', #23831, #13180, #25010, .T. ) ;
#15196 = VECTOR ( 'NONE', #5592, 1000.000000000000227 ) ;
#15197 = CARTESIAN_POINT ( 'NONE',  ( 195.0000000000000000, 37.18007812608393436, -13.14518615778179544 ) ) ;
#15198 = CARTESIAN_POINT ( 'NONE',  ( 120.8198241863519939, 55.00000000000000000, 9.999999999999969802 ) ) ;
#15199 = CARTESIAN_POINT ( 'NONE',  ( 13.57481594606304931, 34.30273437716787299, 5.622872871577868636 ) ) ;
#15200 = CARTESIAN_POINT ( 'NONE',  ( 181.4251840539369596, 37.87460937716787868, -5.622872871577872189 ) ) ;
#15201 = DIRECTION ( 'NONE',  ( 0.000000000000000000, 0.000000000000000000, -1.000000000000000000 ) ) ;
#15202 = CARTESIAN_POINT ( 'NONE',  ( 204.5988444088204403, 36.73359374999999716, -9.598844408820458085 ) ) ;
#15203 = CARTESIAN_POINT ( 'NONE',  ( 5.622872871577871301, 38.37070312499999147, -13.57481594606304753 ) ) ;
#15204 = CARTESIAN_POINT ( 'NONE',  ( 84.99999999999998579, 120.0000000000000000, -15.00000000000000533 ) ) ;
#15205 = CARTESIAN_POINT ( 'NONE',  ( -8.049105076161786076E-16, 38.17226562608394147, -13.14518615778179544 ) ) ;
#15206 = CARTESIAN_POINT ( 'NONE',  ( -5.444914386472299306, 39.90859375108393436, 13.14518615778179722 ) ) ;
#15207 = EDGE_CURVE ( 'NONE', #6975, #15231, #23179, .T. ) ;
#15208 = CARTESIAN_POINT ( 'NONE',  ( 200.6228728715778686, 35.69179687499999432, 13.57481594606304576 ) ) ;
#15209 = CARTESIAN_POINT ( 'NONE',  ( 65.00000000000000000, 40.00781250000000000, -13.57481594606304576 ) ) ;
#15210 = CARTESIAN_POINT ( 'NONE',  ( 70.44491438647230552, 36.03906250108394005, 13.14518615778179189 ) ) ;
#15211 = ADVANCED_FACE ( 'NONE', ( #11733 ), #20457, .F. ) ;
#15212 = CARTESIAN_POINT ( 'NONE',  ( 99.99999999999995737, 85.00000000000000000, -1.387778780781445676E-14 ) ) ;
#15213 = CARTESIAN_POINT ( 'NONE',  ( -9.598844408820454532, 35.64218750216787868, 9.598844408820459861 ) ) ;
#15214 = CARTESIAN_POINT ( 'NONE',  ( 104.4587341249999781, 93.31249999863440792, -6.938893903907228378E-15 ) ) ;
#15215 = DIRECTION ( 'NONE',  ( 0.000000000000000000, -1.000000000000000000, 0.000000000000000000 ) ) ;
#15216 = CARTESIAN_POINT ( 'NONE',  ( 5.622872871577878406, 35.69179687499999432, 13.57481594606304576 ) ) ;
#15217 = CARTESIAN_POINT ( 'NONE',  ( 130.0000000000000000, 40.55351562608393579, -13.14518615778179544 ) ) ;
#15218 = EDGE_CURVE ( 'NONE', #11953, #4933, #13196, .T. ) ;
#15219 = VERTEX_POINT ( 'NONE', #14299 ) ;
#15220 = CARTESIAN_POINT ( 'NONE',  ( 99.99999999999995737, 80.93750000136559208, 4.458734124999988779 ) ) ;
#15221 = CIRCLE ( 'NONE', #3876, 5.000000000000000000 ) ;
#15222 = CARTESIAN_POINT ( 'NONE',  ( 96.84719886470463734, 94.93749999863440792, 3.152801135295351997 ) ) ;
#15223 = CARTESIAN_POINT ( 'NONE',  ( 64.82771023522410303, 35.99999999999999289, -13.51468191220837944 ) ) ;
#15224 = VERTEX_POINT ( 'NONE', #14578 ) ;
#15225 = EDGE_CURVE ( 'NONE', #10588, #18001, #21173, .T. ) ;
#15226 = CARTESIAN_POINT ( 'NONE',  ( 104.3262379212492448, 115.9545556584642867, -49.70000000000001705 ) ) ;
#15227 = CARTESIAN_POINT ( 'NONE',  ( 78.14518615778179367, 36.43593750108392726, -5.444914386472297529 ) ) ;
#15228 = ORIENTED_EDGE ( 'NONE', *, *, #3794, .T. ) ;
#15229 = CARTESIAN_POINT ( 'NONE',  ( 143.5748159460630688, 39.16445312716788152, -5.622872871577873966 ) ) ;
#15230 = CARTESIAN_POINT ( 'NONE',  ( 104.4587341249999781, -1.846868145590721655, 2.125000001365591640 ) ) ;
#15231 = VERTEX_POINT ( 'NONE', #3347 ) ;
#15232 = CARTESIAN_POINT ( 'NONE',  ( 99.99999999999995737, 81.87500000273119838, -5.000000000000018652 ) ) ;
#15233 = CARTESIAN_POINT ( 'NONE',  ( 9.295050272127046043, 38.86679687608393863, -9.295050272127046043 ) ) ;
#15234 = CARTESIAN_POINT ( 'NONE',  ( 195.0000000000000000, 36.93203125216787441, -13.57481594606304576 ) ) ;
#15235 = CARTESIAN_POINT ( 'NONE',  ( -9.295050272127044266, 35.09648437608392868, 9.295050272127047819 ) ) ;
#15236 = CARTESIAN_POINT ( 'NONE',  ( -20.00000000000000000, 75.00000000000000000, 15.00000000000000178 ) ) ;
#15237 = EDGE_CURVE ( 'NONE', #27263, #58, #13490, .T. ) ;
#15238 = CARTESIAN_POINT ( 'NONE',  ( 102.4999999999999858, 122.3000000021849587, -9.847140817659276890E-15 ) ) ;
#15239 = CARTESIAN_POINT ( 'NONE',  ( 13.14518615778179900, 37.92421875108392726, 5.444914386472293977 ) ) ;
#15240 = CARTESIAN_POINT ( 'NONE',  ( 116.8548138422182063, 34.94765625108392726, -5.444914386472297529 ) ) ;
#15241 = CARTESIAN_POINT ( 'NONE',  ( 78.57481594606304043, 34.99726562500000426, 5.622872871577869525 ) ) ;
#15242 = CARTESIAN_POINT ( 'NONE',  ( 104.9999999999999716, 1.449011120738813565E-14, 9.500000000000000000 ) ) ;
#15243 = CARTESIAN_POINT ( 'NONE',  ( 98.15313185440925281, -4.458734124999987891, 9.875000001365593860 ) ) ;
#15244 = CARTESIAN_POINT ( 'NONE',  ( 107.0000000000000142, 110.0000000000000000, -47.00000000000000711 ) ) ;
#15246 = ADVANCED_FACE ( 'NONE', ( #5634 ), #20878, .F. ) ;
#15245 = CARTESIAN_POINT ( 'NONE',  ( 103.1528011352953342, -3.152801135295355106, 13.81250000136559208 ) ) ;
#15247 = CARTESIAN_POINT ( 'NONE',  ( 93.46109445667491400, 114.7507929638356785, -53.32500000273119412 ) ) ;
#15248 = CARTESIAN_POINT ( 'NONE',  ( 84.99999999999998579, 125.0000000000000000, 14.99999999999999112 ) ) ;
#15249 = VECTOR ( 'NONE', #2304, 1000.000000000000000 ) ;
#15250 = AXIS2_PLACEMENT_3D ( 'NONE', #4585, #13245, #21977 ) ;
#15251 = CARTESIAN_POINT ( 'NONE',  ( 96.84719886470459471, 80.81250000136559208, 3.152801135295355994 ) ) ;
#15252 = CARTESIAN_POINT ( 'NONE',  ( 97.50236033167490746, 117.6869444889999841, -48.02499999726882152 ) ) ;
#15253 = CARTESIAN_POINT ( 'NONE',  ( 9.295050272127047819, 37.08085937608393579, 9.295050272127046043 ) ) ;
#15254 = EDGE_CURVE ( 'NONE', #26290, #9425, #16424, .T. ) ;
#15255 = CARTESIAN_POINT ( 'NONE',  ( 91.91746824999998466, 110.0000000000000000, -49.87499999726882294 ) ) ;
#15256 = ORIENTED_EDGE ( 'NONE', *, *, #2215, .T. ) ;
#15257 = CARTESIAN_POINT ( 'NONE',  ( 99.14382582708708469, 123.3000000010924708, 2.066987299999979655 ) ) ;
#15258 = CARTESIAN_POINT ( 'NONE',  ( 93.00000000000000000, 110.0000000000000000, -54.00000000000000711 ) ) ;
#15259 = CARTESIAN_POINT ( 'NONE',  ( 94.99999999999995737, 1.387778780781445676E-14, 3.125000002731185944 ) ) ;
#15260 = CARTESIAN_POINT ( 'NONE',  ( 195.0000000000000000, 38.37070312608393152, 13.14518615778179544 ) ) ;
#15261 = ORIENTED_EDGE ( 'NONE', *, *, #11058, .F. ) ;
#15262 = CARTESIAN_POINT ( 'NONE',  ( 65.00000000000000000, 36.58476562608393579, -13.14518615778179544 ) ) ;
#15263 = CARTESIAN_POINT ( 'NONE',  ( 91.91746824999998466, 110.0000000000000000, -45.74999999726882294 ) ) ;
#15264 = CARTESIAN_POINT ( 'NONE',  ( 66.60527187657659454, 53.60388944777320575, -14.99999999999999822 ) ) ;
#15265 = ORIENTED_EDGE ( 'NONE', *, *, #8133, .T. ) ;
#15266 = CARTESIAN_POINT ( 'NONE',  ( 102.1631189606246295, 116.6573956140660897, -48.60000000000000142 ) ) ;
#15267 = CARTESIAN_POINT ( 'NONE',  ( -13.14518615778179900, 39.71015625108393010, -5.444914386472297529 ) ) ;
#15268 = CIRCLE ( 'NONE', #1648, 5.000000000000004441 ) ;
#15269 = DIRECTION ( 'NONE',  ( 5.782411586589358625E-17, -0.000000000000000000, 1.000000000000000000 ) ) ;
#15270 = CARTESIAN_POINT ( 'NONE',  ( 135.4449143864723055, 40.00781250108393294, 13.14518615778179189 ) ) ;
#15271 = FACE_OUTER_BOUND ( 'NONE', #9575, .T. ) ;
#15272 = CARTESIAN_POINT ( 'NONE',  ( 97.92893218813452449, 94.56249999726883004, 4.999999999999983125 ) ) ;
#15273 =( BOUNDED_SURFACE ( )  B_SPLINE_SURFACE ( 1, 2, ( 
 ( #15792, #18366, #27216, #2835, #9804, #7524, #7670, #16071, #5404, #20220, #9378, #4980, #20790, #22794, #853, #14215, #3122, #22933, #9663, #18075, #13924, #16363, #26789, #24779, #3263, #3394, #12065, #7234, #1271, #15925, #9935, #18650, #13782, #5260, #7093, #13646, #26934, #22361, #2969, #11503, #12759, #18916, #1412, #7946, #19196, #25608, #27490, #1686, #25478, #27625, #20928, #12476, #14759, #19052, #10071, #8220, #18783, #23066, #21065, #10628, #7813, #16643, #8083, #5685, #16778, #3816, #6092, #27899, #14624, #3959, #12619, #5956, #8359, #21344, #25335, #23479, #3544, #27761, #27355, #5821, #17045 ),
 ( #1823, #23342, #10488, #12347, #3683, #14491, #25749, #21203, #6231, #10345, #1553, #16505, #14898, #16910, #23619, #12201, #4096, #21479, #14351, #1959, #25199, #23208, #10206, #8645, #24313, #11043, #21620, #4799, #26464, #6499, #21910, #382, #17761, #21766, #19333, #15464, #8780, #19898, #4232, #2518, #13171, #25895, #17610, #17468, #10905, #15175, #17334, #13457, #19752, #2096, #22183, #6918, #23894, #2385, #9066, #15611, #26028, #2243, #12890, #2663, #10764, #11180, #26170, #15321, #13317, #235, #28036, #8922, #19475, #28174, #26318, #19614, #6779, #8503, #99, #4373, #17188, #13029, #24178, #6365, #15037 ) ),
 .UNSPECIFIED., .F., .F., .F. ) 
 B_SPLINE_SURFACE_WITH_KNOTS ( ( 2, 2 ),
 ( 3, 2, 2, 2, 2, 2, 2, 2, 2, 2, 2, 2, 2, 2, 2, 2, 2, 2, 2, 2, 2, 2, 2, 2, 2, 2, 2, 2, 2, 2, 2, 2, 2, 2, 2, 2, 2, 2, 2, 2, 3 ),
 ( 0.000000000000000000, 1.000000000000000000 ),
 ( 0.000000000000000000, 0.02500000000000000139, 0.05000000000000000278, 0.07499999999999999722, 0.1000000000000000056, 0.1250000000000000000, 0.1499999999999999944, 0.1749999999999999889, 0.2000000000000000111, 0.2250000000000000056, 0.2500000000000000000, 0.2750000000000000222, 0.2999999999999999889, 0.3250000000000000111, 0.3499999999999999778, 0.3750000000000000000, 0.4000000000000000222, 0.4249999999999999889, 0.4500000000000000111, 0.4749999999999999778, 0.5000000000000000000, 0.5250000000000000222, 0.5500000000000000444, 0.5749999999999999556, 0.5999999999999999778, 0.6250000000000000000, 0.6500000000000000222, 0.6750000000000000444, 0.6999999999999999556, 0.7249999999999999778, 0.7500000000000000000, 0.7750000000000000222, 0.8000000000000000444, 0.8249999999999999556, 0.8499999999999999778, 0.8750000000000000000, 0.9000000000000000222, 0.9250000000000000444, 0.9499999999999999556, 0.9749999999999999778, 1.000000000000000000 ),
 .UNSPECIFIED. ) 
 GEOMETRIC_REPRESENTATION_ITEM ( )  RATIONAL_B_SPLINE_SURFACE ( (
 ( 1.000000000000000000, 0.9238795325112867385, 1.000000000000000000, 0.9238795325112867385, 1.000000000000000000, 0.9238795325112867385, 1.000000000000000000, 0.9238795325112867385, 1.000000000000000000, 0.9238795325112867385, 1.000000000000000000, 0.9238795325112867385, 1.000000000000000000, 0.9238795325112867385, 1.000000000000000000, 0.9238795325112867385, 1.000000000000000000, 0.9238795325112867385, 1.000000000000000000, 0.9238795325112867385, 1.000000000000000000, 0.9238795325112867385, 1.000000000000000000, 0.9238795325112867385, 1.000000000000000000, 0.9238795325112867385, 1.000000000000000000, 0.9238795325112867385, 1.000000000000000000, 0.9238795325112867385, 1.000000000000000000, 0.9238795325112867385, 1.000000000000000000, 0.9238795325112867385, 1.000000000000000000, 0.9238795325112867385, 1.000000000000000000, 0.9238795325112867385, 1.000000000000000000, 0.9238795325112867385, 1.000000000000000000, 0.9238795325112867385, 1.000000000000000000, 0.9238795325112867385, 1.000000000000000000, 0.9238795325112867385, 1.000000000000000000, 0.9238795325112867385, 1.000000000000000000, 0.9238795325112867385, 1.000000000000000000, 0.9238795325112867385, 1.000000000000000000, 0.9238795325112867385, 1.000000000000000000, 0.9238795325112867385, 1.000000000000000000, 0.9238795325112867385, 1.000000000000000000, 0.9238795325112867385, 1.000000000000000000, 0.9238795325112867385, 1.000000000000000000, 0.9238795325112867385, 1.000000000000000000, 0.9238795325112867385, 1.000000000000000000, 0.9238795325112867385, 1.000000000000000000, 0.9238795325112867385, 1.000000000000000000, 0.9238795325112867385, 1.000000000000000000, 0.9238795325112867385, 1.000000000000000000, 0.9238795325112867385, 1.000000000000000000, 0.9238795325112867385, 1.000000000000000000, 0.9238795325112867385, 1.000000000000000000),
 ( 1.000000000000000000, 0.9238795325112867385, 1.000000000000000000, 0.9238795325112867385, 1.000000000000000000, 0.9238795325112867385, 1.000000000000000000, 0.9238795325112867385, 1.000000000000000000, 0.9238795325112867385, 1.000000000000000000, 0.9238795325112867385, 1.000000000000000000, 0.9238795325112867385, 1.000000000000000000, 0.9238795325112867385, 1.000000000000000000, 0.9238795325112867385, 1.000000000000000000, 0.9238795325112867385, 1.000000000000000000, 0.9238795325112867385, 1.000000000000000000, 0.9238795325112867385, 1.000000000000000000, 0.9238795325112867385, 1.000000000000000000, 0.9238795325112867385, 1.000000000000000000, 0.9238795325112867385, 1.000000000000000000, 0.9238795325112867385, 1.000000000000000000, 0.9238795325112867385, 1.000000000000000000, 0.9238795325112867385, 1.000000000000000000, 0.9238795325112867385, 1.000000000000000000, 0.9238795325112867385, 1.000000000000000000, 0.9238795325112867385, 1.000000000000000000, 0.9238795325112867385, 1.000000000000000000, 0.9238795325112867385, 1.000000000000000000, 0.9238795325112867385, 1.000000000000000000, 0.9238795325112867385, 1.000000000000000000, 0.9238795325112867385, 1.000000000000000000, 0.9238795325112867385, 1.000000000000000000, 0.9238795325112867385, 1.000000000000000000, 0.9238795325112867385, 1.000000000000000000, 0.9238795325112867385, 1.000000000000000000, 0.9238795325112867385, 1.000000000000000000, 0.9238795325112867385, 1.000000000000000000, 0.9238795325112867385, 1.000000000000000000, 0.9238795325112867385, 1.000000000000000000, 0.9238795325112867385, 1.000000000000000000, 0.9238795325112867385, 1.000000000000000000, 0.9238795325112867385, 1.000000000000000000, 0.9238795325112867385, 1.000000000000000000, 0.9238795325112867385, 1.000000000000000000, 0.9238795325112867385, 1.000000000000000000) ) ) 
 REPRESENTATION_ITEM ( '' )  SURFACE ( )  );
#15274 = DIRECTION ( 'NONE',  ( -0.000000000000000000, -0.000000000000000000, -1.000000000000000000 ) ) ;
#15275 = CARTESIAN_POINT ( 'NONE',  ( 1.662435489736055498E-15, -7.395377635281828788, -13.57481594606304398 ) ) ;
#15276 = CARTESIAN_POINT ( 'NONE',  ( 208.1451861577818079, 33.21132812608393436, -1.609821015232357215E-15 ) ) ;
#15277 = EDGE_CURVE ( 'NONE', #7991, #4458, #14439, .T. ) ;
#15278 = ORIENTED_EDGE ( 'NONE', *, *, #14192, .F. ) ;
#15279 = ORIENTED_EDGE ( 'NONE', *, *, #23532, .F. ) ;
#15280 = ORIENTED_EDGE ( 'NONE', *, *, #16469, .F. ) ;
#15281 = CARTESIAN_POINT ( 'NONE',  ( 5.444914386472302859, 37.82500000108392868, 13.14518615778179189 ) ) ;
#15282 = CARTESIAN_POINT ( 'NONE',  ( 96.84719886470459471, 3.152801135295383084, 9.562500001365593860 ) ) ;
#15283 = CIRCLE ( 'NONE', #18944, 1.000000000000000888 ) ;
#15284 = CARTESIAN_POINT ( 'NONE',  ( 99.99999999999998579, 94.75000000000000000, 4.999999999999984013 ) ) ;
#15285 = CARTESIAN_POINT ( 'NONE',  ( 104.4587341249999781, 82.00000000136560629, -1.846868145590750521 ) ) ;
#15286 = CARTESIAN_POINT ( 'NONE',  ( 204.2950502721270425, 39.46210937608393010, -9.295050272127046043 ) ) ;
#15287 = CARTESIAN_POINT ( 'NONE',  ( -13.14518615778179544, 38.37070312608393152, 0.000000000000000000 ) ) ;
#15288 = CARTESIAN_POINT ( 'NONE',  ( 185.8198241863519797, 55.00000000000001421, 14.99999999999995026 ) ) ;
#15289 = CIRCLE ( 'NONE', #18523, 5.000000000000004441 ) ;
#15290 = DIRECTION ( 'NONE',  ( -0.000000000000000000, 1.000000000000000000, -0.000000000000000000 ) ) ;
#15291 = CARTESIAN_POINT ( 'NONE',  ( 200.4449143864723055, 40.50390625108394005, -13.14518615778179722 ) ) ;
#15292 = CARTESIAN_POINT ( 'NONE',  ( 93.46109445667489979, 114.7507929638356785, -46.07499999726881867 ) ) ;
#15293 = ORIENTED_EDGE ( 'NONE', *, *, #26043, .F. ) ;
#15294 = CARTESIAN_POINT ( 'NONE',  ( -13.57481594606304753, 36.18789062499999432, -5.622872871577873077 ) ) ;
#15295 = CARTESIAN_POINT ( 'NONE',  ( 2.414731522848535132E-15, 37.57695312608392868, 13.14518615778179544 ) ) ;
#15296 = ORIENTED_EDGE ( 'NONE', *, *, #6126, .F. ) ;
#15297 = CARTESIAN_POINT ( 'NONE',  ( 94.99999999999995737, -2.071067811865466624, 3.187500002731184168 ) ) ;
#15298 = CARTESIAN_POINT ( 'NONE',  ( 143.1451861577818079, 36.43593750108392726, -5.444914386472297529 ) ) ;
#15299 = CARTESIAN_POINT ( 'NONE',  ( 65.00000000000000000, 33.60820312608392868, 13.14518615778179544 ) ) ;
#15300 = CARTESIAN_POINT ( 'NONE',  ( 181.8548138422181921, 36.03906250108394005, 5.444914386472304635 ) ) ;
#15301 = ORIENTED_EDGE ( 'NONE', *, *, #13687, .F. ) ;
#15302 = PLANE ( 'NONE',  #2509 ) ;
#15303 = CARTESIAN_POINT ( 'NONE',  ( 5.444914386472302859, 32.86406250108392868, 13.14518615778179189 ) ) ;
#15304 = CARTESIAN_POINT ( 'NONE',  ( 122.3780364657951907, 54.91641323977497535, -15.00000000000000000 ) ) ;
#15305 = AXIS2_PLACEMENT_3D ( 'NONE', #26070, #17374, #6539 ) ;
#15306 = CARTESIAN_POINT ( 'NONE',  ( 5.622872871577928144, 39.16445312500000142, -13.57481594606299247 ) ) ;
#15307 = CARTESIAN_POINT ( 'NONE',  ( 99.99999999999995737, 85.00000000000000000, 4.999999999999990230 ) ) ;
#15308 = CARTESIAN_POINT ( 'NONE',  ( 91.91746824999998466, 107.3738262389971680, -51.02500000273119696 ) ) ;
#15309 = CARTESIAN_POINT ( 'NONE',  ( -13.14518615778179544, 36.58476562608393579, 0.000000000000000000 ) ) ;
#15310 = CARTESIAN_POINT ( 'NONE',  ( 99.99999999999998579, 110.0000000000000000, -45.00000000000000711 ) ) ;
#15311 = CARTESIAN_POINT ( 'NONE',  ( 103.5355339059327093, 79.50000000273119838, 3.535533905932726206 ) ) ;
#15312 = FACE_OUTER_BOUND ( 'NONE', #436, .T. ) ;
#15313 = VERTEX_POINT ( 'NONE', #22879 ) ;
#15314 = CARTESIAN_POINT ( 'NONE',  ( 104.4587341249999781, -1.846868145590721655, 6.875000001365592972 ) ) ;
#15315 = ORIENTED_EDGE ( 'NONE', *, *, #20663, .T. ) ;
#15316 = CARTESIAN_POINT ( 'NONE',  ( 97.50000000000000000, 122.7500000021849615, 1.035533905932725096 ) ) ;
#15317 = CARTESIAN_POINT ( 'NONE',  ( 96.84719886470459471, -3.152801135295355994, 10.56250000136559208 ) ) ;
#15318 = CARTESIAN_POINT ( 'NONE',  ( 128.8612318829052299, 50.00000000043912962, 13.56816686242597392 ) ) ;
#15319 = CARTESIAN_POINT ( 'NONE',  ( 13.14518615778179900, 40.10703125108393152, 5.444914386472293977 ) ) ;
#15320 = PLANE ( 'NONE',  #379 ) ;
#15321 = CARTESIAN_POINT ( 'NONE',  ( 95.54126587499995082, 80.75000000136560629, 1.846868145590724986 ) ) ;
#15322 = CARTESIAN_POINT ( 'NONE',  ( 55.70494972787295751, 35.09648437608393579, -9.295050272127046043 ) ) ;
#15323 =( BOUNDED_CURVE ( )  B_SPLINE_CURVE ( 2, ( #19500, #6522, #4398, #21789, #2269, #10373, #14925, #4120, #10928, #8528, #23645, #19638, #3983, #3839, #12785 ),
 .UNSPECIFIED., .F., .T. ) 
 B_SPLINE_CURVE_WITH_KNOTS ( ( 3, 2, 2, 2, 2, 2, 2, 3 ),
 ( 0.5416666676520737189, 0.5833333333333333703, 0.6250000000000000000, 0.6666666666666666297, 0.7083333333333333703, 0.7500000000000000000, 0.7916666666666666297, 0.8333333333333333703 ),
 .UNSPECIFIED. ) 
 CURVE ( )  GEOMETRIC_REPRESENTATION_ITEM ( )  RATIONAL_B_SPLINE_CURVE ( ( 1.000000000000000000, 0.9238795325112867385, 1.000000000000000000, 0.9238795325112867385, 1.000000000000000000, 0.9238795325112867385, 1.000000000000000000, 0.9238795325112867385, 1.000000000000000000, 0.9238795325112867385, 1.000000000000000000, 0.9238795325112867385, 1.000000000000000000, 0.9238795325112867385, 1.000000000000000000 ) ) 
 REPRESENTATION_ITEM ( '' )  );
#15324 = CARTESIAN_POINT ( 'NONE',  ( 93.46109445667491400, 105.2492070361643215, -48.92500000273119554 ) ) ;
#15325 = CARTESIAN_POINT ( 'NONE',  ( -13.14518615778179722, 38.91640625108393436, -5.444914386472297529 ) ) ;
#15326 = CARTESIAN_POINT ( 'NONE',  ( 99.99999999999995737, 80.37500000273119838, 4.999999999999990230 ) ) ;
#15327 = CARTESIAN_POINT ( 'NONE',  ( 94.99999999999995737, 1.387778780781445676E-14, 11.12500000273118594 ) ) ;
#15328 = CARTESIAN_POINT ( 'NONE',  ( 94.33688103937534208, 114.1144967660473242, -49.20000000000001705 ) ) ;
#15329 = CARTESIAN_POINT ( 'NONE',  ( 116.4251840539369454, 36.98164062499999005, -5.622872871577873077 ) ) ;
#15330 = VERTEX_POINT ( 'NONE', #12294 ) ;
#15331 = DIRECTION ( 'NONE',  ( 0.000000000000000000, 0.000000000000000000, 1.000000000000000000 ) ) ;
#15332 = CARTESIAN_POINT ( 'NONE',  ( 5.444914386472302859, 37.03125000108393294, 13.14518615778179189 ) ) ;
#15333 = CARTESIAN_POINT ( 'NONE',  ( -13.57481594606304576, 36.38632812716788578, 5.622872871577880183 ) ) ;
#15334 = CARTESIAN_POINT ( 'NONE',  ( 116.8548138422182205, 36.58476562608393579, 0.000000000000000000 ) ) ;
#15335 = CARTESIAN_POINT ( 'NONE',  ( 70.62287287157788285, 34.20351562716788862, 13.57481594606304576 ) ) ;
#15336 = ADVANCED_FACE ( 'NONE', ( #14712 ), #20599, .F. ) ;
#15337 = CARTESIAN_POINT ( 'NONE',  ( 99.99999999999998579, 137.0000000000000000, -5.204170427930421283E-15 ) ) ;
#15338 = CARTESIAN_POINT ( 'NONE',  ( -5.622872871577873077, 34.10429687716786873, 13.57481594606304753 ) ) ;
#15339 = CARTESIAN_POINT ( 'NONE',  ( 97.92893218813451028, 5.000000000000018652, 3.812500000000000000 ) ) ;
#15340 = CARTESIAN_POINT ( 'NONE',  ( 99.99999999999997158, 101.5015231886685712, -47.37499999726882294 ) ) ;
#15341 = CARTESIAN_POINT ( 'NONE',  ( 195.0000000000000000, 35.59257812608393579, -13.14518615778179544 ) ) ;
#15342 = DIRECTION ( 'NONE',  ( -0.000000000000000000, -1.000000000000000000, -0.000000000000000000 ) ) ;
#15343 = CARTESIAN_POINT ( 'NONE',  ( 5.622872871577961895, 34.50117187716787726, -13.57481594606295339 ) ) ;
#15345 = ORIENTED_EDGE ( 'NONE', *, *, #1518, .T. ) ;
#15344 = DIRECTION ( 'NONE',  ( 3.469446951953613696E-16, 0.000000000000000000, -1.000000000000000000 ) ) ;
#15346 = DIRECTION ( 'NONE',  ( -1.000000000000000000, 2.507721281754145042E-33, 7.228014483236696740E-18 ) ) ;
#15347 = CARTESIAN_POINT ( 'NONE',  ( 131.5010191243050031, 53.60014735326987534, 14.99999999999996803 ) ) ;
#15348 = CARTESIAN_POINT ( 'NONE',  ( 13.57481594606304753, 37.47773437500001137, -5.622872871577873077 ) ) ;
#15349 = CARTESIAN_POINT ( 'NONE',  ( 2.007297010069739596, 35.99999999999998579, -13.40042260803723373 ) ) ;
#15350 = CARTESIAN_POINT ( 'NONE',  ( -13.14518615778179544, 38.37070312608393152, 0.000000000000000000 ) ) ;
#15351 = CARTESIAN_POINT ( 'NONE',  ( 13.14518615778179900, 37.72578125108393721, 5.444914386472293977 ) ) ;
#15352 = CARTESIAN_POINT ( 'NONE',  ( 185.4011555911795597, 33.95546874999999432, 9.598844408820459861 ) ) ;
#15353 = ITEM_DEFINED_TRANSFORMATION ( 'NONE', 'NONE', #19496,  #26844 ) ;
#15354 = DIRECTION ( 'NONE',  ( -5.782411586589357392E-17, -0.000000000000000000, -1.000000000000000000 ) ) ;
#15355 = CARTESIAN_POINT ( 'NONE',  ( 143.5748159460630688, 36.58476562499999574, 5.622872871577868636 ) ) ;
#15356 = CARTESIAN_POINT ( 'NONE',  ( 51.85481384221819923, 34.15390625108393863, -5.444914386472297529 ) ) ;
#15357 = CARTESIAN_POINT ( 'NONE',  ( 95.54126587499996504, 1.387778780781445676E-14, 2.437500001365592084 ) ) ;
#15358 = CARTESIAN_POINT ( 'NONE',  ( 95.67376207875072680, 115.9545556584642867, -44.80000000546236549 ) ) ;
#15359 = CARTESIAN_POINT ( 'NONE',  ( 101.8468681455907330, 93.49999999863442213, -4.458734124999994997 ) ) ;
#15360 = CARTESIAN_POINT ( 'NONE',  ( 3.061616997868384226E-15, 23.00000000000000000, 25.00000000000001066 ) ) ;
#15361 = CARTESIAN_POINT ( 'NONE',  ( 13.57481594606304931, 34.99726562500000426, 5.622872871577869525 ) ) ;
#15362 = CARTESIAN_POINT ( 'NONE',  ( 143.1451861577818079, 36.43593750108392726, -5.444914386472297529 ) ) ;
#15363 = VERTEX_POINT ( 'NONE', #1497 ) ;
#15364 = CARTESIAN_POINT ( 'NONE',  ( 102.0710678118654329, 84.31250000000001421, 4.999999999999989342 ) ) ;
#15365 = CARTESIAN_POINT ( 'NONE',  ( 97.92893218813451028, 80.93750000273119838, -5.000000000000018652 ) ) ;
#15366 = CARTESIAN_POINT ( 'NONE',  ( 104.4587341249999923, 94.24999999863439371, 1.846868145590726318 ) ) ;
#15367 = CARTESIAN_POINT ( 'NONE',  ( 53.85445312690458763, 36.00000000000000000, -7.260818043107227560 ) ) ;
#15368 = AXIS2_PLACEMENT_3D ( 'NONE', #5820, #3815, #1685 ) ;
#15369 = CARTESIAN_POINT ( 'NONE',  ( 97.83688103937537051, 103.3426043859339103, -50.60000000000001563 ) ) ;
#15370 = CARTESIAN_POINT ( 'NONE',  ( 65.00000000000000000, 33.80664062608393294, 13.14518615778179544 ) ) ;
#15371 = ORIENTED_EDGE ( 'NONE', *, *, #18711, .F. ) ;
#15372 = EDGE_CURVE ( 'NONE', #8183, #210, #622, .T. ) ;
#15373 = CARTESIAN_POINT ( 'NONE',  ( 143.5748159460630688, 39.06523437716786873, 5.622872871577868636 ) ) ;
#15374 = CARTESIAN_POINT ( 'NONE',  ( 99.99999999999995737, -4.458734124999988779, 2.937500001365592528 ) ) ;
#15375 = EDGE_CURVE ( 'NONE', #15622, #2100, #7514, .T. ) ;
#15376 = VERTEX_POINT ( 'NONE', #12981 ) ;
#15377 = CARTESIAN_POINT ( 'NONE',  ( 13.14518615778179722, 32.46718750108393436, -5.444914386472297529 ) ) ;
#15378 = CARTESIAN_POINT ( 'NONE',  ( -5.444914386472297529, 39.01562500108394005, -13.14518615778179900 ) ) ;
#15379 = CARTESIAN_POINT ( 'NONE',  ( 200.6228728715778686, 36.08867187716787583, -13.57481594606304753 ) ) ;
#15380 = CARTESIAN_POINT ( 'NONE',  ( -9.295050272127046043, 35.69179687608393436, -9.295050272127046043 ) ) ;
#15381 = CARTESIAN_POINT ( 'NONE',  ( -13.57481594606304398, 32.31835937499999289, 5.622872871577880183 ) ) ;
#15382 = CARTESIAN_POINT ( 'NONE',  ( 130.0000000000000000, 37.77539062608393294, 13.14518615778179544 ) ) ;
#15383 = ORIENTED_EDGE ( 'NONE', *, *, #9004, .T. ) ;
#15384 = CARTESIAN_POINT ( 'NONE',  ( 5.444914386472302859, 39.41250000108393436, 13.14518615778179189 ) ) ;
#15385 = CARTESIAN_POINT ( 'NONE',  ( 116.8548138422182063, 34.25312500108393010, 5.444914386472304635 ) ) ;
#15386 = CARTESIAN_POINT ( 'NONE',  ( 51.42518405393695957, 35.49335937499999005, 5.622872871577880183 ) ) ;
#15387 = CARTESIAN_POINT ( 'NONE',  ( 104.9999999999999716, 92.06249999999998579, -2.071067811865478170 ) ) ;
#15388 = AXIS2_PLACEMENT_3D ( 'NONE', #12033, #21169, #16881 ) ;
#15389 = ADVANCED_FACE ( 'NONE', ( #23708 ), #19703, .T. ) ;
#15390 = CARTESIAN_POINT ( 'NONE',  ( 98.15313185440925281, -4.458734124999987891, 10.87500000136559386 ) ) ;
#15391 = CARTESIAN_POINT ( 'NONE',  ( 185.4011555911795597, 37.13046874999999147, 9.598844408820459861 ) ) ;
#15392 = CARTESIAN_POINT ( 'NONE',  ( 98.15313185440923860, -4.458734124999987891, 13.62500000136559208 ) ) ;
#15393 = CARTESIAN_POINT ( 'NONE',  ( 104.9952793366501851, 116.8754121666685393, -53.82500000273119412 ) ) ;
#15394 = AXIS2_PLACEMENT_3D ( 'NONE', #25428, #5769, #21290 ) ;
#15395 = CARTESIAN_POINT ( 'NONE',  ( 13.57481594606304753, 39.16445312716788152, -5.622872871577873966 ) ) ;
#15396 = CARTESIAN_POINT ( 'NONE',  ( 214.9999999999999716, 55.00000000000000000, 9.999999999999946709 ) ) ;
#15397 = CARTESIAN_POINT ( 'NONE',  ( 106.5389055433250860, 105.2492070361643215, -48.82499999726882578 ) ) ;
#15398 = CARTESIAN_POINT ( 'NONE',  ( -9.295050272127046043, 35.09648437608393579, -9.295050272127046043 ) ) ;
#15399 = CARTESIAN_POINT ( 'NONE',  ( 97.50236033167490746, 102.3130555110000159, -51.47499999726882436 ) ) ;
#15400 = ORIENTED_EDGE ( 'NONE', *, *, #25502, .F. ) ;
#15401 = CARTESIAN_POINT ( 'NONE',  ( 107.0000000000000142, 110.0000000000000000, -51.50000000546237544 ) ) ;
#15402 = DIRECTION ( 'NONE',  ( 0.000000000000000000, -1.000000000000000000, 3.469446951953611231E-16 ) ) ;
#15403 = CARTESIAN_POINT ( 'NONE',  ( 94.99999999999998579, 110.0000000000000000, -145.0000000000000284 ) ) ;
#15404 = CARTESIAN_POINT ( 'NONE',  ( 200.4449143864723055, 40.30546875108393579, -13.14518615778179900 ) ) ;
#15405 = ORIENTED_EDGE ( 'NONE', *, *, #18628, .F. ) ;
#15406 = ADVANCED_FACE ( 'NONE', ( #189 ), #25166, .F. ) ;
#15407 = LINE ( 'NONE', #10984, #22920 ) ;
#15408 = CARTESIAN_POINT ( 'NONE',  ( 187.3834746745192206, 54.91574374957786375, -15.00000000000000178 ) ) ;
#15409 = CARTESIAN_POINT ( 'NONE',  ( 103.1528011352953342, -3.152801135295355106, 14.06250000136559208 ) ) ;
#15410 = VERTEX_POINT ( 'NONE', #6872 ) ;
#15411 = CARTESIAN_POINT ( 'NONE',  ( 107.0000000000000142, 110.0000000000000000, -49.00000000000000711 ) ) ;
#15412 = CARTESIAN_POINT ( 'NONE',  ( -8.049105076161786076E-16, 38.76757812608393294, -13.14518615778179544 ) ) ;
#15413 = AXIS2_PLACEMENT_3D ( 'NONE', #21229, #12372, #1713 ) ;
#15414 = CARTESIAN_POINT ( 'NONE',  ( 99.99999999999998579, 122.9500000010924765, -2.066987299999998751 ) ) ;
#15415 = EDGE_CURVE ( 'NONE', #9571, #499, #7214, .T. ) ;
#15416 = CARTESIAN_POINT ( 'NONE',  ( 124.3771271284221314, 31.72304687716787441, 13.57481594606304753 ) ) ;
#15417 = DIRECTION ( 'NONE',  ( 0.000000000000000000, 1.000000000000000000, 0.000000000000000000 ) ) ;
#15418 = CARTESIAN_POINT ( 'NONE',  ( 95.00000000000000000, 92.43749999726878741, 2.071067811865463959 ) ) ;
#15419 = CARTESIAN_POINT ( 'NONE',  ( 51.85481384221820633, 38.42031250108393436, 5.444914386472304635 ) ) ;
#15420 = DIRECTION ( 'NONE',  ( 0.000000000000000000, 0.000000000000000000, -1.000000000000000000 ) ) ;
#15421 = CARTESIAN_POINT ( 'NONE',  ( 185.7049497278729575, 34.50117187608393721, 9.295050272127047819 ) ) ;
#15422 = EDGE_CURVE ( 'NONE', #15363, #7335, #5537, .T. ) ;
#15423 = ORIENTED_EDGE ( 'NONE', *, *, #3286, .T. ) ;
#15424 = CARTESIAN_POINT ( 'NONE',  ( 5.444914386472302859, 39.41250000108393436, 13.14518615778179189 ) ) ;
#15425 = CARTESIAN_POINT ( 'NONE',  ( 0.000000000000000000, 0.000000000000000000, 0.000000000000000000 ) ) ;
#15426 = CARTESIAN_POINT ( 'NONE',  ( 95.54126587499996504, -1.846868145590724986, 11.75000000136559208 ) ) ;
#15427 = CARTESIAN_POINT ( 'NONE',  ( 102.0710678118655181, 94.81250000000000000, 4.999999999999919176 ) ) ;
#15428 = CARTESIAN_POINT ( 'NONE',  ( 99.99999999999995737, 81.68750000136559208, 4.458734124999988779 ) ) ;
#15429 = CARTESIAN_POINT ( 'NONE',  ( 195.0000000000000000, 37.97382812608393721, -13.14518615778179544 ) ) ;
#15430 = CARTESIAN_POINT ( 'NONE',  ( -13.14518615778179189, 37.62656250108393152, 5.444914386472304635 ) ) ;
#15431 = CARTESIAN_POINT ( 'NONE',  ( -5.622872871577947684, 39.36289062716787157, -13.57481594606297293 ) ) ;
#15432 = VECTOR ( 'NONE', #8493, 1000.000000000000000 ) ;
#15433 = LINE ( 'NONE', #17729, #19845 ) ;
#15434 = CARTESIAN_POINT ( 'NONE',  ( 74.59884440882045453, 39.71015624999999716, 9.598844408820456309 ) ) ;
#15435 = CARTESIAN_POINT ( 'NONE',  ( 95.00472066334982912, 116.8754121666685393, -53.92499999726881299 ) ) ;
#15436 = VERTEX_POINT ( 'NONE', #11698 ) ;
#15437 = CARTESIAN_POINT ( 'NONE',  ( 13.57481594606304576, 35.84062499999999574, -1.662435489736055892E-15 ) ) ;
#15438 = CARTESIAN_POINT ( 'NONE',  ( 13.14518615778179900, 36.13828125108393863, 5.444914386472293977 ) ) ;
#15439 = ORIENTED_EDGE ( 'NONE', *, *, #18240, .F. ) ;
#15440 = CARTESIAN_POINT ( 'NONE',  ( 120.7049497278729575, 36.68398437608393436, -9.295050272127046043 ) ) ;
#15441 = CARTESIAN_POINT ( 'NONE',  ( 51.85481384221820633, 34.25312500108393010, 5.444914386472304635 ) ) ;
#15442 = CIRCLE ( 'NONE', #25098, 4.999999999999999112 ) ;
#15443 = CARTESIAN_POINT ( 'NONE',  ( 204.2950502721270425, 38.07304687608393579, -9.295050272127046043 ) ) ;
#15444 = ORIENTED_EDGE ( 'NONE', *, *, #12266, .T. ) ;
#15445 = DIRECTION ( 'NONE',  ( -1.000000000000000000, 0.000000000000000000, 0.000000000000000000 ) ) ;
#15446 = CARTESIAN_POINT ( 'NONE',  ( 13.14518615778179544, 32.21914062608393436, -1.609821015232357215E-15 ) ) ;
#15447 = CARTESIAN_POINT ( 'NONE',  ( 133.1146977455429692, 53.90847045361285694, -15.00000000000000000 ) ) ;
#15448 =( BOUNDED_CURVE ( )  B_SPLINE_CURVE ( 2, ( #12514, #1724, #27936, #14795, #25787, #12660, #23246, #12385, #21387 ),
 .UNSPECIFIED., .F., .F. ) 
 B_SPLINE_CURVE_WITH_KNOTS ( ( 3, 2, 2, 2, 3 ),
 ( 0.1458333333333336757, 0.1562500000000002776, 0.1666666666666669072, 0.1770833333333335369, 0.1875000000000001388 ),
 .UNSPECIFIED. ) 
 CURVE ( )  GEOMETRIC_REPRESENTATION_ITEM ( )  RATIONAL_B_SPLINE_CURVE ( ( 0.9999999999999975575, 0.9238795325112891810, 1.000000000000000000, 0.9238795325112867385, 1.000000000000000000, 0.9238795325112867385, 1.000000000000000000, 0.9238795325112857393, 1.000000000000001110 ) ) 
 REPRESENTATION_ITEM ( '' )  );
#15449 = ADVANCED_FACE ( 'NONE', ( #13700 ), #11557, .T. ) ;
#15450 = DIRECTION ( 'NONE',  ( 0.000000000000000000, 1.000000000000000000, 0.000000000000000000 ) ) ;
#15451 = CARTESIAN_POINT ( 'NONE',  ( 130.0000000000000000, 40.10703125216787157, -13.57481594606304576 ) ) ;
#15452 = CARTESIAN_POINT ( 'NONE',  ( 99.99999999999998579, 118.4984768113314146, -53.62500000273119838 ) ) ;
#15453 = ORIENTED_EDGE ( 'NONE', *, *, #8987, .T. ) ;
#15454 = DIRECTION ( 'NONE',  ( 0.000000000000000000, 0.000000000000000000, 1.000000000000000000 ) ) ;
#15455 = CARTESIAN_POINT ( 'NONE',  ( 97.50000000000000000, 123.5500000021849587, 1.035533905932725096 ) ) ;
#15456 = CARTESIAN_POINT ( 'NONE',  ( 94.99999999999994316, -2.071067811865456409, 10.06249999999999645 ) ) ;
#15457 = VECTOR ( 'NONE', #23445, 1000.000000000000000 ) ;
#15458 = CARTESIAN_POINT ( 'NONE',  ( 104.4587341249999639, 1.442382525525748735E-14, 9.937500001365592084 ) ) ;
#15459 = CARTESIAN_POINT ( 'NONE',  ( 102.4999999999999716, 123.0500000021849445, 1.035533905932722876 ) ) ;
#15460 = CARTESIAN_POINT ( 'NONE',  ( 95.54126587499995082, -1.846868145590724986, 11.50000000136559208 ) ) ;
#15461 = CARTESIAN_POINT ( 'NONE',  ( 126.8853022544570450, 53.90847045361285694, 14.99999999999996447 ) ) ;
#15462 = CARTESIAN_POINT ( 'NONE',  ( -5.444914386472297529, 38.81718750108393579, -13.14518615778179900 ) ) ;
#15463 = DIRECTION ( 'NONE',  ( 0.000000000000000000, 0.000000000000000000, 1.000000000000000000 ) ) ;
#15464 = CARTESIAN_POINT ( 'NONE',  ( 98.15313185440925281, 82.50000000136560629, -4.458734125000016313 ) ) ;
#15465 = CARTESIAN_POINT ( 'NONE',  ( 74.29505027212704249, 34.10429687608393579, -9.295050272127046043 ) ) ;
#15466 = CARTESIAN_POINT ( 'NONE',  ( 97.50236033167492167, 102.3130555110000159, -44.97500000273119980 ) ) ;
#15467 = CARTESIAN_POINT ( 'NONE',  ( 5.444914386472302859, 38.42031250108393436, 13.14518615778179189 ) ) ;
#15468 = CARTESIAN_POINT ( 'NONE',  ( -9.598844408820454532, 39.51171874999999289, 9.598844408820459861 ) ) ;
#15469 = CARTESIAN_POINT ( 'NONE',  ( 2.493653234604083739E-15, 39.71015625216787015, 13.57481594606304576 ) ) ;
#15470 = CARTESIAN_POINT ( 'NONE',  ( 107.0000000000000000, 110.0000000000000000, -55.49999999453763877 ) ) ;
#15471 = CARTESIAN_POINT ( 'NONE',  ( 116.4251840539369454, 38.56914062500000284, -5.622872871577873077 ) ) ;
#15472 = ORIENTED_EDGE ( 'NONE', *, *, #15947, .F. ) ;
#15473 = CARTESIAN_POINT ( 'NONE',  ( 99.99999999999995737, 83.75000000000000000, -5.000000000000018652 ) ) ;
#15474 = CARTESIAN_POINT ( 'NONE',  ( 13.14518615778179900, 37.92421875108392726, 5.444914386472293977 ) ) ;
#15475 = CARTESIAN_POINT ( 'NONE',  ( 13.57481594606304576, 35.93984375216787441, -1.662435489736055892E-15 ) ) ;
#15476 = CARTESIAN_POINT ( 'NONE',  ( 94.99999999999995737, 1.387778780781445676E-14, 8.125000002731185944 ) ) ;
#15477 = CARTESIAN_POINT ( 'NONE',  ( 120.7049497278729575, 38.07304687608393579, -9.295050272127046043 ) ) ;
#15478 = CARTESIAN_POINT ( 'NONE',  ( 65.00000000000000000, 34.94765625216787441, 13.57481594606304576 ) ) ;
#15479 = CIRCLE ( 'NONE', #3195, 1.000000000000000888 ) ;
#15480 = ORIENTED_EDGE ( 'NONE', *, *, #25386, .T. ) ;
#15481 = CARTESIAN_POINT ( 'NONE',  ( 13.01985494039077729, 35.99999999999995026, 3.369129453355339976 ) ) ;
#15482 = CARTESIAN_POINT ( 'NONE',  ( 9.598844408820459861, 33.45937500216787441, 9.598844408820456309 ) ) ;
#15483 = CARTESIAN_POINT ( 'NONE',  ( 1.662435489736055892E-15, 40.99999999999999289, 13.57481594606304576 ) ) ;
#15484 = CARTESIAN_POINT ( 'NONE',  ( 91.91746824999997045, 112.6261737610028320, -47.97499999726881725 ) ) ;
#15485 = CARTESIAN_POINT ( 'NONE',  ( 189.5550856135277229, 34.05468750108393294, -13.14518615778179900 ) ) ;
#15486 = DIRECTION ( 'NONE',  ( 0.000000000000000000, 0.000000000000000000, -1.000000000000000000 ) ) ;
#15487 = DIRECTION ( 'NONE',  ( 5.782411586589357392E-17, 0.000000000000000000, 1.000000000000000000 ) ) ;
#15488 = VERTEX_POINT ( 'NONE', #15982 ) ;
#15490 = VERTEX_POINT ( 'NONE', #24696 ) ;
#15489 = DIRECTION ( 'NONE',  ( -0.000000000000000000, 1.000000000000000000, -0.000000000000000000 ) ) ;
#15491 =( BOUNDED_CURVE ( )  B_SPLINE_CURVE ( 2, ( #28166, #89, #8770, #2508, #12880, #17602, #8911, #19467, #17459 ),
 .UNSPECIFIED., .F., .F. ) 
 B_SPLINE_CURVE_WITH_KNOTS ( ( 3, 2, 2, 2, 3 ),
 ( 0.3958333333333331483, 0.4062499999999999445, 0.4166666666666667407, 0.4270833333333335369, 0.4375000000000003331 ),
 .UNSPECIFIED. ) 
 CURVE ( )  GEOMETRIC_REPRESENTATION_ITEM ( )  RATIONAL_B_SPLINE_CURVE ( ( 1.000000000000001110, 0.9238795325112855172, 1.000000000000000000, 0.9238795325112867385, 1.000000000000000000, 0.9238795325112867385, 1.000000000000000000, 0.9238795325112842960, 1.000000000000002442 ) ) 
 REPRESENTATION_ITEM ( '' )  );
#15492 = CARTESIAN_POINT ( 'NONE',  ( 6.944426393311537993, 31.75150625057403175, -11.16113171639042356 ) ) ;
#15493 = B_SPLINE_CURVE_WITH_KNOTS ( 'NONE', 3,
 ( #25504, #22963, #27516, #3425 ),
 .UNSPECIFIED., .F., .F.,
 ( 4, 4 ),
 ( 0.000000000000000000, 1.000000000000000000 ),
 .UNSPECIFIED. ) ;
#15494 = CARTESIAN_POINT ( 'NONE',  ( 204.5988444088204403, 39.21406250216787015, -9.598844408820458085 ) ) ;
#15495 = CARTESIAN_POINT ( 'NONE',  ( -13.57481594606304576, 37.03124999999999289, 0.000000000000000000 ) ) ;
#15496 = CARTESIAN_POINT ( 'NONE',  ( 92.99999999999998579, 110.0000000000000000, -45.00000000000001421 ) ) ;
#15497 = CARTESIAN_POINT ( 'NONE',  ( 5.444914386472302859, 37.82500000108392868, 13.14518615778179189 ) ) ;
#15498 = CARTESIAN_POINT ( 'NONE',  ( -5.444914386472297529, 35.64218750108392442, -13.14518615778179900 ) ) ;
#15499 = CARTESIAN_POINT ( 'NONE',  ( 200.6228728715778686, 35.19570312499999432, -13.57481594606304753 ) ) ;
#15500 = VECTOR ( 'NONE', #13772, 1000.000000000000000 ) ;
#15501 = DIRECTION ( 'NONE',  ( 0.000000000000000000, -1.000000000000000000, -1.040834085586084848E-15 ) ) ;
#15502 = DIRECTION ( 'NONE',  ( 0.000000000000000000, 1.000000000000000000, 0.000000000000000000 ) ) ;
#15503 = CARTESIAN_POINT ( 'NONE',  ( 51.85481384221820633, 34.99726562608393721, 0.000000000000000000 ) ) ;
#15504 = ADVANCED_FACE ( 'NONE', ( #1325 ), #18970, .F. ) ;
#15505 = CARTESIAN_POINT ( 'NONE',  ( 103.1528011352953342, 3.152801135295383084, 4.062500001365592084 ) ) ;
#15506 = CARTESIAN_POINT ( 'NONE',  ( 101.1641122485766999, 123.0000000000000284, -2.217301332870669217 ) ) ;
#15507 = ORIENTED_EDGE ( 'NONE', *, *, #14517, .F. ) ;
#15508 = CARTESIAN_POINT ( 'NONE',  ( 96.46446609406726225, 93.24999999726881583, -3.535533905932738197 ) ) ;
#15509 = CARTESIAN_POINT ( 'NONE',  ( -8.312177448680279460E-16, 35.24531249999999716, -13.57481594606304576 ) ) ;
#15510 = CARTESIAN_POINT ( 'NONE',  ( 124.5550856135277087, 36.13828125108393863, 13.14518615778179722 ) ) ;
#15511 = ORIENTED_EDGE ( 'NONE', *, *, #23138, .T. ) ;
#15512 = VERTEX_POINT ( 'NONE', #16698 ) ;
#15513 = CARTESIAN_POINT ( 'NONE',  ( 104.9999999999999716, 83.50000000000000000, -1.449011120738813565E-14 ) ) ;
#15514 = VECTOR ( 'NONE', #23993, 1000.000000000000000 ) ;
#15515 = CARTESIAN_POINT ( 'NONE',  ( 94.99999999999995737, 84.06250000273119838, -2.071067811865491048 ) ) ;
#15516 = CARTESIAN_POINT ( 'NONE',  ( 104.4587341249999923, 93.37499999863439371, -1.846868145590737198 ) ) ;
#15517 = CARTESIAN_POINT ( 'NONE',  ( 103.1528011352953484, 94.68749999863440792, -3.152801135295366208 ) ) ;
#15518 = CARTESIAN_POINT ( 'NONE',  ( 107.0000000000000000, 112.2744378736303332, -49.90000000000000568 ) ) ;
#15519 = CARTESIAN_POINT ( 'NONE',  ( 51.42518405393695957, 40.15664062500000142, -5.622872871577873077 ) ) ;
#15520 = EDGE_LOOP ( 'NONE', ( #3730, #16724, #25523, #11474 ) ) ;
#15521 = CARTESIAN_POINT ( 'NONE',  ( 139.5988444088204687, 39.01562500216787299, 9.598844408820456309 ) ) ;
#15522 = CARTESIAN_POINT ( 'NONE',  ( 97.92893218813451028, 5.000000000000018652, 12.81249999999999822 ) ) ;
#15523 = ORIENTED_EDGE ( 'NONE', *, *, #27672, .F. ) ;
#15524 = CARTESIAN_POINT ( 'NONE',  ( -13.14518615778179189, 32.86406250108393579, 5.444914386472304635 ) ) ;
#15525 = CARTESIAN_POINT ( 'NONE',  ( -13.14518615778179189, 40.00781250108393294, 5.444914386472304635 ) ) ;
#15526 = UNCERTAINTY_MEASURE_WITH_UNIT (LENGTH_MEASURE( 1.000000000000000082E-05 ), #1949, 'distance_accuracy_value', 'NONE');
#15527 = CARTESIAN_POINT ( 'NONE',  ( 208.5748159460630688, 33.55859375216787299, -1.662435489736055892E-15 ) ) ;
#15528 = CARTESIAN_POINT ( 'NONE',  ( 9.295050272127046043, 36.28710937608393294, -9.295050272127046043 ) ) ;
#15529 = CARTESIAN_POINT ( 'NONE',  ( 99.99999999999995737, 80.00000000000000000, -1.387778780781445676E-14 ) ) ;
#15530 = ORIENTED_EDGE ( 'NONE', *, *, #5841, .T. ) ;
#15531 = CARTESIAN_POINT ( 'NONE',  ( -5.444914386472299306, 34.55078125108393294, 13.14518615778179722 ) ) ;
#15532 = CARTESIAN_POINT ( 'NONE',  ( 120.7049497278729575, 34.89804687608393152, -9.295050272127046043 ) ) ;
#15533 = CARTESIAN_POINT ( 'NONE',  ( 51.42518405393695957, 33.80664062500000000, -5.622872871577873077 ) ) ;
#15534 = DIRECTION ( 'NONE',  ( 1.000000000000000000, 0.000000000000000000, -7.228014483236696740E-18 ) ) ;
#15535 = CARTESIAN_POINT ( 'NONE',  ( 103.1528011352953342, -3.152801135295355106, 10.06250000136559386 ) ) ;
#15536 = DIRECTION ( 'NONE',  ( 0.000000000000000000, -1.000000000000000000, 0.000000000000000000 ) ) ;
#15537 = CARTESIAN_POINT ( 'NONE',  ( 95.54126587499996504, 1.387778780781445676E-14, 12.43750000136559208 ) ) ;
#15538 = CARTESIAN_POINT ( 'NONE',  ( 104.3262379212492590, 115.9545556584642867, -53.20000000546237118 ) ) ;
#15539 = LINE ( 'NONE', #4306, #4530 ) ;
#15540 = CARTESIAN_POINT ( 'NONE',  ( 107.5412658750000077, 110.0000000000000000, -44.68750000136559919 ) ) ;
#15541 = CARTESIAN_POINT ( 'NONE',  ( 99.99999999999997158, 118.4984768113314146, -48.12499999726881583 ) ) ;
#15542 = CARTESIAN_POINT ( 'NONE',  ( 13.14518615778179900, 36.43593750108392726, -5.444914386472297529 ) ) ;
#15543 = CARTESIAN_POINT ( 'NONE',  ( 104.9952793366501709, 103.1245878333314323, -53.17499999726882010 ) ) ;
#15544 = ORIENTED_EDGE ( 'NONE', *, *, #19113, .T. ) ;
#15545 = EDGE_CURVE ( 'NONE', #7822, #20854, #24835, .T. ) ;
#15546 = CARTESIAN_POINT ( 'NONE',  ( 97.93301270000000613, 123.1000000010924822, -0.8561741729129506151 ) ) ;
#15547 = CARTESIAN_POINT ( 'NONE',  ( 124.3771271284221314, 36.98164062716787015, -13.57481594606304753 ) ) ;
#15548 = FACE_OUTER_BOUND ( 'NONE', #3065, .T. ) ;
#15549 = CARTESIAN_POINT ( 'NONE',  ( 208.1451861577817795, 36.23750000108393010, -5.444914386472297529 ) ) ;
#15550 = ORIENTED_EDGE ( 'NONE', *, *, #10490, .F. ) ;
#15551 = DIRECTION ( 'NONE',  ( 1.000000000000000000, 0.000000000000000000, 0.000000000000000000 ) ) ;
#15552 = CARTESIAN_POINT ( 'NONE',  ( 202.6239419619254818, 55.00000000000001421, -15.00000000000000711 ) ) ;
#15553 = LINE ( 'NONE', #27985, #2114 ) ;
#15554 = ORIENTED_EDGE ( 'NONE', *, *, #4251, .T. ) ;
#15555 = CARTESIAN_POINT ( 'NONE',  ( 95.00472066334982912, 103.1245878333314323, -51.07500000273118701 ) ) ;
#15556 = CARTESIAN_POINT ( 'NONE',  ( -5.444914386472299306, 39.90859375108393436, 13.14518615778179722 ) ) ;
#15557 = CARTESIAN_POINT ( 'NONE',  ( 99.99999999999998579, 110.0000000000000000, -45.00000000000000711 ) ) ;
#15558 = CARTESIAN_POINT ( 'NONE',  ( 124.3771271284221314, 31.42539062716787157, -13.57481594606304753 ) ) ;
#15559 = CARTESIAN_POINT ( 'NONE',  ( -13.14518615778179544, 39.95820312608393010, 0.000000000000000000 ) ) ;
#15560 = EDGE_CURVE ( 'NONE', #17002, #10602, #5707, .T. ) ;
#15561 = CARTESIAN_POINT ( 'NONE',  ( 104.9999999999999716, 91.93749999726880162, -2.071067811865478170 ) ) ;
#15562 = CARTESIAN_POINT ( 'NONE',  ( 70.44491438647230552, 37.03125000108393294, 13.14518615778179189 ) ) ;
#15563 = CARTESIAN_POINT ( 'NONE',  ( 60.49511291368164478, 51.44650206077175625, -15.00000000000199130 ) ) ;
#15564 = VERTEX_POINT ( 'NONE', #5601 ) ;
#15565 = VECTOR ( 'NONE', #25500, 1000.000000000000000 ) ;
#15566 = CARTESIAN_POINT ( 'NONE',  ( 200.6228728715778686, 39.95820312499999716, -13.57481594606304753 ) ) ;
#15567 = CARTESIAN_POINT ( 'NONE',  ( -15.00000000000000000, 75.00000000000000000, 10.00000000000000000 ) ) ;
#15568 = ORIENTED_EDGE ( 'NONE', *, *, #1814, .F. ) ;
#15569 = VERTEX_POINT ( 'NONE', #14408 ) ;
#15570 = CARTESIAN_POINT ( 'NONE',  ( -13.14518615778179189, 38.42031250108393436, 5.444914386472304635 ) ) ;
#15571 = CARTESIAN_POINT ( 'NONE',  ( 103.1528011352953342, -3.152801135295355106, 13.06250000136559208 ) ) ;
#15572 = EDGE_CURVE ( 'NONE', #8963, #26902, #3534, .T. ) ;
#15573 = CARTESIAN_POINT ( 'NONE',  ( 99.99999999999998579, 91.25000000000000000, -4.999999999999997335 ) ) ;
#15574 = CARTESIAN_POINT ( 'NONE',  ( 200.4449143864723055, 37.92421875108393436, -13.14518615778179722 ) ) ;
#15575 = ADVANCED_FACE ( 'NONE', ( #3736 ), #20984, .T. ) ;
#15576 = CARTESIAN_POINT ( 'NONE',  ( 9.295050272127047819, 37.87460937608393863, 9.295050272127046043 ) ) ;
#15577 = CARTESIAN_POINT ( 'NONE',  ( 101.8468681455907330, 90.74999999863439371, -4.458734124999994997 ) ) ;
#15578 = CARTESIAN_POINT ( 'NONE',  ( 181.8548138422182205, 36.73359375108393010, -5.444914386472297529 ) ) ;
#15579 = CARTESIAN_POINT ( 'NONE',  ( 104.9952793366501709, 116.8754121666685393, -50.32499999726882578 ) ) ;
#15580 = EDGE_CURVE ( 'NONE', #19007, #6540, #9040, .T. ) ;
#15581 = EDGE_LOOP ( 'NONE', ( #17495, #5910, #21867, #16827 ) ) ;
#15582 = CARTESIAN_POINT ( 'NONE',  ( -8.312177448680279460E-16, 35.24531249999999716, -13.57481594606304576 ) ) ;
#15583 = CARTESIAN_POINT ( 'NONE',  ( 9.295050272127046043, 37.08085937608393579, -9.295050272127046043 ) ) ;
#15584 = ORIENTED_EDGE ( 'NONE', *, *, #5151, .F. ) ;
#15585 = CARTESIAN_POINT ( 'NONE',  ( 116.8548138422182063, 33.65781250108393152, 5.444914386472304635 ) ) ;
#15586 = CARTESIAN_POINT ( 'NONE',  ( 59.55508561352770158, 33.55859375108393294, 13.14518615778179722 ) ) ;
#15587 = AXIS2_PLACEMENT_3D ( 'NONE', #18463, #1228, #16733 ) ;
#15588 = EDGE_CURVE ( 'NONE', #439, #1089, #16275, .T. ) ;
#15589 = CARTESIAN_POINT ( 'NONE',  ( 195.0000000000000000, 37.37851562608393863, -13.14518615778179544 ) ) ;
#15590 = ORIENTED_EDGE ( 'NONE', *, *, #19754, .F. ) ;
#15591 = CARTESIAN_POINT ( 'NONE',  ( 100.8561741729129437, 123.2000000010924765, 2.066987299999979655 ) ) ;
#15592 = CARTESIAN_POINT ( 'NONE',  ( -5.444914386472297529, 31.67343750108393863, -13.14518615778179900 ) ) ;
#15593 = CARTESIAN_POINT ( 'NONE',  ( 99.99999988184244160, 117.0000000000000000, -45.00000000000000711 ) ) ;
#15594 = DIRECTION ( 'NONE',  ( 0.000000000000000000, 0.000000000000000000, 1.000000000000000000 ) ) ;
#15595 = CARTESIAN_POINT ( 'NONE',  ( 93.46109445667491400, 105.2492070361643215, -52.92500000273119554 ) ) ;
#15596 = LINE ( 'NONE', #20175, #8350 ) ;
#15597 = DIRECTION ( 'NONE',  ( -0.000000000000000000, 1.000000000000000000, -0.000000000000000000 ) ) ;
#15598 = CARTESIAN_POINT ( 'NONE',  ( 181.8548138422181921, 40.00781250108393294, 5.444914386472304635 ) ) ;
#15599 = EDGE_CURVE ( 'NONE', #18726, #949, #11846, .T. ) ;
#15600 = ORIENTED_EDGE ( 'NONE', *, *, #1090, .T. ) ;
#15601 = SURFACE_STYLE_FILL_AREA ( #22607 ) ;
#15602 = CARTESIAN_POINT ( 'NONE',  ( 95.54126587499995082, -1.846868145590724986, 6.500000001365592084 ) ) ;
#15603 = ORIENTED_EDGE ( 'NONE', *, *, #26376, .T. ) ;
#15604 = CARTESIAN_POINT ( 'NONE',  ( 102.0669872999999939, 123.3000000010924850, 0.8561741729129311862 ) ) ;
#15605 = CARTESIAN_POINT ( 'NONE',  ( 101.8468681455906903, 4.458734125000016313, 7.125000001365591196 ) ) ;
#15606 = CARTESIAN_POINT ( 'NONE',  ( 120.8198241863519797, 50.00000000000000000, 14.99999999999996447 ) ) ;
#15607 = VECTOR ( 'NONE', #2985, 1000.000000000000000 ) ;
#15608 = ADVANCED_FACE ( 'NONE', ( #25250 ), #10417, .T. ) ;
#15609 = CARTESIAN_POINT ( 'NONE',  ( 13.14518615778179900, 36.93203125108394147, 5.444914386472293977 ) ) ;
#15610 = CARTESIAN_POINT ( 'NONE',  ( 96.46446609406721961, 3.535533905932755072, 7.000000002731185056 ) ) ;
#15611 = CARTESIAN_POINT ( 'NONE',  ( 104.4587341249999781, 81.25000000136560629, -1.846868145590750299 ) ) ;
#15612 = CARTESIAN_POINT ( 'NONE',  ( 55.70494972787295751, 36.08867187608393579, 9.295050272127047819 ) ) ;
#15613 = CARTESIAN_POINT ( 'NONE',  ( 102.4976396683250925, 117.6869444889999841, -51.72500000273119980 ) ) ;
#15614 = CARTESIAN_POINT ( 'NONE',  ( -9.295050272127046043, 38.86679687608393863, -9.295050272127046043 ) ) ;
#15615 = EDGE_CURVE ( 'NONE', #8262, #25975, #402, .T. ) ;
#15616 = CYLINDRICAL_SURFACE ( 'NONE', #10717, 5.000000000000000000 ) ;
#15617 = DIRECTION ( 'NONE',  ( 0.000000000000000000, 1.000000000000000000, 0.000000000000000000 ) ) ;
#15618 = CARTESIAN_POINT ( 'NONE',  ( 107.0000000000000000, 107.7255621263696668, -55.59999999453763309 ) ) ;
#15619 = CARTESIAN_POINT ( 'NONE',  ( 120.4011555911795455, 37.13046874999999147, 9.598844408820459861 ) ) ;
#15620 = ORIENTED_EDGE ( 'NONE', *, *, #1675, .T. ) ;
#15621 = EDGE_CURVE ( 'NONE', #17097, #12117, #14258, .T. ) ;
#15622 = VERTEX_POINT ( 'NONE', #20637 ) ;
#15623 = CARTESIAN_POINT ( 'NONE',  ( 99.99999999999995737, -4.999999999999990230, 8.250000000000000000 ) ) ;
#15624 = CARTESIAN_POINT ( 'NONE',  ( -13.14518615778179189, 36.83281250108393579, 5.444914386472304635 ) ) ;
#15625 = CARTESIAN_POINT ( 'NONE',  ( 5.622872871577871301, 38.46992187716787015, -13.57481594606304753 ) ) ;
#15626 =( BOUNDED_CURVE ( )  B_SPLINE_CURVE ( 2, ( #27565, #21008, #23006, #10430, #19139, #27844, #12142, #16989, #7885 ),
 .UNSPECIFIED., .F., .F. ) 
 B_SPLINE_CURVE_WITH_KNOTS ( ( 3, 2, 2, 2, 3 ),
 ( 0.5357142857142856984, 0.5446428571428570953, 0.5535714285714286031, 0.5625000000000000000, 0.5714285714285713969 ),
 .UNSPECIFIED. ) 
 CURVE ( )  GEOMETRIC_REPRESENTATION_ITEM ( )  RATIONAL_B_SPLINE_CURVE ( ( 1.000000000000000000, 0.9238795325112867385, 1.000000000000000000, 0.9238795325112867385, 1.000000000000000000, 0.9238795325112867385, 1.000000000000000000, 0.9238795325112867385, 1.000000000000000000 ) ) 
 REPRESENTATION_ITEM ( '' )  );
#15627 = CARTESIAN_POINT ( 'NONE',  ( 103.5355339059327093, 3.535533905932755072, 9.750000002731184168 ) ) ;
#15628 = CARTESIAN_POINT ( 'NONE',  ( 124.5550856135277087, 34.35234375108392868, 13.14518615778179722 ) ) ;
#15629 = CARTESIAN_POINT ( 'NONE',  ( 78.57481594606304043, 34.40195312716787157, -5.622872871577873077 ) ) ;
#15630 = ORIENTED_EDGE ( 'NONE', *, *, #23425, .T. ) ;
#15631 = CARTESIAN_POINT ( 'NONE',  ( 104.9999999999999716, 83.56250000000002842, -2.071067811865491937 ) ) ;
#15632 = CARTESIAN_POINT ( 'NONE',  ( 5.622872871577871301, 32.91367187716787157, -13.57481594606304753 ) ) ;
#15633 = CARTESIAN_POINT ( 'NONE',  ( 101.7677669529663547, 123.8000000021849587, 1.767766952966350891 ) ) ;
#15634 = AXIS2_PLACEMENT_3D ( 'NONE', #22491, #13630, #2956 ) ;
#15635 = CARTESIAN_POINT ( 'NONE',  ( 91.91746824999997045, 107.3738262389971680, -49.77499999726881441 ) ) ;
#15636 = CARTESIAN_POINT ( 'NONE',  ( 9.598844408820459861, 39.80937500216786873, 9.598844408820456309 ) ) ;
#15637 = CARTESIAN_POINT ( 'NONE',  ( 200.4449143864723055, 34.45156250108393436, 13.14518615778179189 ) ) ;
#15638 = CARTESIAN_POINT ( 'NONE',  ( 94.99999999999995737, 1.387778780781445676E-14, 6.125000002731185056 ) ) ;
#15639 = CARTESIAN_POINT ( 'NONE',  ( 203.2014461876500775, 50.69246985422139318, 14.99999999999785416 ) ) ;
#15640 =( LENGTH_UNIT ( ) NAMED_UNIT ( * ) SI_UNIT ( .MILLI., .METRE. ) );
#15641 = CYLINDRICAL_SURFACE ( 'NONE', #10955, 13.57481594606304398 ) ;
#15642 = CARTESIAN_POINT ( 'NONE',  ( 214.9999999999999716, 55.00000000000000000, 9.999999999999946709 ) ) ;
#15643 = CARTESIAN_POINT ( 'NONE',  ( 105.6631189606246295, 105.8855032339526758, -47.69999999453764161 ) ) ;
#15644 = CARTESIAN_POINT ( 'NONE',  ( -9.598844408820454532, 38.71796874999999716, 9.598844408820459861 ) ) ;
#15645 = CARTESIAN_POINT ( 'NONE',  ( 93.00000000000000000, 110.0000000000000000, -54.00000000000000711 ) ) ;
#15646 = CARTESIAN_POINT ( 'NONE',  ( -8.049105076161786076E-16, 34.20351562608394147, -13.14518615778179544 ) ) ;
#15647 = CARTESIAN_POINT ( 'NONE',  ( -8.049105076161786076E-16, 37.18007812608393436, -13.14518615778179544 ) ) ;
#15648 = CARTESIAN_POINT ( 'NONE',  ( 195.0000000000000000, 34.45156249999999432, -13.57481594606304576 ) ) ;
#15649 = CARTESIAN_POINT ( 'NONE',  ( 93.46109445667491400, 114.7507929638356785, -47.57500000273119412 ) ) ;
#15650 = CARTESIAN_POINT ( 'NONE',  ( 101.8468681455906903, -4.458734124999987891, 1.000000001365592528 ) ) ;
#15651 = CARTESIAN_POINT ( 'NONE',  ( 55.70494972787295751, 34.89804687608393152, -9.295050272127046043 ) ) ;
#15652 = CARTESIAN_POINT ( 'NONE',  ( 99.99999999999995737, 4.458734125000016313, 2.187500001365592084 ) ) ;
#15653 = CARTESIAN_POINT ( 'NONE',  ( 101.5239092622869492, 123.0000000000000284, -1.987527404725653035 ) ) ;
#15654 = CARTESIAN_POINT ( 'NONE',  ( 99.99999999999998579, 90.00000000000000000, -4.999999999999996447 ) ) ;
#15655 = CARTESIAN_POINT ( 'NONE',  ( 2.493653234604083739E-15, 37.22968749999999716, 13.57481594606304576 ) ) ;
#15656 = CARTESIAN_POINT ( 'NONE',  ( 116.8548138422182063, 39.11484375108394573, -5.444914386472297529 ) ) ;
#15657 = EDGE_CURVE ( 'NONE', #18860, #20976, #14334, .T. ) ;
#15658 = ORIENTED_EDGE ( 'NONE', *, *, #24079, .T. ) ;
#15659 = LINE ( 'NONE', #18084, #26390 ) ;
#15660 = CARTESIAN_POINT ( 'NONE',  ( 5.622872871577878406, 34.89804687499999147, 13.57481594606304398 ) ) ;
#15661 = CARTESIAN_POINT ( 'NONE',  ( 94.99999999999995737, 81.12500000273119838, -1.387778780781445676E-14 ) ) ;
#15662 = CARTESIAN_POINT ( 'NONE',  ( 103.1528011352953484, 92.18749999863440792, 3.152801135295352886 ) ) ;
#15663 = CARTESIAN_POINT ( 'NONE',  ( 5.622872871577786924, 34.10429687500000284, 13.57481594606313813 ) ) ;
#15664 = AXIS2_PLACEMENT_3D ( 'NONE', #6269, #25522, #5867 ) ;
#15665 = CARTESIAN_POINT ( 'NONE',  ( 107.0000000000000000, 110.0000000000000000, -50.00000000000000711 ) ) ;
#15666 = CARTESIAN_POINT ( 'NONE',  ( 65.00000000000000000, 39.61093749999999147, 13.57481594606304576 ) ) ;
#15667 = EDGE_LOOP ( 'NONE', ( #6855, #9939, #18777, #21211 ) ) ;
#15668 = DIRECTION ( 'NONE',  ( -1.000000000000000000, 0.000000000000000000, 0.000000000000000000 ) ) ;
#15669 = CARTESIAN_POINT ( 'NONE',  ( 94.99999999999995737, -2.071067811865466624, 14.06249999999999645 ) ) ;
#15670 = ORIENTED_EDGE ( 'NONE', *, *, #3745, .T. ) ;
#15671 =( BOUNDED_CURVE ( )  B_SPLINE_CURVE ( 2, ( #23391, #21112, #26081, #1876, #15085, #21674, #3864, #12673, #6141 ),
 .UNSPECIFIED., .F., .T. ) 
 B_SPLINE_CURVE_WITH_KNOTS ( ( 3, 2, 2, 2, 3 ),
 ( 0.7291666666666668517, 0.7395833333333334814, 0.7500000000000001110, 0.7604166666666667407, 0.7708333333333333703 ),
 .UNSPECIFIED. ) 
 CURVE ( )  GEOMETRIC_REPRESENTATION_ITEM ( )  RATIONAL_B_SPLINE_CURVE ( ( 0.9999999999999983347, 0.9238795325112884038, 1.000000000000000000, 0.9238795325112867385, 1.000000000000000000, 0.9238795325112867385, 1.000000000000000000, 0.9238795325112867385, 1.000000000000000000 ) ) 
 REPRESENTATION_ITEM ( '' )  );
#15672 = CARTESIAN_POINT ( 'NONE',  ( -9.295050272127046043, 37.47773437608393010, -9.295050272127046043 ) ) ;
#15673 = CARTESIAN_POINT ( 'NONE',  ( 185.4011555911795313, 34.65000000216787868, -9.598844408820458085 ) ) ;
#15674 = CARTESIAN_POINT ( 'NONE',  ( 13.14518615778179722, 32.16953125108393152, 5.444914386472293977 ) ) ;
#15675 = DIRECTION ( 'NONE',  ( 5.782411586589358625E-17, -0.000000000000000000, 1.000000000000000000 ) ) ;
#15676 = CARTESIAN_POINT ( 'NONE',  ( 130.0000000000000000, 37.37851562608393863, -13.14518615778179544 ) ) ;
#15677 = ORIENTED_EDGE ( 'NONE', *, *, #14871, .F. ) ;
#15678 = CARTESIAN_POINT ( 'NONE',  ( 9.295050272127047819, 36.28710937608393294, 9.295050272127046043 ) ) ;
#15679 = CARTESIAN_POINT ( 'NONE',  ( 124.5550856135277087, 31.97109375108393436, 13.14518615778179722 ) ) ;
#15680 = CARTESIAN_POINT ( 'NONE',  ( 55.40115559117954547, 33.95546874999999432, 9.598844408820459861 ) ) ;
#15681 = CARTESIAN_POINT ( 'NONE',  ( 100.8561741729129295, 124.2000000010924907, 2.066987299999979211 ) ) ;
#15682 = CARTESIAN_POINT ( 'NONE',  ( 95.54126587499995082, 1.846868145590750077, 9.625000001365593860 ) ) ;
#15683 = PLANE ( 'NONE',  #26733 ) ;
#15684 = CARTESIAN_POINT ( 'NONE',  ( 98.15313185440925281, 4.458734125000016313, 1.250000001365592750 ) ) ;
#15685 = CARTESIAN_POINT ( 'NONE',  ( 95.00472066334982912, 103.1245878333314323, -46.82500000273118701 ) ) ;
#15686 = PLANE ( 'NONE',  #26367 ) ;
#15687 = CARTESIAN_POINT ( 'NONE',  ( 65.00000000000000000, 37.22968749999999716, 13.57481594606304576 ) ) ;
#15688 = CARTESIAN_POINT ( 'NONE',  ( 95.00472066334981491, 116.8754121666685393, -49.92499999726880588 ) ) ;
#15689 = CARTESIAN_POINT ( 'NONE',  ( 13.14518615778179900, 36.33671875108394289, 5.444914386472293977 ) ) ;
#15690 = CARTESIAN_POINT ( 'NONE',  ( 105.6631189606246153, 114.1144967660473242, -47.29999999453764303 ) ) ;
#15691 = EDGE_LOOP ( 'NONE', ( #5138, #1734, #12355, #263 ) ) ;
#15692 = DIRECTION ( 'NONE',  ( 0.000000000000000000, 0.000000000000000000, -1.000000000000000000 ) ) ;
#15693 = CARTESIAN_POINT ( 'NONE',  ( 99.14382582708708469, 122.8000000010924708, -2.066987299999998751 ) ) ;
#15694 = DIRECTION ( 'NONE',  ( -1.000000000000000000, -1.203706215242021094E-31, 3.469446951953613696E-16 ) ) ;
#15695 = CARTESIAN_POINT ( 'NONE',  ( 208.1451861577817795, 34.65000000108393152, -5.444914386472297529 ) ) ;
#15696 = ORIENTED_EDGE ( 'NONE', *, *, #2053, .T. ) ;
#15697 = CARTESIAN_POINT ( 'NONE',  ( 198.1165920804657503, 53.90895096933309105, -15.00000000000000178 ) ) ;
#15698 = CARTESIAN_POINT ( 'NONE',  ( 96.84719886470459471, -3.152801135295355994, 10.81250000136559208 ) ) ;
#15699 = ADVANCED_FACE ( 'NONE', ( #9508 ), #18769, .T. ) ;
#15700 = ORIENTED_EDGE ( 'NONE', *, *, #16294, .F. ) ;
#15701 = CARTESIAN_POINT ( 'NONE',  ( 102.1631189606246295, 103.3426043859339103, -47.40000000000000568 ) ) ;
#15702 = VECTOR ( 'NONE', #21375, 1000.000000000000000 ) ;
#15703 = CARTESIAN_POINT ( 'NONE',  ( -13.14518615778179900, 38.12265625108393152, -5.444914386472297529 ) ) ;
#15704 = CARTESIAN_POINT ( 'NONE',  ( 101.0355339059327378, 124.7500000000000142, -2.499999999999997780 ) ) ;
#15705 = CARTESIAN_POINT ( 'NONE',  ( 116.4251840539369596, 32.41757812716787157, 5.622872871577880183 ) ) ;
#15706 = DIRECTION ( 'NONE',  ( 0.000000000000000000, 1.000000000000000000, -1.156482317317871478E-16 ) ) ;
#15707 = CARTESIAN_POINT ( 'NONE',  ( 97.92893218813452449, 94.18749999726880162, -4.999999999999997335 ) ) ;
#15708 = CARTESIAN_POINT ( 'NONE',  ( 51.85481384221819923, 37.52734375108393294, -5.444914386472297529 ) ) ;
#15709 = CARTESIAN_POINT ( 'NONE',  ( 71.16106217484892227, 51.27996893916711940, -15.00000000000068390 ) ) ;
#15710 = CARTESIAN_POINT ( 'NONE',  ( 93.46109445667491400, 114.7507929638356785, -51.57500000273120122 ) ) ;
#15711 = CARTESIAN_POINT ( 'NONE',  ( 208.1451861577817795, 32.36796875108393579, 5.444914386472293977 ) ) ;
#15712 = CARTESIAN_POINT ( 'NONE',  ( 66.13716782454086740, 35.99999999999998579, 13.09590655363602707 ) ) ;
#15713 = EDGE_LOOP ( 'NONE', ( #12665, #8805, #24437, #21073 ) ) ;
#15714 = CARTESIAN_POINT ( 'NONE',  ( 2.414731522848535132E-15, 34.60039062608393579, 13.14518615778179544 ) ) ;
#15715 = CARTESIAN_POINT ( 'NONE',  ( 101.8468681455907046, -4.458734124999987891, 11.00000000136559208 ) ) ;
#15716 = CARTESIAN_POINT ( 'NONE',  ( 78.14518615778179367, 36.18789062608393436, -1.609821015232357215E-15 ) ) ;
#15717 = PLANE ( 'NONE',  #26076 ) ;
#15718 = CARTESIAN_POINT ( 'NONE',  ( 97.92893218813451028, -4.999999999999989342, 2.187499999999999112 ) ) ;
#15719 = VERTEX_POINT ( 'NONE', #9790 ) ;
#15720 = CARTESIAN_POINT ( 'NONE',  ( -9.295050272127046043, 39.06523437608392868, -9.295050272127046043 ) ) ;
#15721 = CIRCLE ( 'NONE', #7073, 0.5000000000000086597 ) ;
#15722 = CARTESIAN_POINT ( 'NONE',  ( 99.99999999999998579, 90.81249999863440792, -4.458734124999994997 ) ) ;
#15723 = CARTESIAN_POINT ( 'NONE',  ( 181.8548138422182205, 37.57695312608393579, 0.000000000000000000 ) ) ;
#15724 = CARTESIAN_POINT ( 'NONE',  ( 91.91746824999997045, 112.6261737610028320, -45.97499999726882436 ) ) ;
#15725 = VERTEX_POINT ( 'NONE', #15908 ) ;
#15726 = CARTESIAN_POINT ( 'NONE',  ( 13.57481594606304576, 32.66562499999999858, -1.662435489736055892E-15 ) ) ;
#15727 = CARTESIAN_POINT ( 'NONE',  ( 2.414731522848535132E-15, 35.19570312608392726, 13.14518615778179544 ) ) ;
#15728 = VECTOR ( 'NONE', #10802, 1000.000000000000000 ) ;
#15729 = ORIENTED_EDGE ( 'NONE', *, *, #14283, .T. ) ;
#15730 = CARTESIAN_POINT ( 'NONE',  ( 116.8548138422182063, 34.45156250108394147, 5.444914386472304635 ) ) ;
#15731 = CARTESIAN_POINT ( 'NONE',  ( 65.00000000000000000, 40.55351562608393579, -13.14518615778179544 ) ) ;
#15732 = CARTESIAN_POINT ( 'NONE',  ( 181.8548138422182205, 32.81445312608393294, 0.000000000000000000 ) ) ;
#15733 = VERTEX_POINT ( 'NONE', #18497 ) ;
#15734 = CARTESIAN_POINT ( 'NONE',  ( 102.0669873000000081, 124.2000000010924623, -0.8561741729129508371 ) ) ;
#15735 = CARTESIAN_POINT ( 'NONE',  ( 5.444914386472297529, 33.16171875108393152, -13.14518615778179900 ) ) ;
#15736 = DIRECTION ( 'NONE',  ( -0.8660254037844407060, 0.4999999999999963363, 0.000000000000000000 ) ) ;
#15737 = EDGE_CURVE ( 'NONE', #8402, #26359, #25181, .T. ) ;
#15738 = CARTESIAN_POINT ( 'NONE',  ( 2.129810658427479630, 36.02027164734404607, -13.57481594606306352 ) ) ;
#15739 = CARTESIAN_POINT ( 'NONE',  ( 195.0000000000000000, 40.40468749999999432, 13.57481594606304576 ) ) ;
#15740 = ADVANCED_FACE ( 'NONE', ( #27204 ), #16263, .T. ) ;
#15741 = CARTESIAN_POINT ( 'NONE',  ( -5.622872871577782483, 34.60039062716787583, -13.57481594606313990 ) ) ;
#15742 = CARTESIAN_POINT ( 'NONE',  ( 73.25961152888550032, 50.00000000056312643, 10.79618466886052630 ) ) ;
#15743 = EDGE_LOOP ( 'NONE', ( #10670, #15948, #10043, #8549 ) ) ;
#15744 = CARTESIAN_POINT ( 'NONE',  ( 99.99999999999995737, 4.458734125000016313, 4.187500001365592084 ) ) ;
#15745 = VECTOR ( 'NONE', #1930, 1000.000000000000000 ) ;
#15746 = EDGE_LOOP ( 'NONE', ( #8316, #24570, #16040, #16024 ) ) ;
#15747 = CARTESIAN_POINT ( 'NONE',  ( 97.93301270000000613, 124.5500000010924850, -9.540979117872439019E-15 ) ) ;
#15748 = CARTESIAN_POINT ( 'NONE',  ( 95.54126587499995082, -1.846868145590724986, 9.500000001365593860 ) ) ;
#15749 = CARTESIAN_POINT ( 'NONE',  ( 137.0894172723430415, 49.99999999943648987, 11.59823041028222157 ) ) ;
#15750 = EDGE_CURVE ( 'NONE', #13180, #11544, #2616, .T. ) ;
#15751 = CARTESIAN_POINT ( 'NONE',  ( 9.295050272127046043, 35.49335937608393010, -9.295050272127046043 ) ) ;
#15752 = CARTESIAN_POINT ( 'NONE',  ( 94.99999999999995737, 1.387778780781445676E-14, 7.125000002731185056 ) ) ;
#15753 = CARTESIAN_POINT ( 'NONE',  ( 214.9999999999999716, 55.00000000000000000, -15.00000000000000000 ) ) ;
#15754 = CARTESIAN_POINT ( 'NONE',  ( 59.55508561352770158, 35.04687500108393294, -13.14518615778179900 ) ) ;
#15755 = CARTESIAN_POINT ( 'NONE',  ( 106.5389055433251002, 114.7507929638356785, -45.92500000273119554 ) ) ;
#15756 = CARTESIAN_POINT ( 'NONE',  ( 13.14518615778179722, 37.03125000108393294, -5.444914386472297529 ) ) ;
#15757 = CARTESIAN_POINT ( 'NONE',  ( 105.6631189606246295, 114.1144967660473242, -49.30000000546237970 ) ) ;
#15758 = CARTESIAN_POINT ( 'NONE',  ( -1.602533130612661116, 53.60343507248209960, 15.00000000000000000 ) ) ;
#15759 = CARTESIAN_POINT ( 'NONE',  ( 93.00000000000001421, 112.2744378736303617, -49.10000000000000142 ) ) ;
#15760 = CARTESIAN_POINT ( 'NONE',  ( 120.4011555911795455, 38.71796874999999716, 9.598844408820459861 ) ) ;
#15761 = ORIENTED_EDGE ( 'NONE', *, *, #2230, .T. ) ;
#15762 = CARTESIAN_POINT ( 'NONE',  ( 65.00000000000000000, -7.395377635281828788, 13.57481594606303688 ) ) ;
#15763 = CARTESIAN_POINT ( 'NONE',  ( -9.295050272127046043, 32.71523437608393436, -9.295050272127046043 ) ) ;
#15764 = CARTESIAN_POINT ( 'NONE',  ( 13.57481594606304931, 35.09648437716787583, 5.622872871577869525 ) ) ;
#15765 = CARTESIAN_POINT ( 'NONE',  ( 104.9999999999999574, -2.071067811865462627, 11.56250000273118772 ) ) ;
#15766 = CARTESIAN_POINT ( 'NONE',  ( 130.0000000000000000, 32.81445312608393294, 13.14518615778179544 ) ) ;
#15767 = CARTESIAN_POINT ( 'NONE',  ( 51.42518405393695957, 33.90585937716787868, -5.622872871577873077 ) ) ;
#15768 = ADVANCED_FACE ( 'NONE', ( #14241 ), #27514, .F. ) ;
#15769 = CARTESIAN_POINT ( 'NONE',  ( 100.0000000000000000, 110.0000000000000000, -55.00000000000000711 ) ) ;
#15770 = CARTESIAN_POINT ( 'NONE',  ( -13.57481594606304576, 31.57421875216786944, 0.000000000000000000 ) ) ;
#15771 = AXIS2_PLACEMENT_3D ( 'NONE', #908, #15450, #9862 ) ;
#15772 = CARTESIAN_POINT ( 'NONE',  ( 103.5355339059327093, -3.535533905932726206, 1.374999999999999556 ) ) ;
#15773 = DIRECTION ( 'NONE',  ( -1.000000000000000000, 0.000000000000000000, 7.228014483236696740E-18 ) ) ;
#15774 = CARTESIAN_POINT ( 'NONE',  ( 13.57481594606304931, 39.85898437716787157, 5.622872871577869525 ) ) ;
#15775 = CARTESIAN_POINT ( 'NONE',  ( 189.5550856135277229, 34.35234375108392868, 13.14518615778179722 ) ) ;
#15776 = DIRECTION ( 'NONE',  ( 0.000000000000000000, 0.000000000000000000, 1.000000000000000000 ) ) ;
#15777 = CARTESIAN_POINT ( 'NONE',  ( 102.4999999999999716, 124.6569999999781544, -1.035533905932742638 ) ) ;
#15778 = EDGE_CURVE ( 'NONE', #12289, #12988, #28083, .T. ) ;
#15779 = FILL_AREA_STYLE_COLOUR ( '', #15009 ) ;
#15780 = DIRECTION ( 'NONE',  ( -0.000000000000000000, -1.000000000000000000, -0.000000000000000000 ) ) ;
#15781 = CARTESIAN_POINT ( 'NONE',  ( 120.4011555911795455, 36.43593750216787441, 9.598844408820459861 ) ) ;
#15782 = CYLINDRICAL_SURFACE ( 'NONE', #22426, 5.000000000000004441 ) ;
#15783 = CARTESIAN_POINT ( 'NONE',  ( -5.622872871577873077, 35.29492187500000000, -13.57481594606304753 ) ) ;
#15784 =( BOUNDED_CURVE ( )  B_SPLINE_CURVE ( 2, ( #22464, #11599, #20322, #20609, #2929, #1093, #9760, #18470, #27178 ),
 .UNSPECIFIED., .F., .T. ) 
 B_SPLINE_CURVE_WITH_KNOTS ( ( 3, 2, 2, 2, 3 ),
 ( 0.07142857142857149400, 0.08035714285714290472, 0.08928571428571430157, 0.09821428571428571230, 0.1071428571428571092 ),
 .UNSPECIFIED. ) 
 CURVE ( )  GEOMETRIC_REPRESENTATION_ITEM ( )  RATIONAL_B_SPLINE_CURVE ( ( 0.9999999999999994449, 0.9238795325112872936, 1.000000000000000000, 0.9238795325112867385, 1.000000000000000000, 0.9238795325112867385, 1.000000000000000000, 0.9238795325112869605, 0.9999999999999997780 ) ) 
 REPRESENTATION_ITEM ( '' )  );
#15785 = CARTESIAN_POINT ( 'NONE',  ( 105.6631189606246295, 114.1144967660473242, -54.80000000000001137 ) ) ;
#15786 = VECTOR ( 'NONE', #12141, 1000.000000000000000 ) ;
#15787 = CARTESIAN_POINT ( 'NONE',  ( 5.444914386472297529, 35.74140625108393721, -13.14518615778179900 ) ) ;
#15788 = CARTESIAN_POINT ( 'NONE',  ( 5.444914386472297529, 34.74921875108394431, -13.14518615778179900 ) ) ;
#15789 = CARTESIAN_POINT ( 'NONE',  ( -9.295050272127046043, 35.69179687608393436, -9.295050272127046043 ) ) ;
#15790 = CARTESIAN_POINT ( 'NONE',  ( -13.57481594606304576, 36.38632812716788578, 5.622872871577880183 ) ) ;
#15791 = CARTESIAN_POINT ( 'NONE',  ( 96.46446609406721961, -3.535533905932727539, 4.250000002731185056 ) ) ;
#15792 = CARTESIAN_POINT ( 'NONE',  ( 95.54126587499996504, 84.43750000136560629, -1.387778780781445676E-14 ) ) ;
#15793 = CARTESIAN_POINT ( 'NONE',  ( 78.14518615778179367, 34.60039062608392868, -1.609821015232357215E-15 ) ) ;
#15794 = CARTESIAN_POINT ( 'NONE',  ( 95.00472066334982912, 103.1245878333314323, -53.07500000273118701 ) ) ;
#15795 = CARTESIAN_POINT ( 'NONE',  ( 97.90609941151407725, 123.0000000000000000, 1.374260159723026176 ) ) ;
#15796 = CARTESIAN_POINT ( 'NONE',  ( 100.8561741729129295, 123.2000000010924765, 2.066987299999979211 ) ) ;
#15797 = CARTESIAN_POINT ( 'NONE',  ( 13.57481594606304753, 33.50898437499999716, -5.622872871577873077 ) ) ;
#15798 = CARTESIAN_POINT ( 'NONE',  ( 120.7049497278729575, 38.46992187608393721, 9.295050272127047819 ) ) ;
#15799 = ORIENTED_EDGE ( 'NONE', *, *, #19418, .T. ) ;
#15800 = DIRECTION ( 'NONE',  ( 5.782411586589358625E-17, -0.000000000000000000, 1.000000000000000000 ) ) ;
#15801 = CARTESIAN_POINT ( 'NONE',  ( 99.99999999999998579, 129.0000000000000000, -12.50000000000002132 ) ) ;
#15802 = CARTESIAN_POINT ( 'NONE',  ( 104.9999999999999716, 81.62500000273119838, -1.449011120738813565E-14 ) ) ;
#15803 = CARTESIAN_POINT ( 'NONE',  ( 97.92893218813452449, 91.31250000000001421, -4.999999999999997335 ) ) ;
#15804 = CARTESIAN_POINT ( 'NONE',  ( 68.62861429328485485, 35.99999999999999289, -13.08307257738123575 ) ) ;
#15805 = CARTESIAN_POINT ( 'NONE',  ( 93.46109445667489979, 105.2492070361643215, -49.42499999726882010 ) ) ;
#15806 = CARTESIAN_POINT ( 'NONE',  ( 70.62287287157788285, 40.45429687500001137, 13.57481594606304576 ) ) ;
#15807 = ADVANCED_BREP_SHAPE_REPRESENTATION ( '', ( #17477, #26844 ), #9975 ) ;
#15808 = EDGE_LOOP ( 'NONE', ( #19167, #18839, #24940, #22596, #13854, #26372 ) ) ;
#15809 = AXIS2_PLACEMENT_3D ( 'NONE', #27404, #22848, #10260 ) ;
#15810 = CARTESIAN_POINT ( 'NONE',  ( 99.99999999999998579, 95.12499999726881583, -4.999999999999997335 ) ) ;
#15811 = CARTESIAN_POINT ( 'NONE',  ( 97.92893218813451028, 5.000000000000018652, 11.81249999999999822 ) ) ;
#15812 = VERTEX_POINT ( 'NONE', #5576 ) ;
#15813 = CARTESIAN_POINT ( 'NONE',  ( -13.14518615778179900, 37.52734375108393294, -5.444914386472297529 ) ) ;
#15814 = CARTESIAN_POINT ( 'NONE',  ( 181.4251840539369596, 35.54296875216788010, 0.000000000000000000 ) ) ;
#15815 = CARTESIAN_POINT ( 'NONE',  ( 2.414731522848535132E-15, 34.40195312608393152, 13.14518615778179544 ) ) ;
#15816 = CARTESIAN_POINT ( 'NONE',  ( 207.0772764098356049, 36.00000000000000711, -6.197985357349214297 ) ) ;
#15817 = CARTESIAN_POINT ( 'NONE',  ( 208.5748159460630688, 38.32109375216786873, -1.662435489736055892E-15 ) ) ;
#15818 = CARTESIAN_POINT ( 'NONE',  ( 13.14518615778179544, 34.00507812608393721, -1.609821015232357215E-15 ) ) ;
#15819 = CARTESIAN_POINT ( 'NONE',  ( 120.7049497278729575, 31.72304687608393081, -9.295050272127046043 ) ) ;
#15820 = CARTESIAN_POINT ( 'NONE',  ( 98.15313185440923860, 90.99999999863439371, 4.458734124999980786 ) ) ;
#15821 = CARTESIAN_POINT ( 'NONE',  ( 214.9999999999999716, 75.00000000000000000, -15.00000000000000000 ) ) ;
#15822 = CARTESIAN_POINT ( 'NONE',  ( 117.9434479702998431, 36.00000000000000000, 5.307619621752288630 ) ) ;
#15823 = CARTESIAN_POINT ( 'NONE',  ( 95.54126587499995082, -1.846868145590724986, 12.75000000136559386 ) ) ;
#15824 = CARTESIAN_POINT ( 'NONE',  ( 0.000000000000000000, 50.00000000000000000, 0.000000000000000000 ) ) ;
#15825 = CARTESIAN_POINT ( 'NONE',  ( 98.15313185440923860, -4.458734124999987891, 9.625000001365593860 ) ) ;
#15826 = CARTESIAN_POINT ( 'NONE',  ( 99.99999999999998579, 118.4984768113314004, -47.62500000273119127 ) ) ;
#15827 = CARTESIAN_POINT ( 'NONE',  ( 99.99999999999998579, 92.31249999863440792, 4.458734124999981674 ) ) ;
#15828 = CARTESIAN_POINT ( 'NONE',  ( 0.000000000000000000, 36.00000000000000000, 0.000000000000000000 ) ) ;
#15829 = CARTESIAN_POINT ( 'NONE',  ( 106.5389055433250860, 114.7507929638356785, -52.42499999726882010 ) ) ;
#15830 = CARTESIAN_POINT ( 'NONE',  ( 5.444914386472302859, 35.44375000108393436, 13.14518615778179189 ) ) ;
#15831 = EDGE_LOOP ( 'NONE', ( #9395, #21851 ) ) ;
#15832 = DIRECTION ( 'NONE',  ( -1.000000000000000000, 0.000000000000000000, 1.224646799147411139E-16 ) ) ;
#15833 = CARTESIAN_POINT ( 'NONE',  ( 94.99999999999995737, -2.071067811865466624, 1.062499999999999112 ) ) ;
#15834 =( BOUNDED_CURVE ( )  B_SPLINE_CURVE ( 2, ( #23033, #3505, #20479, #27184, #12166, #959, #7635, #16329, #5226 ),
 .UNSPECIFIED., .F., .F. ) 
 B_SPLINE_CURVE_WITH_KNOTS ( ( 3, 2, 2, 2, 3 ),
 ( 0.02083333333333358892, 0.03125000000000020123, 0.04166666666666681007, 0.05208333333333342585, 0.06250000000000004163 ),
 .UNSPECIFIED. ) 
 CURVE ( )  GEOMETRIC_REPRESENTATION_ITEM ( )  RATIONAL_B_SPLINE_CURVE ( ( 0.9999999999999981126, 0.9238795325112886259, 1.000000000000000000, 0.9238795325112867385, 1.000000000000000000, 0.9238795325112867385, 1.000000000000000000, 0.9238795325112864054, 1.000000000000000222 ) ) 
 REPRESENTATION_ITEM ( '' )  );
#15835 = CARTESIAN_POINT ( 'NONE',  ( 185.7049497278729575, 34.30273437608393294, 9.295050272127047819 ) ) ;
#15836 = ORIENTED_EDGE ( 'NONE', *, *, #4279, .T. ) ;
#15837 = CARTESIAN_POINT ( 'NONE',  ( 217.9999999999999716, 78.00000000000000000, 12.99999999999994316 ) ) ;
#15838 = CARTESIAN_POINT ( 'NONE',  ( 104.4587341249999639, 1.442382525525748735E-14, 12.18750000136559208 ) ) ;
#15839 = ORIENTED_EDGE ( 'NONE', *, *, #19768, .T. ) ;
#15840 = CARTESIAN_POINT ( 'NONE',  ( 95.00472066334982912, 103.1245878333314323, -53.07500000273118701 ) ) ;
#15841 = CARTESIAN_POINT ( 'NONE',  ( 5.444914386472302859, 35.24531250108393010, 13.14518615778179189 ) ) ;
#15842 = CARTESIAN_POINT ( 'NONE',  ( 96.46446609406721961, 79.25000000273118417, 3.535533905932727539 ) ) ;
#15843 = CIRCLE ( 'NONE', #18593, 13.57481594606304398 ) ;
#15844 = CARTESIAN_POINT ( 'NONE',  ( 116.8548138422182063, 36.53515625108392584, -5.444914386472297529 ) ) ;
#15845 = CARTESIAN_POINT ( 'NONE',  ( 94.99999999999995737, 1.387778780781445676E-14, 11.12500000273118594 ) ) ;
#15846 = CARTESIAN_POINT ( 'NONE',  ( 9.295050272127047819, 35.29492187608393294, 9.295050272127046043 ) ) ;
#15847 = AXIS2_PLACEMENT_3D ( 'NONE', #28135, #3294, #22827 ) ;
#15848 = CARTESIAN_POINT ( 'NONE',  ( 102.0710678118654613, 95.68749999726881583, 4.999999999999983125 ) ) ;
#15849 = CARTESIAN_POINT ( 'NONE',  ( 74.29505027212704249, 37.27929687608394005, -9.295050272127046043 ) ) ;
#15850 = CARTESIAN_POINT ( 'NONE',  ( 69.92502678366200541, 49.99999999893144320, -12.67776588292042028 ) ) ;
#15851 = CARTESIAN_POINT ( 'NONE',  ( 108.0825317500000011, 112.6261737610028320, -52.27500000273118275 ) ) ;
#15852 = CARTESIAN_POINT ( 'NONE',  ( 208.1451861577817795, 33.16171875108393863, 5.444914386472293977 ) ) ;
#15853 = CYLINDRICAL_SURFACE ( 'NONE', #14833, 7.000000000000006217 ) ;
#15854 = VERTEX_POINT ( 'NONE', #12091 ) ;
#15855 = CARTESIAN_POINT ( 'NONE',  ( 5.444914386472302859, 37.03125000108393294, 13.14518615778179189 ) ) ;
#15856 = CARTESIAN_POINT ( 'NONE',  ( 103.1528011352953342, 3.152801135295383084, 8.312500001365592084 ) ) ;
#15857 = CARTESIAN_POINT ( 'NONE',  ( 59.55508561352770158, 38.81718750108393579, -13.14518615778179722 ) ) ;
#15858 = DIRECTION ( 'NONE',  ( 5.782411586589357392E-17, -0.000000000000000000, 1.000000000000000000 ) ) ;
#15859 = CARTESIAN_POINT ( 'NONE',  ( 103.5355339059327093, -3.535533905932726206, 14.37499999999999822 ) ) ;
#15860 = CARTESIAN_POINT ( 'NONE',  ( -5.444914386472299306, 34.55078125108393294, 13.14518615778179722 ) ) ;
#15861 = EDGE_CURVE ( 'NONE', #291, #10253, #27378, .T. ) ;
#15862 = CARTESIAN_POINT ( 'NONE',  ( -8.312177448680279460E-16, 34.45156249999999432, -13.57481594606304576 ) ) ;
#15863 = CARTESIAN_POINT ( 'NONE',  ( 200.4449143864723055, 38.61875000108392442, 13.14518615778179189 ) ) ;
#15864 = CARTESIAN_POINT ( 'NONE',  ( 91.91746824999998466, 110.0000000000000000, -47.87499999726882294 ) ) ;
#15865 = ORIENTED_EDGE ( 'NONE', *, *, #4617, .F. ) ;
#15866 = CARTESIAN_POINT ( 'NONE',  ( 13.57481594606304576, 34.25312499999999716, -1.662435489736055892E-15 ) ) ;
#15867 = CARTESIAN_POINT ( 'NONE',  ( 2.414731522848535132E-15, 34.40195312608393152, 13.14518615778179544 ) ) ;
#15868 = ORIENTED_EDGE ( 'NONE', *, *, #27428, .T. ) ;
#15869 = CARTESIAN_POINT ( 'NONE',  ( 143.1451861577818079, 33.16171875108393863, 5.444914386472293977 ) ) ;
#15870 = CARTESIAN_POINT ( 'NONE',  ( 181.4251840539369596, 37.08085937716787583, -5.622872871577872189 ) ) ;
#15871 = CARTESIAN_POINT ( 'NONE',  ( 189.5550856135277229, 32.96328125108393436, 13.14518615778179722 ) ) ;
#15872 = ORIENTED_EDGE ( 'NONE', *, *, #13151, .T. ) ;
#15873 = CARTESIAN_POINT ( 'NONE',  ( 98.53841926354351699, 124.4500000010924765, -1.461580736456474794 ) ) ;
#15874 = CARTESIAN_POINT ( 'NONE',  ( 4.571591632531690763, 51.44262710532315452, -14.99999999999999112 ) ) ;
#15875 = DIRECTION ( 'NONE',  ( -0.000000000000000000, 1.000000000000000000, -0.000000000000000000 ) ) ;
#15876 = CARTESIAN_POINT ( 'NONE',  ( 143.5748159460630404, 37.57695312716787583, -5.622872871577873077 ) ) ;
#15877 = CARTESIAN_POINT ( 'NONE',  ( 104.9952793366501709, 103.1245878333314465, -50.42500000273119554 ) ) ;
#15878 = CARTESIAN_POINT ( 'NONE',  ( 99.99999999999998579, 138.0000000000000000, -5.204170427930421283E-15 ) ) ;
#15879 = CYLINDRICAL_SURFACE ( 'NONE', #20989, 4.999999999999989342 ) ;
#15880 = CARTESIAN_POINT ( 'NONE',  ( 189.5550856135277229, 40.60312500108393863, -13.14518615778179900 ) ) ;
#15881 =( GEOMETRIC_REPRESENTATION_CONTEXT ( 3 ) GLOBAL_UNCERTAINTY_ASSIGNED_CONTEXT ( ( #2155 ) ) GLOBAL_UNIT_ASSIGNED_CONTEXT ( ( #19187, #16901, #27888 ) ) REPRESENTATION_CONTEXT ( 'NONE', 'WORKASPACE' ) );
#15882 = CARTESIAN_POINT ( 'NONE',  ( 96.84719886470459471, 3.152801135295383084, 4.312500001365592084 ) ) ;
#15883 = ORIENTED_EDGE ( 'NONE', *, *, #2716, .T. ) ;
#15884 = CARTESIAN_POINT ( 'NONE',  ( -0.9955612250524552564, 35.99999999999999289, -13.45766439703027118 ) ) ;
#15885 = CARTESIAN_POINT ( 'NONE',  ( 98.15313185440925281, 4.458734125000016313, 8.250000001365592084 ) ) ;
#15886 = CARTESIAN_POINT ( 'NONE',  ( 135.6228728715779255, 38.17226562716787441, 13.57481594606301023 ) ) ;
#15887 = COLOUR_RGB ( '', 0.66274510, 0.83137255, 0.94901961) ;
#15888 = CARTESIAN_POINT ( 'NONE',  ( -9.295050272127044266, 36.68398437608392726, 9.295050272127047819 ) ) ;
#15889 = DIRECTION ( 'NONE',  ( 1.000000000000000000, 0.000000000000000000, -2.385244779468110248E-16 ) ) ;
#15890 = CARTESIAN_POINT ( 'NONE',  ( 98.15313185440925281, 93.99999999863439371, 4.458734124999979898 ) ) ;
#15891 = CARTESIAN_POINT ( 'NONE',  ( 99.99999999999998579, 118.4984768113314004, -45.62500000273118417 ) ) ;
#15892 = CARTESIAN_POINT ( 'NONE',  ( -9.295050272127044266, 39.06523437608392868, 9.295050272127047819 ) ) ;
#15893 = CARTESIAN_POINT ( 'NONE',  ( 0.3969994146497132781, 51.45716825712461429, 15.00000000000033573 ) ) ;
#15894 = CARTESIAN_POINT ( 'NONE',  ( 0.000000000000000000, 36.00000000000000000, 11.57481594606304398 ) ) ;
#15895 = CARTESIAN_POINT ( 'NONE',  ( 120.4011555911795455, 35.34453124999998863, -9.598844408820458085 ) ) ;
#15896 = ORIENTED_EDGE ( 'NONE', *, *, #8116, .T. ) ;
#15897 = EDGE_CURVE ( 'NONE', #8880, #9852, #19168, .T. ) ;
#15898 = CARTESIAN_POINT ( 'NONE',  ( -9.295050272127046043, 34.30273437608393294, -9.295050272127046043 ) ) ;
#15899 = CARTESIAN_POINT ( 'NONE',  ( -13.57481594606304576, 33.21132812716787441, 5.622872871577880183 ) ) ;
#15900 = CARTESIAN_POINT ( 'NONE',  ( 94.99999999999995737, -2.071067811865466624, 9.187500002731184168 ) ) ;
#15901 = CARTESIAN_POINT ( 'NONE',  ( 139.2950502721270425, 33.70742187608393436, 9.295050272127046043 ) ) ;
#15902 = CARTESIAN_POINT ( 'NONE',  ( 70.44491438647230552, 38.71796875108393721, -13.14518615778179900 ) ) ;
#15903 = CARTESIAN_POINT ( 'NONE',  ( -8.312177448680279460E-16, 37.72578125216787726, -13.57481594606304576 ) ) ;
#15904 = CARTESIAN_POINT ( 'NONE',  ( -9.295050272127044266, 38.27148437608393294, 9.295050272127047819 ) ) ;
#15905 = CARTESIAN_POINT ( 'NONE',  ( 104.9999999999999716, 1.449011120738813565E-14, 2.499999999999998668 ) ) ;
#15906 = CARTESIAN_POINT ( 'NONE',  ( 108.0825317499999869, 112.6261737610028320, -52.77499999726883573 ) ) ;
#15907 = CARTESIAN_POINT ( 'NONE',  ( -13.57481594606304576, 40.30546875216787583, 0.000000000000000000 ) ) ;
#15908 = CARTESIAN_POINT ( 'NONE',  ( -2.655063156357168549E-15, 10.00000000000000000, -19.22649730810373470 ) ) ;
#15909 = CARTESIAN_POINT ( 'NONE',  ( 97.92893218813451028, 5.000000000000018652, 5.937500002731185056 ) ) ;
#15910 = CARTESIAN_POINT ( 'NONE',  ( 97.50000000000000000, 124.2069999999781515, -9.540979117872439019E-15 ) ) ;
#15911 = AXIS2_PLACEMENT_3D ( 'NONE', #21033, #12443, #10170 ) ;
#15912 = CARTESIAN_POINT ( 'NONE',  ( -13.57481594606304576, 40.30546875216787583, 0.000000000000000000 ) ) ;
#15914 = EDGE_LOOP ( 'NONE', ( #13861, #15301, #12249, #1901 ) ) ;
#15913 = LINE ( 'NONE', #13634, #26447 ) ;
#15915 = EDGE_CURVE ( 'NONE', #19327, #24259, #19518, .T. ) ;
#15916 = DIRECTION ( 'NONE',  ( 0.000000000000000000, 0.000000000000000000, -1.000000000000000000 ) ) ;
#15917 = LINE ( 'NONE', #22644, #20146 ) ;
#15918 = CARTESIAN_POINT ( 'NONE',  ( 2.493653234604083739E-15, 33.26093749999999716, 13.57481594606304576 ) ) ;
#15919 = CARTESIAN_POINT ( 'NONE',  ( 102.1631189606246153, 116.6573956140660897, -45.60000000000001563 ) ) ;
#15920 = CARTESIAN_POINT ( 'NONE',  ( -13.14518615778179189, 35.24531250108393721, 5.444914386472304635 ) ) ;
#15921 = CARTESIAN_POINT ( 'NONE',  ( -8.049105076161786076E-16, 36.38632812608393152, -13.14518615778179544 ) ) ;
#15922 = CARTESIAN_POINT ( 'NONE',  ( 200.6228728715778686, 32.51679687499999716, 13.57481594606304576 ) ) ;
#15923 = CARTESIAN_POINT ( 'NONE',  ( -9.598844408820458085, 35.44375000216787441, -9.598844408820458085 ) ) ;
#15924 = CARTESIAN_POINT ( 'NONE',  ( 9.598844408820459861, 36.53515624999999289, 9.598844408820456309 ) ) ;
#15925 = CARTESIAN_POINT ( 'NONE',  ( 98.15313185440925281, 82.62500000136560629, 4.458734124999987891 ) ) ;
#15926 = CARTESIAN_POINT ( 'NONE',  ( 59.55508561352770158, 31.67343750108393863, -13.14518615778179900 ) ) ;
#15927 = CARTESIAN_POINT ( 'NONE',  ( 95.00000000000000000, 90.50000000000000000, -7.551217303480904118E-15 ) ) ;
#15928 = CARTESIAN_POINT ( 'NONE',  ( 99.67158809262824093, 122.9999999999999716, 2.482844439542343018 ) ) ;
#15929 = ORIENTED_EDGE ( 'NONE', *, *, #10025, .F. ) ;
#15930 = EDGE_CURVE ( 'NONE', #3337, #24121, #21372, .T. ) ;
#15931 = CARTESIAN_POINT ( 'NONE',  ( 99.14382582708707048, 123.1000000010924822, 2.066987299999979211 ) ) ;
#15932 = CARTESIAN_POINT ( 'NONE',  ( 5.622872871577871301, 34.40195312499999858, -13.57481594606304753 ) ) ;
#15933 = CARTESIAN_POINT ( 'NONE',  ( 130.0000000000000000, 38.96601562608393721, -13.14518615778179544 ) ) ;
#15934 = EDGE_LOOP ( 'NONE', ( #9986, #7005, #25825, #17861 ) ) ;
#15935 = CARTESIAN_POINT ( 'NONE',  ( 116.6399989480775901, 40.42949218912590936, 0.000000000000000000 ) ) ;
#15936 = VECTOR ( 'NONE', #16033, 1000.000000000000000 ) ;
#15937 = CARTESIAN_POINT ( 'NONE',  ( 96.46446609406726225, 94.37500000000000000, -3.535533905932738197 ) ) ;
#15938 = CARTESIAN_POINT ( 'NONE',  ( 102.0710678118654329, 79.81250000273119838, -5.000000000000018652 ) ) ;
#15939 = CARTESIAN_POINT ( 'NONE',  ( 104.9999999999999858, 94.00000000000000000, -6.938893903907228378E-15 ) ) ;
#15940 = CARTESIAN_POINT ( 'NONE',  ( 74.59884440882045453, 40.00781250216787299, -9.598844408820458085 ) ) ;
#15941 = ADVANCED_FACE ( 'NONE', ( #10651 ), #12500, .F. ) ;
#15942 = CARTESIAN_POINT ( 'NONE',  ( 91.91746824999997045, 107.3738262389971538, -47.52499999726881441 ) ) ;
#15943 = CARTESIAN_POINT ( 'NONE',  ( 55.40115559117954547, 40.10703124999999147, -9.598844408820458085 ) ) ;
#15944 = ORIENTED_EDGE ( 'NONE', *, *, #27136, .T. ) ;
#15945 = CARTESIAN_POINT ( 'NONE',  ( 186.3308878946625100, 36.00000000000000000, -10.16963847934286314 ) ) ;
#15946 = CARTESIAN_POINT ( 'NONE',  ( 96.46446609406721961, -3.535533905932727539, 12.12500000000000000 ) ) ;
#15947 = EDGE_CURVE ( 'NONE', #4172, #5706, #23919, .T. ) ;
#15948 = ORIENTED_EDGE ( 'NONE', *, *, #973, .T. ) ;
#15949 = CARTESIAN_POINT ( 'NONE',  ( -13.14518615778179544, 35.19570312608393436, 0.000000000000000000 ) ) ;
#15950 = CARTESIAN_POINT ( 'NONE',  ( 189.3771271284221314, 34.60039062716786873, -13.57481594606304753 ) ) ;
#15951 =( BOUNDED_CURVE ( )  B_SPLINE_CURVE ( 2, ( #26393, #5015, #18112 ),
 .UNSPECIFIED., .F., .T. ) 
 B_SPLINE_CURVE_WITH_KNOTS ( ( 3, 3 ),
 ( 0.5208333333333332593, 0.5249747582430960291 ),
 .UNSPECIFIED. ) 
 CURVE ( )  GEOMETRIC_REPRESENTATION_ITEM ( )  RATIONAL_B_SPLINE_CURVE ( ( 1.000000000000000888, 0.9697362687807487003, 0.9635368518655809122 ) ) 
 REPRESENTATION_ITEM ( '' )  );
#15952 = CARTESIAN_POINT ( 'NONE',  ( 5.444914386472302859, 33.65781250108393152, 13.14518615778179189 ) ) ;
#15953 = LINE ( 'NONE', #11104, #3490 ) ;
#15954 = CARTESIAN_POINT ( 'NONE',  ( 94.99999999999995737, -2.071067811865466624, 3.062499999999999112 ) ) ;
#15955 = CARTESIAN_POINT ( 'NONE',  ( 9.295050272127047819, 35.49335937608393721, 9.295050272127046043 ) ) ;
#15956 = PLANE ( 'NONE',  #21335 ) ;
#15957 = CARTESIAN_POINT ( 'NONE',  ( 104.4587341249999923, 92.37499999863440792, -1.846868145590737198 ) ) ;
#15958 = CARTESIAN_POINT ( 'NONE',  ( 114.9999999999999858, 125.0000000000000000, 14.99999999999998934 ) ) ;
#15959 = DIRECTION ( 'NONE',  ( 1.000000000000000000, 0.000000000000000000, 0.000000000000000000 ) ) ;
#15960 = CARTESIAN_POINT ( 'NONE',  ( 195.0000000000000000, 40.10703125216787157, -13.57481594606304576 ) ) ;
#15961 = CARTESIAN_POINT ( 'NONE',  ( 101.8468681455906903, -4.458734124999987891, 8.000000001365592084 ) ) ;
#15962 = CARTESIAN_POINT ( 'NONE',  ( -5.622872871577839327, 38.07304687716787583, 13.57481594606308128 ) ) ;
#15963 = AXIS2_PLACEMENT_3D ( 'NONE', #11348, #14061, #18061 ) ;
#15964 = CARTESIAN_POINT ( 'NONE',  ( 98.15313185440923860, -4.458734124999987891, 8.625000001365592084 ) ) ;
#15965 = CARTESIAN_POINT ( 'NONE',  ( 104.9952793366501851, 116.8754121666685393, -47.82500000273119412 ) ) ;
#15966 = DIRECTION ( 'NONE',  ( -0.000000000000000000, 1.000000000000000000, -0.000000000000000000 ) ) ;
#15967 = CARTESIAN_POINT ( 'NONE',  ( 104.9999999999999716, 1.449011120738813565E-14, 34.79898987322334136 ) ) ;
#15968 = FACE_OUTER_BOUND ( 'NONE', #6270, .T. ) ;
#15969 = CARTESIAN_POINT ( 'NONE',  ( -9.295050272127046043, 34.30273437608393294, -9.295050272127046043 ) ) ;
#15970 = EDGE_LOOP ( 'NONE', ( #20840, #14424, #10622, #17430 ) ) ;
#15971 = CARTESIAN_POINT ( 'NONE',  ( 99.99999999999998579, 138.0000000000000000, -5.204170427930421283E-15 ) ) ;
#15972 = DIRECTION ( 'NONE',  ( 1.000000000000000000, 0.000000000000000000, -5.782411586589357392E-17 ) ) ;
#15973 = ADVANCED_FACE ( 'NONE', ( #10787 ), #21228, .T. ) ;
#15974 = AXIS2_PLACEMENT_3D ( 'NONE', #23777, #8806, #2549 ) ;
#15975 = CARTESIAN_POINT ( 'NONE',  ( 181.8548138422182205, 36.58476562608393579, 0.000000000000000000 ) ) ;
#15976 = ORIENTED_EDGE ( 'NONE', *, *, #24123, .T. ) ;
#15977 = CARTESIAN_POINT ( 'NONE',  ( 188.9209199794811411, 54.65154858643464308, -15.00000000000000000 ) ) ;
#15978 = CARTESIAN_POINT ( 'NONE',  ( 95.54126587499995082, 1.846868145590750077, 11.62500000136559031 ) ) ;
#15979 = ORIENTED_EDGE ( 'NONE', *, *, #17301, .F. ) ;
#15980 = CARTESIAN_POINT ( 'NONE',  ( 91.91746824999999887, 110.0000000000000000, -53.37500000273119838 ) ) ;
#15981 = CARTESIAN_POINT ( 'NONE',  ( 9.295050272127046043, 36.28710937608393294, -9.295050272127046043 ) ) ;
#15982 = CARTESIAN_POINT ( 'NONE',  ( 99.99999999999998579, 124.0000000000000000, -2.499999999999997780 ) ) ;
#15983 = CARTESIAN_POINT ( 'NONE',  ( 13.57481594606304753, 39.06523437499999574, -5.622872871577873966 ) ) ;
#15984 = CARTESIAN_POINT ( 'NONE',  ( 135.4449143864723055, 37.62656250108393863, 13.14518615778179189 ) ) ;
#15985 = CARTESIAN_POINT ( 'NONE',  ( -13.14518615778179722, 39.11484375108393863, -5.444914386472297529 ) ) ;
#15986 = CARTESIAN_POINT ( 'NONE',  ( -13.14518615778179900, 34.15390625108393863, -5.444914386472297529 ) ) ;
#15987 = CARTESIAN_POINT ( 'NONE',  ( 101.8468681455907330, 92.37499999863440792, 4.458734124999979898 ) ) ;
#15988 = CARTESIAN_POINT ( 'NONE',  ( 73.26859732838660477, 50.00000000054332361, -10.78867689284328790 ) ) ;
#15989 = CARTESIAN_POINT ( 'NONE',  ( 95.00472066334981491, 116.8754121666685393, -53.67500000273118843 ) ) ;
#15990 = CARTESIAN_POINT ( 'NONE',  ( 66.68551164908284079, 35.99999999999997868, 13.05727741351676130 ) ) ;
#15991 = ORIENTED_EDGE ( 'NONE', *, *, #18231, .F. ) ;
#15992 = CARTESIAN_POINT ( 'NONE',  ( 13.14518615778179544, 34.79882812608394005, -1.609821015232357215E-15 ) ) ;
#15993 = CARTESIAN_POINT ( 'NONE',  ( 104.4587341249999781, -1.846868145590721655, 6.125000001365592084 ) ) ;
#15994 = CARTESIAN_POINT ( 'NONE',  ( 65.00000000000000000, 37.97382812608393721, -13.14518615778179544 ) ) ;
#15995 = CARTESIAN_POINT ( 'NONE',  ( 2.493653234604083739E-15, 38.81718749999999574, 13.57481594606304576 ) ) ;
#15996 = CARTESIAN_POINT ( 'NONE',  ( 181.8548138422182205, 36.58476562608393579, 0.000000000000000000 ) ) ;
#15997 = ORIENTED_EDGE ( 'NONE', *, *, #19057, .T. ) ;
#15998 = CARTESIAN_POINT ( 'NONE',  ( 13.14518615778179722, 33.95546875108394147, 5.444914386472293977 ) ) ;
#15999 =( BOUNDED_CURVE ( )  B_SPLINE_CURVE ( 2, ( #16909, #27898, #27354, #14758, #19195, #1552, #5549, #12200, #1270 ),
 .UNSPECIFIED., .F., .F. ) 
 B_SPLINE_CURVE_WITH_KNOTS ( ( 3, 2, 2, 2, 3 ),
 ( 0.7857142857142856984, 0.7946428571428570953, 0.8035714285714286031, 0.8125000000000000000, 0.8214285714285713969 ),
 .UNSPECIFIED. ) 
 CURVE ( )  GEOMETRIC_REPRESENTATION_ITEM ( )  RATIONAL_B_SPLINE_CURVE ( ( 1.000000000000000000, 0.9238795325112867385, 1.000000000000000000, 0.9238795325112867385, 1.000000000000000000, 0.9238795325112867385, 1.000000000000000000, 0.9238795325112867385, 1.000000000000000000 ) ) 
 REPRESENTATION_ITEM ( '' )  );
#16000 = ORIENTED_EDGE ( 'NONE', *, *, #10691, .T. ) ;
#16001 = CARTESIAN_POINT ( 'NONE',  ( 98.96446609406727646, 122.5500000021849587, -2.499999999999997780 ) ) ;
#16002 = CARTESIAN_POINT ( 'NONE',  ( 104.4587341249999781, 90.56249999863440792, -6.938893903907228378E-15 ) ) ;
#16003 = CARTESIAN_POINT ( 'NONE',  ( 185.7049497278729575, 36.88242187608393152, 9.295050272127047819 ) ) ;
#16004 = CARTESIAN_POINT ( 'NONE',  ( 95.00472066334982912, 116.8754121666685393, -52.17499999726881299 ) ) ;
#16005 = EDGE_LOOP ( 'NONE', ( #27633, #28133, #7478, #6650 ) ) ;
#16006 = CARTESIAN_POINT ( 'NONE',  ( 2.493653234604083739E-15, 32.46718749999999432, 13.57481594606304576 ) ) ;
#16007 = CARTESIAN_POINT ( 'NONE',  ( 5.444914386472302859, 32.86406250108392868, 13.14518615778179189 ) ) ;
#16008 = ORIENTED_EDGE ( 'NONE', *, *, #88, .T. ) ;
#16009 = CARTESIAN_POINT ( 'NONE',  ( 143.1451861577818079, 32.36796875108393579, 5.444914386472293977 ) ) ;
#16010 = CARTESIAN_POINT ( 'NONE',  ( 185.4011555911795597, 37.22968750216787726, 9.598844408820459861 ) ) ;
#16011 = CARTESIAN_POINT ( 'NONE',  ( 208.1451861577817795, 35.54296875108394715, 5.444914386472293977 ) ) ;
#16012 = ORIENTED_EDGE ( 'NONE', *, *, #6858, .T. ) ;
#16013 = CARTESIAN_POINT ( 'NONE',  ( 101.4615807364564546, 123.2500000010924879, 1.461580736456455476 ) ) ;
#16014 = DIRECTION ( 'NONE',  ( 5.782411586589358625E-17, -0.000000000000000000, 1.000000000000000000 ) ) ;
#16015 = CARTESIAN_POINT ( 'NONE',  ( 120.8198241863519797, 50.00000000000000000, -9.999999999999976907 ) ) ;
#16016 = CARTESIAN_POINT ( 'NONE',  ( 130.0000000000000000, 36.53515625216787299, 13.57481594606304576 ) ) ;
#16017 = CARTESIAN_POINT ( 'NONE',  ( 108.0825317500000011, 112.6261737610028320, -48.02500000273118985 ) ) ;
#16018 = EDGE_CURVE ( 'NONE', #10588, #15564, #23367, .T. ) ;
#16019 = CARTESIAN_POINT ( 'NONE',  ( 108.0825317500000153, 110.0000000000000000, -44.25000000273119838 ) ) ;
#16020 = CARTESIAN_POINT ( 'NONE',  ( -13.57481594606304398, 34.00507812716787726, 5.622872871577880183 ) ) ;
#16021 = CARTESIAN_POINT ( 'NONE',  ( 200.4449143864723055, 40.20625000108394431, 13.14518615778179189 ) ) ;
#16022 = ORIENTED_EDGE ( 'NONE', *, *, #26189, .F. ) ;
#16023 = CARTESIAN_POINT ( 'NONE',  ( 104.4587341249999639, 1.442382525525748735E-14, 2.937500001365592528 ) ) ;
#16024 = ORIENTED_EDGE ( 'NONE', *, *, #23185, .T. ) ;
#16025 = CARTESIAN_POINT ( 'NONE',  ( 2.007297010069739596, 35.99999999999998579, -13.40042260803723373 ) ) ;
#16026 = CARTESIAN_POINT ( 'NONE',  ( 103.1528011352953342, 3.152801135295383084, 9.062500001365592084 ) ) ;
#16027 = DIRECTION ( 'NONE',  ( 0.000000000000000000, 0.000000000000000000, -1.000000000000000000 ) ) ;
#16028 = CARTESIAN_POINT ( 'NONE',  ( 13.14518615778179900, 37.03125000108393294, -5.444914386472297529 ) ) ;
#16029 = CYLINDRICAL_SURFACE ( 'NONE', #13314, 25.00000000000001066 ) ;
#16030 = CARTESIAN_POINT ( 'NONE',  ( 55.70494972787295751, 33.50898437608393010, -9.295050272127046043 ) ) ;
#16031 = CARTESIAN_POINT ( 'NONE',  ( -15.00000000000000355, 55.00000000000000000, -9.999999999999998224 ) ) ;
#16032 = CARTESIAN_POINT ( 'NONE',  ( 217.9999999999999716, 80.00000000000000000, 14.99999999999994316 ) ) ;
#16033 = DIRECTION ( 'NONE',  ( 0.000000000000000000, 0.000000000000000000, -1.000000000000000000 ) ) ;
#16034 =( BOUNDED_CURVE ( )  B_SPLINE_CURVE ( 2, ( #4183, #8729, #19424, #21857, #2469, #4464, #8870, #23845, #17849 ),
 .UNSPECIFIED., .F., .F. ) 
 B_SPLINE_CURVE_WITH_KNOTS ( ( 3, 2, 2, 2, 3 ),
 ( 0.6874999999999997780, 0.6979166666666665186, 0.7083333333333333703, 0.7187500000000001110, 0.7291666666666668517 ),
 .UNSPECIFIED. ) 
 CURVE ( )  GEOMETRIC_REPRESENTATION_ITEM ( )  RATIONAL_B_SPLINE_CURVE ( ( 1.000000000000001554, 0.9238795325112850731, 1.000000000000000000, 0.9238795325112867385, 1.000000000000000000, 0.9238795325112867385, 1.000000000000000000, 0.9238795325112850731, 1.000000000000001554 ) ) 
 REPRESENTATION_ITEM ( '' )  );
#16035 = LINE ( 'NONE', #7197, #10268 ) ;
#16036 = CARTESIAN_POINT ( 'NONE',  ( -1.014130826074097769, 51.45790058219388641, 14.99999999999932143 ) ) ;
#16037 = FACE_BOUND ( 'NONE', #13271, .T. ) ;
#16038 = CARTESIAN_POINT ( 'NONE',  ( 120.4011555911795455, 33.16171874999999858, 9.598844408820459861 ) ) ;
#16039 = VECTOR ( 'NONE', #6118, 1000.000000000000000 ) ;
#16040 = ORIENTED_EDGE ( 'NONE', *, *, #23640, .T. ) ;
#16041 = CARTESIAN_POINT ( 'NONE',  ( -20.00000000000000000, 80.00000000000000000, 15.00000000000000178 ) ) ;
#16042 = CARTESIAN_POINT ( 'NONE',  ( 13.14518615778179544, 34.79882812608394005, -1.609821015232357215E-15 ) ) ;
#16043 = CARTESIAN_POINT ( 'NONE',  ( 5.622872871577878406, 34.99726562716787726, 13.57481594606304576 ) ) ;
#16044 = CARTESIAN_POINT ( 'NONE',  ( 102.0710678118654329, -4.999999999999989342, 8.437500002731185944 ) ) ;
#16045 = CARTESIAN_POINT ( 'NONE',  ( 124.5550856135277087, 34.05468750108393294, -13.14518615778179900 ) ) ;
#16046 = B_SPLINE_CURVE_WITH_KNOTS ( 'NONE', 3,
 ( #8468, #17156, #23311, #10168 ),
 .UNSPECIFIED., .F., .F.,
 ( 4, 4 ),
 ( 0.000000000000000000, 1.000000000000000000 ),
 .UNSPECIFIED. ) ;
#16047 = PRODUCT ( 'Suction Cups Set (x4)', 'Suction Cups Set (x4)', '', ( #21235 ) ) ;
#16048 = CARTESIAN_POINT ( 'NONE',  ( 78.57481594606304043, 31.92148437716787512, 5.622872871577869525 ) ) ;
#16049 = CYLINDRICAL_SURFACE ( 'NONE', #10220, 13.57481594606304398 ) ;
#16050 = CARTESIAN_POINT ( 'NONE',  ( 13.14518615778179900, 39.31328125108392868, 5.444914386472293977 ) ) ;
#16051 = CARTESIAN_POINT ( 'NONE',  ( -9.295050272127046043, 32.71523437608393436, -9.295050272127046043 ) ) ;
#16052 = DIRECTION ( 'NONE',  ( -0.000000000000000000, 1.000000000000000000, -0.000000000000000000 ) ) ;
#16053 = CARTESIAN_POINT ( 'NONE',  ( 91.91746824999997045, 107.3738262389971680, -55.77499999726881441 ) ) ;
#16054 = EDGE_CURVE ( 'NONE', #10198, #17238, #15323, .T. ) ;
#16055 = CARTESIAN_POINT ( 'NONE',  ( 13.57481594606304931, 39.06523437716786873, 5.622872871577869525 ) ) ;
#16056 = CARTESIAN_POINT ( 'NONE',  ( -8.049105076161786076E-16, 40.35507812608393152, -13.14518615778179544 ) ) ;
#16057 = CYLINDRICAL_SURFACE ( 'NONE', #1541, 13.57481594606304576 ) ;
#16058 = CARTESIAN_POINT ( 'NONE',  ( -13.57481594606304753, 33.11210937716787583, -5.622872871577872189 ) ) ;
#16059 = AXIS2_PLACEMENT_3D ( 'NONE', #5082, #13744, #22468 ) ;
#16060 = CARTESIAN_POINT ( 'NONE',  ( 99.99999999999998579, 123.5500000010924850, -2.066987299999998751 ) ) ;
#16061 = DIRECTION ( 'NONE',  ( 0.000000000000000000, 0.000000000000000000, -1.000000000000000000 ) ) ;
#16062 = CARTESIAN_POINT ( 'NONE',  ( 99.99999999999995737, 1.387778780781445676E-14, 34.79898987322334136 ) ) ;
#16063 = DIRECTION ( 'NONE',  ( 0.8660254037844418162, -0.000000000000000000, 0.4999999999999947264 ) ) ;
#16064 = CARTESIAN_POINT ( 'NONE',  ( -13.57481594606304753, 35.39414062499999147, -5.622872871577873077 ) ) ;
#16065 = CARTESIAN_POINT ( 'NONE',  ( -8.312177448680279460E-16, 40.80156249999999574, -13.57481594606304576 ) ) ;
#16066 = CARTESIAN_POINT ( 'NONE',  ( -5.444914386472297529, 35.04687500108393294, -13.14518615778179900 ) ) ;
#16067 = CARTESIAN_POINT ( 'NONE',  ( -9.295050272127046043, 33.31054687608393294, -9.295050272127046043 ) ) ;
#16068 = CARTESIAN_POINT ( 'NONE',  ( 195.0000000000000000, 32.07031249999999289, -13.57481594606304576 ) ) ;
#16069 = CARTESIAN_POINT ( 'NONE',  ( 9.598844408820456309, 37.62656250216787157, -9.598844408820458085 ) ) ;
#16070 = CARTESIAN_POINT ( 'NONE',  ( -13.57481594606304753, 37.87460937716787868, -5.622872871577872189 ) ) ;
#16071 = CARTESIAN_POINT ( 'NONE',  ( 104.4587341249999781, 84.00000000136560629, -1.846868145590750299 ) ) ;
#16072 = CARTESIAN_POINT ( 'NONE',  ( 70.44491438647230552, 32.36796875108393579, -13.14518615778179900 ) ) ;
#16073 = CARTESIAN_POINT ( 'NONE',  ( 84.99999999999998579, 120.0000000000000000, -45.00000000000000711 ) ) ;
#16074 = CARTESIAN_POINT ( 'NONE',  ( -13.57481594606304576, 35.54296875216788010, 0.000000000000000000 ) ) ;
#16075 = CARTESIAN_POINT ( 'NONE',  ( 97.98586169945060931, 123.0000000000000568, 0.5387381024522378548 ) ) ;
#16076 = CARTESIAN_POINT ( 'NONE',  ( -13.57481594606304576, 34.69960937499999432, 5.622872871577880183 ) ) ;
#16077 = CARTESIAN_POINT ( 'NONE',  ( 120.7049497278729575, 36.08867187608393579, 9.295050272127047819 ) ) ;
#16078 = VERTEX_POINT ( 'NONE', #19080 ) ;
#16079 = CARTESIAN_POINT ( 'NONE',  ( 97.92893218813451028, 81.81250000000001421, -5.000000000000018652 ) ) ;
#16080 = LINE ( 'NONE', #16232, #21689 ) ;
#16081 = CARTESIAN_POINT ( 'NONE',  ( 98.15313185440925281, 82.25000000136559208, -4.458734125000016313 ) ) ;
#16082 = CARTESIAN_POINT ( 'NONE',  ( 103.5355339059327235, 93.87500000000000000, 3.535533905932724874 ) ) ;
#16083 = CARTESIAN_POINT ( 'NONE',  ( 51.42518405393695957, 39.56132812716787583, 5.622872871577880183 ) ) ;
#16084 = VECTOR ( 'NONE', #4360, 1000.000000000000000 ) ;
#16085 = EDGE_CURVE ( 'NONE', #8914, #22555, #12646, .T. ) ;
#16086 = CARTESIAN_POINT ( 'NONE',  ( 91.91746824999998466, 110.0000000000000000, -47.62499999726882294 ) ) ;
#16087 = CARTESIAN_POINT ( 'NONE',  ( 78.14518615778179367, 32.36796875108393579, 5.444914386472293977 ) ) ;
#16088 = CARTESIAN_POINT ( 'NONE',  ( -13.57481594606304576, 38.76757812716787299, 5.622872871577880183 ) ) ;
#16089 = ORIENTED_EDGE ( 'NONE', *, *, #26904, .T. ) ;
#16090 = CARTESIAN_POINT ( 'NONE',  ( 104.9999999999999858, 95.00000000000000000, -6.938893903907228378E-15 ) ) ;
#16091 = CARTESIAN_POINT ( 'NONE',  ( 96.46446609406721961, 3.535533905932755072, 13.87499999999999822 ) ) ;
#16092 = ORIENTED_EDGE ( 'NONE', *, *, #27642, .T. ) ;
#16093 = CARTESIAN_POINT ( 'NONE',  ( 9.295050272127046043, 34.89804687608393863, -9.295050272127046043 ) ) ;
#16094 = CARTESIAN_POINT ( 'NONE',  ( 181.8548138422182205, 39.75976562608393294, 0.000000000000000000 ) ) ;
#16095 = EDGE_CURVE ( 'NONE', #25525, #15131, #794, .T. ) ;
#16096 = CARTESIAN_POINT ( 'NONE',  ( 5.444914386472302859, 34.45156250108392726, 13.14518615778179189 ) ) ;
#16097 = CARTESIAN_POINT ( 'NONE',  ( 104.9999999999999574, -2.071067811865462627, 13.56250000273118772 ) ) ;
#16098 = CARTESIAN_POINT ( 'NONE',  ( 143.1451861577818363, 40.20625000108393010, -5.444914386472297529 ) ) ;
#16099 = CARTESIAN_POINT ( 'NONE',  ( 2.414731522848535132E-15, 36.18789062608393436, 13.14518615778179544 ) ) ;
#16100 = EDGE_CURVE ( 'NONE', #11653, #24722, #6860, .T. ) ;
#16101 = CARTESIAN_POINT ( 'NONE',  ( 139.2950502721270425, 32.31835937608393294, -9.295050272127046043 ) ) ;
#16102 = CARTESIAN_POINT ( 'NONE',  ( 96.84719886470463734, 91.68749999863440792, -3.152801135295366208 ) ) ;
#16103 = CARTESIAN_POINT ( 'NONE',  ( 97.93301270000000613, 123.9500000010924765, -9.540979117872439019E-15 ) ) ;
#16104 = EDGE_CURVE ( 'NONE', #21810, #2105, #23012, .T. ) ;
#16105 = DIRECTION ( 'NONE',  ( 1.000000000000000000, 0.000000000000000000, 0.000000000000000000 ) ) ;
#16106 = CARTESIAN_POINT ( 'NONE',  ( 78.57481594606305464, 36.68398437716787441, 5.622872871577868636 ) ) ;
#16107 = CARTESIAN_POINT ( 'NONE',  ( 95.54126587499995082, -1.846868145590724986, 8.750000001365592084 ) ) ;
#16108 = FACE_OUTER_BOUND ( 'NONE', #3860, .T. ) ;
#16109 = CARTESIAN_POINT ( 'NONE',  ( 96.84719886470459471, -3.152801135295355994, 11.56250000136559208 ) ) ;
#16110 = CARTESIAN_POINT ( 'NONE',  ( 108.0825317500000153, 110.0000000000000000, -48.12500000273119838 ) ) ;
#16111 = CARTESIAN_POINT ( 'NONE',  ( 95.54126587499999346, 91.12499999863439371, 1.846868145590722543 ) ) ;
#16112 = CARTESIAN_POINT ( 'NONE',  ( 214.9999999999999716, 55.00000000000000000, 14.99999999999994316 ) ) ;
#16113 = DIRECTION ( 'NONE',  ( 0.000000000000000000, 0.000000000000000000, -1.000000000000000000 ) ) ;
#16114 = CARTESIAN_POINT ( 'NONE',  ( -13.14518615778179544, 32.02070312608393010, 0.000000000000000000 ) ) ;
#16115 = EDGE_CURVE ( 'NONE', #1696, #747, #5067, .T. ) ;
#16116 = VERTEX_POINT ( 'NONE', #11069 ) ;
#16117 = DIRECTION ( 'NONE',  ( -5.782411586589357392E-17, 0.000000000000000000, -1.000000000000000000 ) ) ;
#16118 = CARTESIAN_POINT ( 'NONE',  ( 0.000000000000000000, 23.00000000000000000, 0.000000000000000000 ) ) ;
#16119 = CARTESIAN_POINT ( 'NONE',  ( 181.8548138422181921, 36.53515625108392584, -5.444914386472297529 ) ) ;
#16120 =( BOUNDED_CURVE ( )  B_SPLINE_CURVE ( 2, ( #23560, #12702, #17127, #12280, #16857, #21426, #14288, #1905, #5620 ),
 .UNSPECIFIED., .F., .T. ) 
 B_SPLINE_CURVE_WITH_KNOTS ( ( 3, 2, 2, 2, 3 ),
 ( 0.06250000000000004163, 0.07291666666666665741, 0.08333333333333325932, 0.09374999999999987510, 0.1041666666666664909 ),
 .UNSPECIFIED. ) 
 CURVE ( )  GEOMETRIC_REPRESENTATION_ITEM ( )  RATIONAL_B_SPLINE_CURVE ( ( 0.9999999999999996669, 0.9238795325112870716, 1.000000000000000000, 0.9238795325112867385, 1.000000000000000000, 0.9238795325112867385, 1.000000000000000000, 0.9238795325112880708, 0.9999999999999986677 ) ) 
 REPRESENTATION_ITEM ( '' )  );
#16121 = ORIENTED_EDGE ( 'NONE', *, *, #4456, .T. ) ;
#16122 = CARTESIAN_POINT ( 'NONE',  ( 194.1234737346433405, 51.45968077934669793, -15.00000000000000000 ) ) ;
#16123 = CARTESIAN_POINT ( 'NONE',  ( 104.4587341249999781, 1.846868145590750299, 10.25000000136559386 ) ) ;
#16124 = EDGE_CURVE ( 'NONE', #17847, #58, #11634, .T. ) ;
#16125 = ORIENTED_EDGE ( 'NONE', *, *, #21370, .F. ) ;
#16126 = CARTESIAN_POINT ( 'NONE',  ( 104.9952793366501851, 103.1245878333314323, -52.67500000273119554 ) ) ;
#16127 = CARTESIAN_POINT ( 'NONE',  ( -9.295050272127044266, 35.89023437608393152, 9.295050272127047819 ) ) ;
#16128 = CARTESIAN_POINT ( 'NONE',  ( 130.0000000000000000, -7.395377635281828788, -1.503427012513233026E-14 ) ) ;
#16129 = CYLINDRICAL_SURFACE ( 'NONE', #781, 5.000000000000000888 ) ;
#16130 = CARTESIAN_POINT ( 'NONE',  ( 139.2950502721270425, 38.46992187608393010, 9.295050272127046043 ) ) ;
#16131 = CARTESIAN_POINT ( 'NONE',  ( 5.444914386472297529, 37.32890625108393579, -13.14518615778179722 ) ) ;
#16132 = CARTESIAN_POINT ( 'NONE',  ( -9.295050272127044266, 35.89023437608393152, 9.295050272127047819 ) ) ;
#16133 = CIRCLE ( 'NONE', #23866, 13.57481594606304576 ) ;
#16134 = EDGE_CURVE ( 'NONE', #540, #25247, #8594, .T. ) ;
#16135 = CARTESIAN_POINT ( 'NONE',  ( 101.8468681455907330, 91.37499999863439371, 4.458734124999979898 ) ) ;
#16136 = CARTESIAN_POINT ( 'NONE',  ( 71.45087934266470597, 50.00000000106856390, -11.97362904075383305 ) ) ;
#16137 = CARTESIAN_POINT ( 'NONE',  ( 106.5389055433251002, 114.7507929638356785, -48.17500000273120264 ) ) ;
#16138 = EDGE_CURVE ( 'NONE', #14731, #4566, #15913, .T. ) ;
#16139 = EDGE_LOOP ( 'NONE', ( #13897, #4364, #26796 ) ) ;
#16140 = LINE ( 'NONE', #18433, #7573 ) ;
#16141 = CARTESIAN_POINT ( 'NONE',  ( 9.295050272127047819, 35.49335937608393721, 9.295050272127046043 ) ) ;
#16142 = CARTESIAN_POINT ( 'NONE',  ( 95.54126587499996504, 1.846868145590750077, 7.625000001365592084 ) ) ;
#16143 = CARTESIAN_POINT ( 'NONE',  ( 74.29505027212704249, 36.88242187608393152, 9.295050272127046043 ) ) ;
#16144 = DIRECTION ( 'NONE',  ( 0.000000000000000000, 0.000000000000000000, 1.000000000000000000 ) ) ;
#16145 = LINE ( 'NONE', #20154, #5797 ) ;
#16146 = CARTESIAN_POINT ( 'NONE',  ( -13.14518615778179722, 35.14609375108393152, -5.444914386472297529 ) ) ;
#16147 = CARTESIAN_POINT ( 'NONE',  ( 99.99999999999998579, 123.1500000010924794, 2.066987299999980099 ) ) ;
#16148 = CARTESIAN_POINT ( 'NONE',  ( 104.4587341249999923, 92.49999999863440792, 1.846868145590726318 ) ) ;
#16149 = CARTESIAN_POINT ( 'NONE',  ( 185.7049497278729575, 39.26367187608393294, 9.295050272127047819 ) ) ;
#16150 = CARTESIAN_POINT ( 'NONE',  ( 97.50236033167490746, 117.6869444889999841, -52.27499999726882862 ) ) ;
#16151 = VERTEX_POINT ( 'NONE', #2689 ) ;
#16152 = AXIS2_PLACEMENT_3D ( 'NONE', #15337, #2260, #4527 ) ;
#16153 = CARTESIAN_POINT ( 'NONE',  ( -13.57481594606304576, 33.85624999999999574, 0.000000000000000000 ) ) ;
#16154 = CARTESIAN_POINT ( 'NONE',  ( -5.444914386472299306, 34.35234375108392868, 13.14518615778179722 ) ) ;
#16155 = EDGE_LOOP ( 'NONE', ( #17955, #9215, #17409, #11443, #7627 ) ) ;
#16156 = FACE_OUTER_BOUND ( 'NONE', #9593, .T. ) ;
#16157 = CARTESIAN_POINT ( 'NONE',  ( 55.70494972787295751, 40.05742187608393579, 9.295050272127047819 ) ) ;
#16158 = DIRECTION ( 'NONE',  ( 0.000000000000000000, 0.000000000000000000, 1.000000000000000000 ) ) ;
#16159 = CARTESIAN_POINT ( 'NONE',  ( 181.8548138422181921, 35.24531250108393721, 5.444914386472304635 ) ) ;
#16160 = VERTEX_POINT ( 'NONE', #18063 ) ;
#16161 = LINE ( 'NONE', #22739, #18449 ) ;
#16162 = CYLINDRICAL_SURFACE ( 'NONE', #10847, 7.000000000000006217 ) ;
#16163 = EDGE_CURVE ( 'NONE', #17097, #23414, #6658, .T. ) ;
#16164 = CARTESIAN_POINT ( 'NONE',  ( 143.5748159460630404, 38.27148437716787299, 5.622872871577869525 ) ) ;
#16165 = CARTESIAN_POINT ( 'NONE',  ( 106.5389055433251002, 105.2492070361643215, -46.32500000273119412 ) ) ;
#16166 = CARTESIAN_POINT ( 'NONE',  ( 130.0000000000000000, -7.395377635281828788, -1.503427012513233026E-14 ) ) ;
#16167 = DIRECTION ( 'NONE',  ( -0.000000000000000000, -0.000000000000000000, -1.000000000000000000 ) ) ;
#16168 = CARTESIAN_POINT ( 'NONE',  ( 72.08941727233755614, 49.99999999943687357, 11.59823041028754353 ) ) ;
#16169 = ORIENTED_EDGE ( 'NONE', *, *, #3840, .F. ) ;
#16170 = VECTOR ( 'NONE', #4834, 1000.000000000000000 ) ;
#16171 = ORIENTED_EDGE ( 'NONE', *, *, #19646, .F. ) ;
#16172 = CARTESIAN_POINT ( 'NONE',  ( 103.1528011352953342, -3.152801135295355106, 3.812500001365591640 ) ) ;
#16173 = ORIENTED_EDGE ( 'NONE', *, *, #7755, .T. ) ;
#16174 = CARTESIAN_POINT ( 'NONE',  ( -13.10247082172194943, 36.00000000000000711, -1.608626461598226420 ) ) ;
#16175 = CARTESIAN_POINT ( 'NONE',  ( 98.15313185440925281, -4.458734124999987891, 9.625000001365593860 ) ) ;
#16176 = CARTESIAN_POINT ( 'NONE',  ( 93.00000000000000000, 110.0000000000000000, -55.00000000000000711 ) ) ;
#16177 = DIRECTION ( 'NONE',  ( 0.000000000000000000, 0.000000000000000000, -1.000000000000000000 ) ) ;
#16178 = CARTESIAN_POINT ( 'NONE',  ( 103.5355339059327235, 95.74999999726881583, 3.535533905932724874 ) ) ;
#16179 = CARTESIAN_POINT ( 'NONE',  ( -13.57481594606304576, 40.30546875216787583, 0.000000000000000000 ) ) ;
#16180 = CARTESIAN_POINT ( 'NONE',  ( 108.0825317500000011, 107.3738262389971538, -48.22500000273118559 ) ) ;
#16181 = CARTESIAN_POINT ( 'NONE',  ( 65.00000000000000000, 38.02343749999999289, 13.57481594606304576 ) ) ;
#16182 = MECHANICAL_DESIGN_GEOMETRIC_PRESENTATION_REPRESENTATION (  '', ( #7058 ), #2989 ) ;
#16183 = AXIS2_PLACEMENT_3D ( 'NONE', #19979, #2598, #18116 ) ;
#16184 = CARTESIAN_POINT ( 'NONE',  ( -8.312177448680279460E-16, 35.34453125216787583, -13.57481594606304576 ) ) ;
#16185 = CARTESIAN_POINT ( 'NONE',  ( 3.044609456929385338, 53.89089363584395898, 14.99999999999999645 ) ) ;
#16186 = DIRECTION ( 'NONE',  ( 1.000000000000000000, 0.000000000000000000, 0.000000000000000000 ) ) ;
#16187 = CARTESIAN_POINT ( 'NONE',  ( 143.5748159460630404, 35.09648437499998863, -5.622872871577873077 ) ) ;
#16188 = ORIENTED_EDGE ( 'NONE', *, *, #14552, .T. ) ;
#16189 = LINE ( 'NONE', #9493, #21310 ) ;
#16190 = CARTESIAN_POINT ( 'NONE',  ( 9.295050272127047819, 34.69960937608393436, 9.295050272127046043 ) ) ;
#16191 = CARTESIAN_POINT ( 'NONE',  ( 13.57481594606304931, 32.71523437716787441, 5.622872871577869525 ) ) ;
#16192 = CARTESIAN_POINT ( 'NONE',  ( 103.5355339059327093, -3.535533905932726206, 6.500000002731185944 ) ) ;
#16193 = CARTESIAN_POINT ( 'NONE',  ( 120.7049497278729575, 34.30273437608393294, 9.295050272127047819 ) ) ;
#16194 = CARTESIAN_POINT ( 'NONE',  ( 51.85481384221820633, 40.55351562608393579, 0.000000000000000000 ) ) ;
#16195 = ORIENTED_EDGE ( 'NONE', *, *, #25008, .F. ) ;
#16196 = CARTESIAN_POINT ( 'NONE',  ( 104.9999999999999716, 1.449011120738813565E-14, 14.49999999999999822 ) ) ;
#16197 = CARTESIAN_POINT ( 'NONE',  ( 9.295050272127046043, 40.25585937608393294, -9.295050272127046043 ) ) ;
#16198 = CARTESIAN_POINT ( 'NONE',  ( 2.414731522848535132E-15, 33.80664062608393294, 13.14518615778179544 ) ) ;
#16199 = CARTESIAN_POINT ( 'NONE',  ( 99.99999999999998579, 97.00000000000000000, -6.938893903907228378E-15 ) ) ;
#16200 = CARTESIAN_POINT ( 'NONE',  ( 217.9999999999999716, 78.00000000000000000, 0.000000000000000000 ) ) ;
#16201 = CARTESIAN_POINT ( 'NONE',  ( -13.57481594606304753, 39.46210937716787726, -5.622872871577873077 ) ) ;
#16202 = CARTESIAN_POINT ( 'NONE',  ( 200.4449143864723055, 32.07031250108393294, 13.14518615778179189 ) ) ;
#16203 = VECTOR ( 'NONE', #25301, 1000.000000000000000 ) ;
#16204 = DIRECTION ( 'NONE',  ( 0.000000000000000000, -0.000000000000000000, 1.000000000000000000 ) ) ;
#16205 = CARTESIAN_POINT ( 'NONE',  ( -5.622872871577873966, 33.01289062716787726, -13.57481594606304753 ) ) ;
#16206 = CARTESIAN_POINT ( 'NONE',  ( 102.0669872999999797, 123.3500000010924680, -9.794112055954760458E-15 ) ) ;
#16208 = ORIENTED_EDGE ( 'NONE', *, *, #16454, .F. ) ;
#16207 = CARTESIAN_POINT ( 'NONE',  ( 128.1834995827138073, 36.00000000000000000, -13.35830014193465587 ) ) ;
#16209 = CARTESIAN_POINT ( 'NONE',  ( 99.99999999999995737, 1.387778780781445676E-14, 34.79898987322334136 ) ) ;
#16210 = CARTESIAN_POINT ( 'NONE',  ( 195.0000000000000000, -7.395377635281828788, -11.57481594606306707 ) ) ;
#16211 = CARTESIAN_POINT ( 'NONE',  ( 5.622872871577871301, 34.40195312499999858, -13.57481594606304753 ) ) ;
#16212 = LINE ( 'NONE', #20360, #19349 ) ;
#16213 =( BOUNDED_CURVE ( )  B_SPLINE_CURVE ( 2, ( #26056, #11210, #15643, #21791, #4256, #19503, #22074, #265, #2123, #4539, #123 ),
 .UNSPECIFIED., .F., .F. ) 
 B_SPLINE_CURVE_WITH_KNOTS ( ( 3, 2, 2, 2, 2, 3 ),
 ( 0.1000000000000000056, 0.1200000000000000233, 0.1400000000000000688, 0.1600000000000001144, 0.1800000000000001044, 0.2000000000000001776 ),
 .UNSPECIFIED. ) 
 CURVE ( )  GEOMETRIC_REPRESENTATION_ITEM ( )  RATIONAL_B_SPLINE_CURVE ( ( 1.000000000000000000, 0.9510565162951535312, 1.000000000000000000, 0.9510565162951535312, 1.000000000000000000, 0.9510565162951535312, 1.000000000000000000, 0.9510565162951535312, 1.000000000000000000, 0.9510565162951530871, 1.000000000000000444 ) ) 
 REPRESENTATION_ITEM ( '' )  );
#16214 = CARTESIAN_POINT ( 'NONE',  ( -13.14518615778179189, 34.45156250108394147, 5.444914386472304635 ) ) ;
#16215 = CARTESIAN_POINT ( 'NONE',  ( 9.295050272127046043, 33.11210937608393579, -9.295050272127046043 ) ) ;
#16216 = CARTESIAN_POINT ( 'NONE',  ( 185.4011555911795313, 32.96328124999999432, -9.598844408820458085 ) ) ;
#16217 = CARTESIAN_POINT ( 'NONE',  ( -13.57481594606304576, 36.33671875216787583, 0.000000000000000000 ) ) ;
#16218 = CARTESIAN_POINT ( 'NONE',  ( 5.622872871577832221, 36.48554687499999716, 13.57481594606309194 ) ) ;
#16219 = CARTESIAN_POINT ( 'NONE',  ( 130.0000000000000000, -7.395377635281828788, 13.57481594606302799 ) ) ;
#16220 = CARTESIAN_POINT ( 'NONE',  ( 55.70494972787295751, 32.71523437608393436, 9.295050272127047819 ) ) ;
#16221 = CARTESIAN_POINT ( 'NONE',  ( 102.4976396683250925, 117.6869444889999841, -53.97500000273119980 ) ) ;
#16222 = CARTESIAN_POINT ( 'NONE',  ( 5.622872871578015186, 34.99726562716787015, 13.57481594606290543 ) ) ;
#16223 = VECTOR ( 'NONE', #11646, 1000.000000000000000 ) ;
#16224 = CARTESIAN_POINT ( 'NONE',  ( -8.312177448680279460E-16, 39.31328125216787583, -13.57481594606304576 ) ) ;
#16225 = CARTESIAN_POINT ( 'NONE',  ( -5.622872871577873077, 33.21132812499999432, 13.57481594606304753 ) ) ;
#16226 = CARTESIAN_POINT ( 'NONE',  ( 99.99999999999997158, 117.3602355696678501, -46.99999999453764588 ) ) ;
#16227 = CARTESIAN_POINT ( 'NONE',  ( 116.8548138422182063, 35.14609375108393152, -5.444914386472297529 ) ) ;
#16228 = PRODUCT_DEFINITION_SHAPE ( 'NONE', 'NONE',  #28212 ) ;
#16229 = ORIENTED_EDGE ( 'NONE', *, *, #12587, .F. ) ;
#16230 = CARTESIAN_POINT ( 'NONE',  ( 96.46446609406721961, 80.87500000000000000, -3.535533905932755072 ) ) ;
#16231 = ADVANCED_FACE ( 'NONE', ( #24059 ), #15641, .T. ) ;
#16232 = CARTESIAN_POINT ( 'NONE',  ( 7.171391131791534868, 31.93754143773660203, -11.52591762960188149 ) ) ;
#16233 = CARTESIAN_POINT ( 'NONE',  ( 95.54126587499995082, 82.37500000136562051, -1.846868145590750077 ) ) ;
#16234 = CIRCLE ( 'NONE', #4870, 2.999999999999989786 ) ;
#16235 = CARTESIAN_POINT ( 'NONE',  ( 103.5355339059327235, 91.87500000000000000, 3.535533905932724874 ) ) ;
#16236 = FACE_OUTER_BOUND ( 'NONE', #25766, .T. ) ;
#16237 = CARTESIAN_POINT ( 'NONE',  ( 102.4976396683250783, 102.3130555110000159, -49.02499999726882152 ) ) ;
#16238 = CARTESIAN_POINT ( 'NONE',  ( 195.0000000000000000, 31.62382812608393579, -13.14518615778179544 ) ) ;
#16239 = CARTESIAN_POINT ( 'NONE',  ( 13.57481594606304753, 39.16445312716788152, -5.622872871577873077 ) ) ;
#16240 = ORIENTED_EDGE ( 'NONE', *, *, #21846, .T. ) ;
#16241 = CARTESIAN_POINT ( 'NONE',  ( 197.0072970100686405, 35.99999999999999289, -13.40042260803738650 ) ) ;
#16242 = CARTESIAN_POINT ( 'NONE',  ( 94.99999999999995737, -2.071067811865466624, 8.062500000000000000 ) ) ;
#16243 = ORIENTED_EDGE ( 'NONE', *, *, #6900, .F. ) ;
#16244 = CARTESIAN_POINT ( 'NONE',  ( -13.14518615778179189, 36.03906250108394005, 5.444914386472304635 ) ) ;
#16245 = CARTESIAN_POINT ( 'NONE',  ( 208.1451861577817795, 40.20625000108393010, -5.444914386472297529 ) ) ;
#16246 = CARTESIAN_POINT ( 'NONE',  ( -13.14518615778179189, 31.87187500108393223, 5.444914386472304635 ) ) ;
#16247 = CARTESIAN_POINT ( 'NONE',  ( 102.0710678118654329, -4.999999999999989342, 12.43750000273118950 ) ) ;
#16248 = CARTESIAN_POINT ( 'NONE',  ( 135.4449143864723339, 40.00781250108393294, 13.14518615778179189 ) ) ;
#16249 = CARTESIAN_POINT ( 'NONE',  ( 96.46446615806316061, 80.00000000000000000, -3.535533969928681852 ) ) ;
#16250 = CARTESIAN_POINT ( 'NONE',  ( 70.62287287157786864, 32.81445312499999289, -13.57481594606304753 ) ) ;
#16251 = CARTESIAN_POINT ( 'NONE',  ( 102.4999999999999716, 124.6500000000000199, -1.035533905932742638 ) ) ;
#16252 = DIRECTION ( 'NONE',  ( 0.000000000000000000, 0.000000000000000000, 1.000000000000000000 ) ) ;
#16253 = CARTESIAN_POINT ( 'NONE',  ( 95.54126587499996504, 1.387778780781445676E-14, 8.687500001365592084 ) ) ;
#16254 = CARTESIAN_POINT ( 'NONE',  ( 59.55508561352770158, 40.40468750108393436, -13.14518615778179900 ) ) ;
#16255 = CARTESIAN_POINT ( 'NONE',  ( 104.4587341249999639, 1.442382525525748735E-14, 9.937500001365592084 ) ) ;
#16256 = CARTESIAN_POINT ( 'NONE',  ( 97.83688103937537051, 103.3426043859339103, -50.10000000546237686 ) ) ;
#16257 = CARTESIAN_POINT ( 'NONE',  ( 99.99999999999998579, 91.31249999863440792, 4.458734124999981674 ) ) ;
#16258 = CARTESIAN_POINT ( 'NONE',  ( 208.5748159460630688, 39.85898437499999858, -5.622872871577873966 ) ) ;
#16259 = DIRECTION ( 'NONE',  ( 0.000000000000000000, 0.000000000000000000, 1.000000000000000000 ) ) ;
#16260 = CARTESIAN_POINT ( 'NONE',  ( -9.295050272127044266, 32.91367187608393152, 9.295050272127047819 ) ) ;
#16261 = VERTEX_POINT ( 'NONE', #262 ) ;
#16262 = CARTESIAN_POINT ( 'NONE',  ( 0.000000000000000000, 0.000000000000000000, 0.000000000000000000 ) ) ;
#16263 =( BOUNDED_SURFACE ( )  B_SPLINE_SURFACE ( 1, 2, ( 
 ( #7656, #16348, #24627, #13767, #16056, #23052, #5533, #14197, #22917, #23601, #27609, #23466, #21470, #6349, #1946, #14744, #17030, #1536, #21327, #23327, #10614, #4082, #19321, #28023, #8489, #10188, #25594, #3943, #17176, #1808, #6078, #25880, #5942, #5807, #12603, #10473, #19181, #27883, #25464, #14610, #15023, #3801, #23743, #21606, #27747, #18899, #16762, #4218, #8207, #14477, #12877, #23194, #8345, #2084, #10753, #6216, #19464, #12745, #19035, #7930, #3671, #1671, #16627, #25319, #8067, #16896, #12333, #25733, #21052, #12461, #21186, #10328, #14885, #2229, #5179, #22710, #13703, #26992, #26702, #24024, #15309, #20141, #7297, #26016, #15161, #13842, #3180, #7151, #26156, #22567, #23881, #17456, #22283, #8767, #16132, #4896, #17319, #4359, #11421, #11850, #3034, #621, #11703, #17992, #6624, #9437, #15846, #5323, #13560, #20428, #13015, #2758, #9295, #24556, #24840, #5037, #6487, #21754, #22420, #28161, #912, #2891, #9582, #11561, #20277, #18137, #764, #13982, #26850, #15986, #8628, #24700, #18286, #7438, #10893, #19601, #85, #27407, #18975, #1196, #27135, #3874, #7868, #21121, #27683, #9864, #18704, #12124, #14413, #18571, #23401, #1053, #25537, #8146, #16840, #14271, #24979, #8002, #11991, #16563, #5882, #6017, #14551, #25253, #1469, #14131, #5743, #7729, #23267, #16703, #3740, #12400, #1607, #22852, #9996, #23128, #10265, #3604, #12263, #14680, #27274, #18427, #20988 ),
 ( #16420, #20572, #9725, #20850, #3319, #25117, #7587, #1330, #16280, #5462, #20714, #10125, #5604, #22989, #18838, #3458, #25401, #27545, #2306, #8279, #6285, #24098, #21264, #4017, #21543, #19118, #4158, #15384, #27825, #21408, #10965, #12536, #14817, #17396, #6696, #25953, #19677, #10686, #8415, #27959, #12819, #19538, #10411, #16970, #26094, #1746, #19394, #13090, #23541, #23959, #28099, #8562, #6559, #12952, #4438, #25669, #20, #15239, #6151, #17535, #17105, #2161, #12683, #1887, #10551, #2018, #8703, #10823, #19259, #8845, #26239, #17252, #21830, #25809, #14961, #23681, #6427, #15096, #23817, #163, #4295, #21686, #13811, #17679, #18254, #732, #9129, #7406, #22389, #3001, #15678, #2588, #16099, #24524, #4575, #9405, #22533, #13235, #11106, #7264, #17963, #7120, #24378, #589, #881, #5146, #15955, #26673, #21968, #2445, #11674, #26385, #20396, #2861, #19820, #11529, #6840, #22109, #304, #26818, #18105, #22251, #2728, #19967, #8990, #15531, #24238, #6982, #24670, #9553, #4867, #4721, #26962, #13381, #11249, #17822, #15818, #445, #9267, #5009, #26527, #11391, #13531, #20112, #13674, #20246, #3424, #14516, #1295, #7838, #5288, #7970, #11960, #8110, #13953, #22962, #9965, #22821, #24946, #16670, #3709, #7698, #23232, #24806, #22679, #3569, #20682, #12371, #20817, #25367, #5432, #21089, #3289, #27242, #9695, #14379, #11819, #23095, #18395, #14100, #20542, #18808, #10095 ) ),
 .UNSPECIFIED., .F., .F., .T. ) 
 B_SPLINE_SURFACE_WITH_KNOTS ( ( 2, 2 ),
 ( 3, 2, 2, 2, 2, 2, 2, 2, 2, 2, 2, 2, 2, 2, 2, 2, 2, 2, 2, 2, 2, 2, 2, 2, 2, 2, 2, 2, 2, 2, 2, 2, 2, 2, 2, 2, 2, 2, 2, 2, 2, 2, 2, 2, 2, 2, 2, 2, 2, 2, 2, 2, 2, 2, 2, 2, 2, 2, 2, 2, 2, 2, 2, 2, 2, 2, 2, 2, 2, 2, 2, 2, 2, 2, 2, 2, 2, 2, 2, 2, 2, 2, 2, 2, 2, 2, 2, 2, 2, 2, 2, 3 ),
 ( 0.000000000000000000, 1.000000000000000000 ),
 ( 0.000000000000000000, 0.01041666666666666609, 0.02083333333333333218, 0.03125000000000000000, 0.04166666666666666435, 0.05208333333333333565, 0.06250000000000000000, 0.07291666666666667129, 0.08333333333333332871, 0.09375000000000000000, 0.1041666666666666713, 0.1145833333333333287, 0.1250000000000000000, 0.1354166666666666574, 0.1458333333333333426, 0.1562500000000000000, 0.1666666666666666574, 0.1770833333333333426, 0.1875000000000000000, 0.1979166666666666574, 0.2083333333333333426, 0.2187500000000000000, 0.2291666666666666574, 0.2395833333333333426, 0.2500000000000000000, 0.2604166666666666852, 0.2708333333333333148, 0.2812500000000000000, 0.2916666666666666852, 0.3020833333333333148, 0.3125000000000000000, 0.3229166666666666852, 0.3333333333333333148, 0.3437500000000000000, 0.3541666666666666852, 0.3645833333333333148, 0.3750000000000000000, 0.3854166666666666852, 0.3958333333333333148, 0.4062500000000000000, 0.4166666666666666852, 0.4270833333333333148, 0.4375000000000000000, 0.4479166666666666852, 0.4583333333333333148, 0.4687500000000000000, 0.4791666666666666852, 0.4895833333333333148, 0.5000000000000000000, 0.5104166666666666297, 0.5208333333333333703, 0.5312500000000000000, 0.5416666666666666297, 0.5520833333333333703, 0.5625000000000000000, 0.5729166666666666297, 0.5833333333333333703, 0.5937500000000000000, 0.6041666666666666297, 0.6145833333333333703, 0.6250000000000000000, 0.6354166666666666297, 0.6458333333333333703, 0.6562500000000000000, 0.6666666666666666297, 0.6770833333333333703, 0.6875000000000000000, 0.6979166666666666297, 0.7083333333333333703, 0.7187500000000000000, 0.7291666666666666297, 0.7395833333333333703, 0.7500000000000000000, 0.7604166666666666297, 0.7708333333333333703, 0.7812500000000000000, 0.7916666666666666297, 0.8020833333333333703, 0.8125000000000000000, 0.8229166666666666297, 0.8333333333333333703, 0.8437500000000000000, 0.8541666666666666297, 0.8645833333333333703, 0.8750000000000000000, 0.8854166666666666297, 0.8958333333333333703, 0.9062500000000000000, 0.9166666666666666297, 0.9270833333333333703, 0.9375000000000000000, 0.9448587001587775980 ),
 .UNSPECIFIED. ) 
 GEOMETRIC_REPRESENTATION_ITEM ( )  RATIONAL_B_SPLINE_SURFACE ( (
 ( 1.000000000000000000, 0.9238795325112867385, 1.000000000000000000, 0.9238795325112867385, 1.000000000000000000, 0.9238795325112867385, 1.000000000000000000, 0.9238795325112867385, 1.000000000000000000, 0.9238795325112867385, 1.000000000000000000, 0.9238795325112867385, 1.000000000000000000, 0.9238795325112867385, 1.000000000000000000, 0.9238795325112867385, 1.000000000000000000, 0.9238795325112867385, 1.000000000000000000, 0.9238795325112867385, 1.000000000000000000, 0.9238795325112867385, 1.000000000000000000, 0.9238795325112867385, 1.000000000000000000, 0.9238795325112867385, 1.000000000000000000, 0.9238795325112867385, 1.000000000000000000, 0.9238795325112867385, 1.000000000000000000, 0.9238795325112867385, 1.000000000000000000, 0.9238795325112867385, 1.000000000000000000, 0.9238795325112867385, 1.000000000000000000, 0.9238795325112867385, 1.000000000000000000, 0.9238795325112867385, 1.000000000000000000, 0.9238795325112867385, 1.000000000000000000, 0.9238795325112867385, 1.000000000000000000, 0.9238795325112867385, 1.000000000000000000, 0.9238795325112867385, 1.000000000000000000, 0.9238795325112867385, 1.000000000000000000, 0.9238795325112867385, 1.000000000000000000, 0.9238795325112867385, 1.000000000000000000, 0.9238795325112867385, 1.000000000000000000, 0.9238795325112867385, 1.000000000000000000, 0.9238795325112867385, 1.000000000000000000, 0.9238795325112867385, 1.000000000000000000, 0.9238795325112867385, 1.000000000000000000, 0.9238795325112867385, 1.000000000000000000, 0.9238795325112867385, 1.000000000000000000, 0.9238795325112867385, 1.000000000000000000, 0.9238795325112867385, 1.000000000000000000, 0.9238795325112867385, 1.000000000000000000, 0.9238795325112867385, 1.000000000000000000, 0.9238795325112867385, 1.000000000000000000, 0.9238795325112867385, 1.000000000000000000, 0.9238795325112867385, 1.000000000000000000, 0.9238795325112867385, 1.000000000000000000, 0.9238795325112867385, 1.000000000000000000, 0.9238795325112867385, 1.000000000000000000, 0.9238795325112867385, 1.000000000000000000, 0.9238795325112867385, 1.000000000000000000, 0.9238795325112867385, 1.000000000000000000, 0.9238795325112867385, 1.000000000000000000, 0.9238795325112867385, 1.000000000000000000, 0.9238795325112867385, 1.000000000000000000, 0.9238795325112867385, 1.000000000000000000, 0.9238795325112867385, 1.000000000000000000, 0.9238795325112867385, 1.000000000000000000, 0.9238795325112867385, 1.000000000000000000, 0.9238795325112867385, 1.000000000000000000, 0.9238795325112867385, 1.000000000000000000, 0.9238795325112867385, 1.000000000000000000, 0.9238795325112867385, 1.000000000000000000, 0.9238795325112867385, 1.000000000000000000, 0.9238795325112867385, 1.000000000000000000, 0.9238795325112867385, 1.000000000000000000, 0.9238795325112867385, 1.000000000000000000, 0.9238795325112867385, 1.000000000000000000, 0.9238795325112867385, 1.000000000000000000, 0.9238795325112867385, 1.000000000000000000, 0.9238795325112867385, 1.000000000000000000, 0.9238795325112867385, 1.000000000000000000, 0.9238795325112867385, 1.000000000000000000, 0.9238795325112867385, 1.000000000000000000, 0.9238795325112867385, 1.000000000000000000, 0.9238795325112867385, 1.000000000000000000, 0.9238795325112867385, 1.000000000000000000, 0.9238795325112867385, 1.000000000000000000, 0.9238795325112867385, 1.000000000000000000, 0.9238795325112867385, 1.000000000000000000, 0.9238795325112867385, 1.000000000000000000, 0.9238795325112867385, 1.000000000000000000, 0.9238795325112867385, 1.000000000000000000, 0.9238795325112867385, 1.000000000000000000, 0.9238795325112867385, 1.000000000000000000, 0.9238795325112867385, 1.000000000000000000, 0.9238795325112867385, 1.000000000000000000, 0.9238795325112867385, 1.000000000000000000, 0.9238795325112867385, 1.000000000000000000, 0.9238795325112867385, 1.000000000000000000, 0.9238795325112867385, 1.000000000000000000, 0.9238795325112867385, 1.000000000000000000, 0.9238795325112867385, 1.000000000000000000, 0.9238795325112867385, 1.000000000000000000, 0.9238795325112867385, 1.000000000000000000, 0.9462258211652395667, 0.9684275895297407288),
 ( 1.000000000000000000, 0.9238795325112867385, 1.000000000000000000, 0.9238795325112867385, 1.000000000000000000, 0.9238795325112867385, 1.000000000000000000, 0.9238795325112867385, 1.000000000000000000, 0.9238795325112867385, 1.000000000000000000, 0.9238795325112867385, 1.000000000000000000, 0.9238795325112867385, 1.000000000000000000, 0.9238795325112867385, 1.000000000000000000, 0.9238795325112867385, 1.000000000000000000, 0.9238795325112867385, 1.000000000000000000, 0.9238795325112867385, 1.000000000000000000, 0.9238795325112867385, 1.000000000000000000, 0.9238795325112867385, 1.000000000000000000, 0.9238795325112867385, 1.000000000000000000, 0.9238795325112867385, 1.000000000000000000, 0.9238795325112867385, 1.000000000000000000, 0.9238795325112867385, 1.000000000000000000, 0.9238795325112867385, 1.000000000000000000, 0.9238795325112867385, 1.000000000000000000, 0.9238795325112867385, 1.000000000000000000, 0.9238795325112867385, 1.000000000000000000, 0.9238795325112867385, 1.000000000000000000, 0.9238795325112867385, 1.000000000000000000, 0.9238795325112867385, 1.000000000000000000, 0.9238795325112867385, 1.000000000000000000, 0.9238795325112867385, 1.000000000000000000, 0.9238795325112867385, 1.000000000000000000, 0.9238795325112867385, 1.000000000000000000, 0.9238795325112867385, 1.000000000000000000, 0.9238795325112867385, 1.000000000000000000, 0.9238795325112867385, 1.000000000000000000, 0.9238795325112867385, 1.000000000000000000, 0.9238795325112867385, 1.000000000000000000, 0.9238795325112867385, 1.000000000000000000, 0.9238795325112867385, 1.000000000000000000, 0.9238795325112867385, 1.000000000000000000, 0.9238795325112867385, 1.000000000000000000, 0.9238795325112867385, 1.000000000000000000, 0.9238795325112867385, 1.000000000000000000, 0.9238795325112867385, 1.000000000000000000, 0.9238795325112867385, 1.000000000000000000, 0.9238795325112867385, 1.000000000000000000, 0.9238795325112867385, 1.000000000000000000, 0.9238795325112867385, 1.000000000000000000, 0.9238795325112867385, 1.000000000000000000, 0.9238795325112867385, 1.000000000000000000, 0.9238795325112867385, 1.000000000000000000, 0.9238795325112867385, 1.000000000000000000, 0.9238795325112867385, 1.000000000000000000, 0.9238795325112867385, 1.000000000000000000, 0.9238795325112867385, 1.000000000000000000, 0.9238795325112867385, 1.000000000000000000, 0.9238795325112867385, 1.000000000000000000, 0.9238795325112867385, 1.000000000000000000, 0.9238795325112867385, 1.000000000000000000, 0.9238795325112867385, 1.000000000000000000, 0.9238795325112867385, 1.000000000000000000, 0.9238795325112867385, 1.000000000000000000, 0.9238795325112867385, 1.000000000000000000, 0.9238795325112867385, 1.000000000000000000, 0.9238795325112867385, 1.000000000000000000, 0.9238795325112867385, 1.000000000000000000, 0.9238795325112867385, 1.000000000000000000, 0.9238795325112867385, 1.000000000000000000, 0.9238795325112867385, 1.000000000000000000, 0.9238795325112867385, 1.000000000000000000, 0.9238795325112867385, 1.000000000000000000, 0.9238795325112867385, 1.000000000000000000, 0.9238795325112867385, 1.000000000000000000, 0.9238795325112867385, 1.000000000000000000, 0.9238795325112867385, 1.000000000000000000, 0.9238795325112867385, 1.000000000000000000, 0.9238795325112867385, 1.000000000000000000, 0.9238795325112867385, 1.000000000000000000, 0.9238795325112867385, 1.000000000000000000, 0.9238795325112867385, 1.000000000000000000, 0.9238795325112867385, 1.000000000000000000, 0.9238795325112867385, 1.000000000000000000, 0.9238795325112867385, 1.000000000000000000, 0.9238795325112867385, 1.000000000000000000, 0.9238795325112867385, 1.000000000000000000, 0.9238795325112867385, 1.000000000000000000, 0.9238795325112867385, 1.000000000000000000, 0.9238795325112867385, 1.000000000000000000, 0.9238795325112867385, 1.000000000000000000, 0.9238795325112867385, 1.000000000000000000, 0.9238795325112867385, 1.000000000000000000, 0.9238795325112867385, 1.000000000000000000, 0.9238795325112867385, 1.000000000000000000, 0.9238795325112867385, 1.000000000000000000, 0.9462258211652395667, 0.9684275895297407288) ) ) 
 REPRESENTATION_ITEM ( '' )  SURFACE ( )  );
#16264 = CIRCLE ( 'NONE', #19903, 5.000000000000004441 ) ;
#16266 = ADVANCED_FACE ( 'NONE', ( #8946 ), #13343, .T. ) ;
#16265 = CARTESIAN_POINT ( 'NONE',  ( 95.00000000000000000, 91.50000000000000000, -7.551217303480904118E-15 ) ) ;
#16267 = EDGE_CURVE ( 'NONE', #8723, #4009, #9344, .T. ) ;
#16268 = CARTESIAN_POINT ( 'NONE',  ( 185.7049497278729575, 33.31054687608393294, -9.295050272127046043 ) ) ;
#16269 = ORIENTED_EDGE ( 'NONE', *, *, #25502, .T. ) ;
#16270 = CARTESIAN_POINT ( 'NONE',  ( 192.9753722744670767, 50.00000000050955862, -13.43320860980940701 ) ) ;
#16271 = CARTESIAN_POINT ( 'NONE',  ( 95.54126587499995082, 1.846868145590750077, 10.62500000136559208 ) ) ;
#16272 = ORIENTED_EDGE ( 'NONE', *, *, #13648, .T. ) ;
#16273 = CARTESIAN_POINT ( 'NONE',  ( 93.46109445667491400, 114.7507929638356785, -45.57500000273119412 ) ) ;
#16274 = CARTESIAN_POINT ( 'NONE',  ( -5.444914386472297529, 36.43593750108392726, -13.14518615778179900 ) ) ;
#16275 = LINE ( 'NONE', #7865, #11297 ) ;
#16276 = CARTESIAN_POINT ( 'NONE',  ( 9.598844408820459861, 38.91640624999999432, 9.598844408820456309 ) ) ;
#16277 = ADVANCED_FACE ( 'NONE', ( #26635 ), #19623, .T. ) ;
#16278 = CARTESIAN_POINT ( 'NONE',  ( 120.7049497278729575, 37.47773437608393010, 9.295050272127047819 ) ) ;
#16279 = CARTESIAN_POINT ( 'NONE',  ( 2.414731522848535132E-15, 38.56914062608393579, 13.14518615778179544 ) ) ;
#16280 = CARTESIAN_POINT ( 'NONE',  ( 13.14518615778179544, 40.35507812608393863, -1.609821015232357215E-15 ) ) ;
#16281 = CARTESIAN_POINT ( 'NONE',  ( 99.99999999999998579, 91.81249999863440792, -4.458734124999994997 ) ) ;
#16282 = CARTESIAN_POINT ( 'NONE',  ( -5.622872871577736298, 36.18789062716787441, -13.57481594606318254 ) ) ;
#16283 = CARTESIAN_POINT ( 'NONE',  ( 97.50236033167492167, 117.6869444889999841, -49.77500000273119696 ) ) ;
#16284 = DIRECTION ( 'NONE',  ( 0.000000000000000000, -1.000000000000000000, 0.000000000000000000 ) ) ;
#16285 = CARTESIAN_POINT ( 'NONE',  ( -5.444914386472297529, 31.87187500108393223, -13.14518615778179900 ) ) ;
#16286 = CARTESIAN_POINT ( 'NONE',  ( 104.4587341249999781, -1.846868145590721655, 8.125000001365592084 ) ) ;
#16287 = CARTESIAN_POINT ( 'NONE',  ( 101.8468681455907046, 84.37500000136563472, -4.458734125000016313 ) ) ;
#16288 = CARTESIAN_POINT ( 'NONE',  ( 95.54126587499996504, 84.56250000136560629, -1.387778780781445676E-14 ) ) ;
#16289 = DIRECTION ( 'NONE',  ( -0.000000000000000000, 1.000000000000000000, -0.000000000000000000 ) ) ;
#16290 = CARTESIAN_POINT ( 'NONE',  ( 195.0000000000000000, 37.18007812608393436, -13.14518615778179544 ) ) ;
#16291 = ORIENTED_EDGE ( 'NONE', *, *, #1505, .F. ) ;
#16292 = CARTESIAN_POINT ( 'NONE',  ( -9.295050272127046043, 35.89023437608393152, -9.295050272127046043 ) ) ;
#16294 = EDGE_CURVE ( 'NONE', #27236, #24786, #6433, .T. ) ;
#16293 = CARTESIAN_POINT ( 'NONE',  ( 98.23223304703363112, 122.8000000021849587, 1.767766952966351557 ) ) ;
#16295 = DIRECTION ( 'NONE',  ( 0.000000000000000000, 0.000000000000000000, -1.000000000000000000 ) ) ;
#16296 = EDGE_CURVE ( 'NONE', #10395, #21810, #19335, .T. ) ;
#16297 = CARTESIAN_POINT ( 'NONE',  ( 9.598844408820456309, 32.07031250216787299, -9.598844408820458085 ) ) ;
#16298 = CARTESIAN_POINT ( 'NONE',  ( 91.91746824999997045, 107.3738262389971538, -47.77499999726880731 ) ) ;
#16299 = CARTESIAN_POINT ( 'NONE',  ( -13.57481594606304753, 32.21914062500000142, -5.622872871577873077 ) ) ;
#16300 = CARTESIAN_POINT ( 'NONE',  ( 9.295050272127046043, 33.90585937608393152, -9.295050272127046043 ) ) ;
#16301 = ORIENTED_EDGE ( 'NONE', *, *, #21526, .F. ) ;
#16302 = CARTESIAN_POINT ( 'NONE',  ( 105.6631189606246153, 114.1144967660473242, -45.80000000000001137 ) ) ;
#16303 = CARTESIAN_POINT ( 'NONE',  ( 103.5355339059327093, -3.535533905932726206, 0.5000000027311855000 ) ) ;
#16304 = ORIENTED_EDGE ( 'NONE', *, *, #25372, .T. ) ;
#16305 = ADVANCED_FACE ( 'NONE', ( #16353 ), #9513, .T. ) ;
#16306 = CARTESIAN_POINT ( 'NONE',  ( 0.000000000000000000, 40.99999999999999289, -13.57481594606304576 ) ) ;
#16307 = AXIS2_PLACEMENT_3D ( 'NONE', #10005, #5753, #17898 ) ;
#16308 = CARTESIAN_POINT ( 'NONE',  ( 200.4449143864723055, 33.36015625108393579, -13.14518615778179900 ) ) ;
#16309 = ORIENTED_EDGE ( 'NONE', *, *, #16663, .F. ) ;
#16310 = DIRECTION ( 'NONE',  ( -0.000000000000000000, -0.000000000000000000, -1.000000000000000000 ) ) ;
#16311 = CARTESIAN_POINT ( 'NONE',  ( 99.99999999999995737, 5.000000000000018652, 8.875000002731184168 ) ) ;
#16312 = CARTESIAN_POINT ( 'NONE',  ( 103.1528011352953342, -3.152801135295355106, 1.062500001365592528 ) ) ;
#16313 = CARTESIAN_POINT ( 'NONE',  ( 99.99999999999995737, 1.387778780781445676E-14, 34.79898987322334136 ) ) ;
#16314 = EDGE_CURVE ( 'NONE', #24113, #17588, #24084, .T. ) ;
#16315 = CARTESIAN_POINT ( 'NONE',  ( 116.4251840539369596, 38.71796875216787726, 0.000000000000000000 ) ) ;
#16316 = CARTESIAN_POINT ( 'NONE',  ( 106.9999999999999716, 1.473504056721760595E-14, 0.000000000000000000 ) ) ;
#16317 = DIRECTION ( 'NONE',  ( 0.000000000000000000, -1.000000000000000000, -0.000000000000000000 ) ) ;
#16318 = CARTESIAN_POINT ( 'NONE',  ( 181.8548138422181921, 39.11484375108394573, -5.444914386472297529 ) ) ;
#16319 = ORIENTED_EDGE ( 'NONE', *, *, #25549, .F. ) ;
#16320 = CARTESIAN_POINT ( 'NONE',  ( 104.4587341249999781, 1.846868145590750299, 13.25000000136559208 ) ) ;
#16321 = CARTESIAN_POINT ( 'NONE',  ( -2.892062521303301548, 36.00000000000000711, -13.15766692561478024 ) ) ;
#16322 = DIRECTION ( 'NONE',  ( -0.000000000000000000, -1.000000000000000000, -0.000000000000000000 ) ) ;
#16323 = AXIS2_PLACEMENT_3D ( 'NONE', #6506, #15181, #4379 ) ;
#16324 = AXIS2_PLACEMENT_3D ( 'NONE', #838, #1397, #12049 ) ;
#16325 = CARTESIAN_POINT ( 'NONE',  ( -3.136173621348210983, 36.00000000000000711, 12.79489613812742554 ) ) ;
#16326 = CARTESIAN_POINT ( 'NONE',  ( 78.14518615778179367, 32.41757812608393863, -1.609821015232357215E-15 ) ) ;
#16327 = CARTESIAN_POINT ( 'NONE',  ( 102.0710678118654329, 92.06249999726878741, -5.000000000000011546 ) ) ;
#16328 = CARTESIAN_POINT ( 'NONE',  ( 9.295050272127047819, 39.46210937608393721, 9.295050272127046043 ) ) ;
#16329 = CARTESIAN_POINT ( 'NONE',  ( 5.622872871577863307, 40.45429687500001137, 13.57481594606306174 ) ) ;
#16330 = VECTOR ( 'NONE', #1543, 1000.000000000000000 ) ;
#16331 = DIRECTION ( 'NONE',  ( 1.000000000000000000, -0.000000000000000000, -7.228014483236696740E-18 ) ) ;
#16332 = CARTESIAN_POINT ( 'NONE',  ( 4.504887086316609945, 51.44650206077173493, 15.00000000000000000 ) ) ;
#16333 = CARTESIAN_POINT ( 'NONE',  ( 135.6228728715778971, 34.10429687499999574, 13.57481594606304576 ) ) ;
#16334 = EDGE_LOOP ( 'NONE', ( #16716, #26033, #5348, #27754 ) ) ;
#16335 = DIRECTION ( 'NONE',  ( 0.000000000000000000, -0.000000000000000000, 1.000000000000000000 ) ) ;
#16336 = CARTESIAN_POINT ( 'NONE',  ( -9.295050272127044266, 34.50117187608393721, 9.295050272127047819 ) ) ;
#16337 = CARTESIAN_POINT ( 'NONE',  ( 2.493653234604083739E-15, 34.15390625216787157, 13.57481594606304576 ) ) ;
#16338 = CARTESIAN_POINT ( 'NONE',  ( 102.0710678118654329, 5.000000000000018652, 4.812500002731185056 ) ) ;
#16339 = CARTESIAN_POINT ( 'NONE',  ( 135.4449143864723055, 40.50390625108394005, -13.14518615778179900 ) ) ;
#16340 = CARTESIAN_POINT ( 'NONE',  ( 51.42518405393695957, 31.62382812716787228, 5.622872871577880183 ) ) ;
#16341 = EDGE_CURVE ( 'NONE', #19908, #14596, #16491, .T. ) ;
#16342 = CARTESIAN_POINT ( 'NONE',  ( 55.40115559117954547, 37.03125000216787299, -9.598844408820458085 ) ) ;
#16343 = CARTESIAN_POINT ( 'NONE',  ( -13.14518615778179189, 37.42812500108393436, 5.444914386472304635 ) ) ;
#16344 = CARTESIAN_POINT ( 'NONE',  ( 65.00000000000000000, 50.00000000000000000, -7.517135062566165128E-15 ) ) ;
#16345 = PLANE ( 'NONE',  #18953 ) ;
#16346 = CARTESIAN_POINT ( 'NONE',  ( 106.5389055433250860, 105.2492070361643215, -55.07499999726882578 ) ) ;
#16347 =( NAMED_UNIT ( * ) PLANE_ANGLE_UNIT ( ) SI_UNIT ( $, .RADIAN. ) );
#16348 = CARTESIAN_POINT ( 'NONE',  ( -13.14518615778179900, 40.50390625108394005, -5.444914386472297529 ) ) ;
#16349 = LINE ( 'NONE', #18770, #4276 ) ;
#16350 = CARTESIAN_POINT ( 'NONE',  ( 97.50000000000000000, 125.0069999999781629, -9.540979117872439019E-15 ) ) ;
#16351 = VECTOR ( 'NONE', #14566, 1000.000000000000000 ) ;
#16352 = CARTESIAN_POINT ( 'NONE',  ( 101.4615807364564546, 124.0500000010924850, 1.461580736456455476 ) ) ;
#16353 = FACE_OUTER_BOUND ( 'NONE', #26456, .T. ) ;
#16354 = CARTESIAN_POINT ( 'NONE',  ( 104.3262379212492590, 104.0454443415356991, -47.30000000000000426 ) ) ;
#16355 = DIRECTION ( 'NONE',  ( 0.000000000000000000, 0.000000000000000000, 1.000000000000000000 ) ) ;
#16356 = CARTESIAN_POINT ( 'NONE',  ( -13.57481594606304753, 34.60039062499999574, -5.622872871577873077 ) ) ;
#16357 = CARTESIAN_POINT ( 'NONE',  ( 107.0000000000000000, 110.0000000000000000, -49.49999999453764588 ) ) ;
#16358 = CARTESIAN_POINT ( 'NONE',  ( 9.598844408820459861, 39.71015624999999716, 9.598844408820456309 ) ) ;
#16359 = CARTESIAN_POINT ( 'NONE',  ( 13.14518615778179900, 32.96328125108393436, 5.444914386472293977 ) ) ;
#16360 = CARTESIAN_POINT ( 'NONE',  ( -5.444914386472299306, 34.35234375108392868, 13.14518615778179722 ) ) ;
#16361 = CARTESIAN_POINT ( 'NONE',  ( 9.598844408820456309, 36.03906250216787299, -9.598844408820458085 ) ) ;
#16362 = CARTESIAN_POINT ( 'NONE',  ( -13.57481594606304398, 37.97382812716787726, 5.622872871577880183 ) ) ;
#16363 = CARTESIAN_POINT ( 'NONE',  ( 101.8468681455906903, 83.12500000136560629, -4.458734125000016313 ) ) ;
#16364 = CARTESIAN_POINT ( 'NONE',  ( 59.55508561352770158, 40.60312500108393863, -13.14518615778179900 ) ) ;
#16365 = CARTESIAN_POINT ( 'NONE',  ( 101.7677669209684552, 123.0000000000000000, 1.767766984964258992 ) ) ;
#16366 = CARTESIAN_POINT ( 'NONE',  ( 13.57481594606304576, 37.42812499999999432, -1.662435489736055892E-15 ) ) ;
#16367 = CARTESIAN_POINT ( 'NONE',  ( 13.57481594606304931, 34.20351562499999432, 5.622872871577869525 ) ) ;
#16368 = CARTESIAN_POINT ( 'NONE',  ( 91.91746824999998466, 110.0000000000000000, -55.87499999726882294 ) ) ;
#16369 = CARTESIAN_POINT ( 'NONE',  ( 120.7049497278729575, 35.29492187608393294, 9.295050272127047819 ) ) ;
#16370 = EDGE_LOOP ( 'NONE', ( #8702, #9117, #8363, #10944, #20420, #16883, #16514, #13224, #14114, #16022, #13401, #13572, #4673, #5964, #6446, #27416, #4555, #1609, #18100, #3519, #13787, #11983, #2077, #2607, #15991, #25082, #22277 ) ) ;
#16371 = CARTESIAN_POINT ( 'NONE',  ( 9.180175813647991845, 55.00000000000000000, -14.99999999999999822 ) ) ;
#16372 = DIRECTION ( 'NONE',  ( 0.000000000000000000, 1.000000000000000000, 0.000000000000000000 ) ) ;
#16373 = CARTESIAN_POINT ( 'NONE',  ( 94.99999999999995737, 79.18750000273121259, 2.071067811865466624 ) ) ;
#16374 = CARTESIAN_POINT ( 'NONE',  ( 99.99999999999998579, 91.25000000000000000, -4.999999999999997335 ) ) ;
#16375 = VECTOR ( 'NONE', #8369, 1000.000000000000000 ) ;
#16376 = CARTESIAN_POINT ( 'NONE',  ( 55.40115559117954547, 39.61093750216787868, 9.598844408820459861 ) ) ;
#16377 = CARTESIAN_POINT ( 'NONE',  ( 107.0000000000000000, 112.2744378736303332, -53.90000000000000568 ) ) ;
#16378 = CARTESIAN_POINT ( 'NONE',  ( 185.7049497278729575, 40.65273437608393436, -9.295050272127046043 ) ) ;
#16379 = CARTESIAN_POINT ( 'NONE',  ( 9.598844408820456309, 40.00781250216787299, -9.598844408820458085 ) ) ;
#16380 = ORIENTED_EDGE ( 'NONE', *, *, #26391, .T. ) ;
#16381 = VECTOR ( 'NONE', #23144, 1000.000000000000000 ) ;
#16382 = CARTESIAN_POINT ( 'NONE',  ( 97.92893218813451028, 5.000000000000018652, 7.812499999999999112 ) ) ;
#16383 = ORIENTED_EDGE ( 'NONE', *, *, #6824, .T. ) ;
#16384 = CARTESIAN_POINT ( 'NONE',  ( 9.295050272127047819, 33.90585937608393863, 9.295050272127046043 ) ) ;
#16385 = CARTESIAN_POINT ( 'NONE',  ( 200.6228728715778686, 32.91367187716787157, -13.57481594606304753 ) ) ;
#16386 =( BOUNDED_CURVE ( )  B_SPLINE_CURVE ( 2, ( #20314, #7040, #24589, #5072, #20033, #11594, #13734, #9056, #26738 ),
 .UNSPECIFIED., .F., .F. ) 
 B_SPLINE_CURVE_WITH_KNOTS ( ( 3, 2, 2, 2, 3 ),
 ( 0.8214285714285713969, 0.8303571428571429047, 0.8392857142857143016, 0.8482142857142856984, 0.8571428571428570953 ),
 .UNSPECIFIED. ) 
 CURVE ( )  GEOMETRIC_REPRESENTATION_ITEM ( )  RATIONAL_B_SPLINE_CURVE ( ( 1.000000000000000000, 0.9238795325112867385, 1.000000000000000000, 0.9238795325112867385, 1.000000000000000000, 0.9238795325112867385, 1.000000000000000000, 0.9238795325112867385, 1.000000000000000000 ) ) 
 REPRESENTATION_ITEM ( '' )  );
#16387 = DIRECTION ( 'NONE',  ( -0.000000000000000000, 1.000000000000000000, -0.000000000000000000 ) ) ;
#16388 = CARTESIAN_POINT ( 'NONE',  ( 99.99999999999995737, 5.000000000000018652, 11.87500000273118594 ) ) ;
#16389 = CARTESIAN_POINT ( 'NONE',  ( 116.8548138422182205, 39.80937500108393579, 5.444914386472304635 ) ) ;
#16390 = CARTESIAN_POINT ( 'NONE',  ( 97.50000000000000000, 123.5500000021849587, 1.035533905932725096 ) ) ;
#16391 = ADVANCED_FACE ( 'NONE', ( #10061 ), #25324, .F. ) ;
#16392 = CYLINDRICAL_SURFACE ( 'NONE', #21812, 13.57481594606304398 ) ;
#16393 = CARTESIAN_POINT ( 'NONE',  ( 103.1528011352953484, 92.18749999863440792, 3.152801135295352886 ) ) ;
#16394 = CARTESIAN_POINT ( 'NONE',  ( 98.23223304703363112, 124.8999999999999915, -1.767766952966370209 ) ) ;
#16395 = CARTESIAN_POINT ( 'NONE',  ( 181.4251840539369596, 40.25585937499999289, 5.622872871577880183 ) ) ;
#16396 = CONTEXT_DEPENDENT_SHAPE_REPRESENTATION ( #10398, #13759 ) ;
#16397 = CARTESIAN_POINT ( 'NONE',  ( -13.57481594606304753, 33.01289062499999716, -5.622872871577872189 ) ) ;
#16398 = CARTESIAN_POINT ( 'NONE',  ( 104.4587341249999639, 1.442382525525748735E-14, 7.187500001365592972 ) ) ;
#16399 = CARTESIAN_POINT ( 'NONE',  ( -5.622872871577964560, 37.77539062716787299, -13.57481594606295339 ) ) ;
#16400 = VECTOR ( 'NONE', #6705, 1000.000000000000000 ) ;
#16401 = CARTESIAN_POINT ( 'NONE',  ( 101.8468681455907046, -4.458734124999987891, 10.75000000136559208 ) ) ;
#16402 = CARTESIAN_POINT ( 'NONE',  ( 99.99999999999998579, 102.6397644303321215, -52.00000000546236834 ) ) ;
#16403 = CARTESIAN_POINT ( 'NONE',  ( 101.8468681455907330, 90.49999999863442213, -4.458734124999994997 ) ) ;
#16404 = CARTESIAN_POINT ( 'NONE',  ( 94.99999999999995737, 1.387778780781445676E-14, 4.000000000000000000 ) ) ;
#16405 = CARTESIAN_POINT ( 'NONE',  ( 108.0825317499999869, 107.3738262389971680, -52.72499999726881725 ) ) ;
#16406 = CARTESIAN_POINT ( 'NONE',  ( -5.444914386472299306, 32.96328125108393436, 13.14518615778179722 ) ) ;
#16407 = EDGE_LOOP ( 'NONE', ( #8052, #13188, #16787, #10482 ) ) ;
#16408 = CARTESIAN_POINT ( 'NONE',  ( 114.9999999999999858, 95.00000000000000000, 14.99999999999999289 ) ) ;
#16409 = CARTESIAN_POINT ( 'NONE',  ( -13.57481594606304753, 37.77539062499998579, -5.622872871577872189 ) ) ;
#16410 = CARTESIAN_POINT ( 'NONE',  ( 195.0000000000000000, 32.81445312608393294, 13.14518615778179544 ) ) ;
#16411 = ORIENTED_EDGE ( 'NONE', *, *, #23294, .T. ) ;
#16412 = CARTESIAN_POINT ( 'NONE',  ( 196.1387681171055419, 50.00000000043849013, -13.56816686242531667 ) ) ;
#16413 = CARTESIAN_POINT ( 'NONE',  ( 96.84719886470459471, -3.152801135295355994, 8.812500001365592084 ) ) ;
#16414 = ORIENTED_EDGE ( 'NONE', *, *, #7706, .F. ) ;
#16415 = CARTESIAN_POINT ( 'NONE',  ( 91.91746824999999887, 110.0000000000000000, -45.37500000273119838 ) ) ;
#16416 = CARTESIAN_POINT ( 'NONE',  ( 9.295050272127047819, 33.70742187608393436, 9.295050272127046043 ) ) ;
#16417 = DIRECTION ( 'NONE',  ( 0.000000000000000000, 0.000000000000000000, 1.000000000000000000 ) ) ;
#16418 = CARTESIAN_POINT ( 'NONE',  ( 13.14518615778179544, 38.56914062608393579, -1.609821015232357215E-15 ) ) ;
#16419 = CARTESIAN_POINT ( 'NONE',  ( 9.295050272127046043, 38.86679687608393863, -9.295050272127046043 ) ) ;
#16420 = CARTESIAN_POINT ( 'NONE',  ( -13.14518615778179544, 40.75195312608393294, 0.000000000000000000 ) ) ;
#16421 = CARTESIAN_POINT ( 'NONE',  ( 99.99999999999998579, 93.31249999863440792, 4.458734124999981674 ) ) ;
#16422 = DIRECTION ( 'NONE',  ( -0.000000000000000000, 1.000000000000000000, -0.000000000000000000 ) ) ;
#16423 = CARTESIAN_POINT ( 'NONE',  ( 0.000000000000000000, 50.00000000000000000, 0.000000000000000000 ) ) ;
#16424 =( BOUNDED_CURVE ( )  B_SPLINE_CURVE ( 2, ( #5913, #18734, #10295, #27432, #19001, #7896, #27713, #25284, #5770 ),
 .UNSPECIFIED., .F., .T. ) 
 B_SPLINE_CURVE_WITH_KNOTS ( ( 3, 2, 2, 2, 3 ),
 ( 0.3541666666666666852, 0.3645833333333332593, 0.3749999999999998890, 0.3854166666666665741, 0.3958333333333331483 ),
 .UNSPECIFIED. ) 
 CURVE ( )  GEOMETRIC_REPRESENTATION_ITEM ( )  RATIONAL_B_SPLINE_CURVE ( ( 1.000000000000000000, 0.9238795325112867385, 1.000000000000000000, 0.9238795325112867385, 1.000000000000000000, 0.9238795325112867385, 1.000000000000000000, 0.9238795325112879597, 0.9999999999999987788 ) ) 
 REPRESENTATION_ITEM ( '' )  );
#16425 = CARTESIAN_POINT ( 'NONE',  ( 13.14518615778179900, 33.16171875108393863, 5.444914386472293977 ) ) ;
#16426 = CARTESIAN_POINT ( 'NONE',  ( 101.8468681455907046, 4.458734125000016313, 8.375000001365592084 ) ) ;
#16427 = CARTESIAN_POINT ( 'NONE',  ( 104.4587341249999639, 82.18750000136559208, -1.442382525525748735E-14 ) ) ;
#16428 = PLANE ( 'NONE',  #26337 ) ;
#16429 = CARTESIAN_POINT ( 'NONE',  ( 9.598844408820456309, 39.21406250216787015, -9.598844408820458085 ) ) ;
#16430 = VERTEX_POINT ( 'NONE', #8349 ) ;
#16431 = CARTESIAN_POINT ( 'NONE',  ( 5.444914386472297529, 35.74140625108393721, -13.14518615778179722 ) ) ;
#16432 = CARTESIAN_POINT ( 'NONE',  ( 101.0355339059327378, 122.4500000021849502, -2.499999999999997780 ) ) ;
#16433 = CARTESIAN_POINT ( 'NONE',  ( 98.15313185440923860, 95.24999999863437949, 4.458734124999980786 ) ) ;
#16434 = CARTESIAN_POINT ( 'NONE',  ( 189.5550856135277229, 36.13828125108393152, 13.14518615778179722 ) ) ;
#16435 = CARTESIAN_POINT ( 'NONE',  ( 97.50236033167490746, 102.3130555110000159, -49.47499999726882436 ) ) ;
#16436 = CARTESIAN_POINT ( 'NONE',  ( 99.99999999999995737, 1.387778780781445676E-14, 34.79898987322334136 ) ) ;
#16437 = FACE_OUTER_BOUND ( 'NONE', #22956, .T. ) ;
#16438 = ORIENTED_EDGE ( 'NONE', *, *, #6239, .F. ) ;
#16439 = DIRECTION ( 'NONE',  ( 0.000000000000000000, -0.000000000000000000, 1.000000000000000000 ) ) ;
#16440 = CARTESIAN_POINT ( 'NONE',  ( 51.85481384221821344, 36.83281250108393579, 5.444914386472304635 ) ) ;
#16441 = CARTESIAN_POINT ( 'NONE',  ( 13.57481594606304753, 32.81445312716787299, -5.622872871577873966 ) ) ;
#16442 = CARTESIAN_POINT ( 'NONE',  ( -9.598844408820458085, 39.31328124999999574, -9.598844408820458085 ) ) ;
#16443 = EDGE_CURVE ( 'NONE', #6267, #2719, #4086, .T. ) ;
#16444 = ORIENTED_EDGE ( 'NONE', *, *, #18574, .F. ) ;
#16445 = CARTESIAN_POINT ( 'NONE',  ( 70.62287287157786864, 37.57695312499999574, -13.57481594606304753 ) ) ;
#16446 = CARTESIAN_POINT ( 'NONE',  ( 8.758334392354081288, 50.00000000000000000, -10.38725784494425675 ) ) ;
#16447 = CARTESIAN_POINT ( 'NONE',  ( -13.57481594606304753, 33.80664062499999289, -5.622872871577872189 ) ) ;
#16448 = CARTESIAN_POINT ( 'NONE',  ( 139.5988444088204687, 39.01562500216787299, 9.598844408820456309 ) ) ;
#16449 = DIRECTION ( 'NONE',  ( 0.000000000000000000, 0.000000000000000000, -1.000000000000000000 ) ) ;
#16450 = EDGE_CURVE ( 'NONE', #19200, #4367, #12406, .T. ) ;
#16451 = DIRECTION ( 'NONE',  ( -0.000000000000000000, -0.000000000000000000, -1.000000000000000000 ) ) ;
#16452 = CARTESIAN_POINT ( 'NONE',  ( 181.8548138422181921, 36.83281250108393579, 5.444914386472304635 ) ) ;
#16453 = ORIENTED_EDGE ( 'NONE', *, *, #2373, .F. ) ;
#16454 = EDGE_CURVE ( 'NONE', #11953, #2183, #56, .T. ) ;
#16455 = ORIENTED_EDGE ( 'NONE', *, *, #24130, .F. ) ;
#16456 = CARTESIAN_POINT ( 'NONE',  ( 104.4587341249999639, 1.442382525525748735E-14, 0.9375000013655925279 ) ) ;
#16457 = DIRECTION ( 'NONE',  ( 0.000000000000000000, -1.000000000000000000, 0.000000000000000000 ) ) ;
#16458 = CARTESIAN_POINT ( 'NONE',  ( -5.622872871577890841, 40.35507812499999147, 13.57481594606302444 ) ) ;
#16459 = ADVANCED_FACE ( 'NONE', ( #27568 ), #9746, .F. ) ;
#16460 = CARTESIAN_POINT ( 'NONE',  ( 103.1528011352953342, 83.81250000136560629, 3.152801135295355106 ) ) ;
#16461 = DIRECTION ( 'NONE',  ( -5.782411586589357392E-17, 0.000000000000000000, -1.000000000000000000 ) ) ;
#16462 = CARTESIAN_POINT ( 'NONE',  ( 104.9999999999999716, 91.93749999726880162, -2.071067811865478170 ) ) ;
#16463 = CARTESIAN_POINT ( 'NONE',  ( -9.295050272127044266, 40.05742187608393579, 9.295050272127047819 ) ) ;
#16464 = DIRECTION ( 'NONE',  ( 5.782411586589358625E-17, -0.000000000000000000, 1.000000000000000000 ) ) ;
#16465 = CARTESIAN_POINT ( 'NONE',  ( 12.89215161363577344, 36.00000000000001421, -4.169510824906851099 ) ) ;
#16466 = CARTESIAN_POINT ( 'NONE',  ( 9.180175813648009608, 49.99999999999999289, 14.99999999999999822 ) ) ;
#16467 = CARTESIAN_POINT ( 'NONE',  ( 116.4251840539369596, 33.90585937500000568, 5.622872871577880183 ) ) ;
#16468 = VERTEX_POINT ( 'NONE', #20735 ) ;
#16469 = EDGE_CURVE ( 'NONE', #9928, #24154, #14294, .T. ) ;
#16470 = ORIENTED_EDGE ( 'NONE', *, *, #27168, .F. ) ;
#16471 = CARTESIAN_POINT ( 'NONE',  ( 74.59884440882045453, 36.73359374999999716, -9.598844408820458085 ) ) ;
#16472 = CARTESIAN_POINT ( 'NONE',  ( -13.57481594606304576, 38.61874999999999147, 0.000000000000000000 ) ) ;
#16473 = CARTESIAN_POINT ( 'NONE',  ( 9.295050272127046043, 40.25585937608393294, -9.295050272127046043 ) ) ;
#16474 = CARTESIAN_POINT ( 'NONE',  ( 96.46446609406721961, -3.535533905932727539, 5.250000002731184168 ) ) ;
#16475 = CARTESIAN_POINT ( 'NONE',  ( 120.7049497278729575, 39.26367187608393294, 9.295050272127047819 ) ) ;
#16476 = CARTESIAN_POINT ( 'NONE',  ( 78.14518615778179367, 39.36289062608393152, -1.609821015232357215E-15 ) ) ;
#16477 = ORIENTED_EDGE ( 'NONE', *, *, #22954, .T. ) ;
#16478 = CARTESIAN_POINT ( 'NONE',  ( 60.62597786918168197, 36.00000000000000711, 12.40367315690567196 ) ) ;
#16479 = CARTESIAN_POINT ( 'NONE',  ( 9.295050272127046043, 38.66835937608393436, -9.295050272127046043 ) ) ;
#16480 = CARTESIAN_POINT ( 'NONE',  ( 97.50000000000000000, 124.3000000021849587, -9.540979117872439019E-15 ) ) ;
#16481 = DIRECTION ( 'NONE',  ( -0.000000000000000000, -1.000000000000000000, -0.000000000000000000 ) ) ;
#16482 = ADVANCED_FACE ( 'NONE', ( #5346 ), #27016, .F. ) ;
#16483 = CARTESIAN_POINT ( 'NONE',  ( 97.50236033167490746, 117.6869444889999841, -54.27499999726882862 ) ) ;
#16484 = ORIENTED_EDGE ( 'NONE', *, *, #5894, .T. ) ;
#16485 = SURFACE_STYLE_USAGE ( .BOTH. , #5532 ) ;
#16486 = DIRECTION ( 'NONE',  ( 0.000000000000000000, 0.000000000000000000, -1.000000000000000000 ) ) ;
#16487 = CARTESIAN_POINT ( 'NONE',  ( 141.2065315021356469, 36.00000000000001421, 7.323573988461032691 ) ) ;
#16488 = CARTESIAN_POINT ( 'NONE',  ( 101.7677669529663547, 123.7000000000000028, 1.767766952966350891 ) ) ;
#16489 = EDGE_CURVE ( 'NONE', #7335, #18339, #18858, .T. ) ;
#16490 = CARTESIAN_POINT ( 'NONE',  ( 101.4615807364564546, 122.8500000010924680, -1.461580736456474794 ) ) ;
#16491 = LINE ( 'NONE', #25186, #12322 ) ;
#16492 = ADVANCED_FACE ( 'NONE', ( #16726 ), #27162, .T. ) ;
#16493 = DIRECTION ( 'NONE',  ( -0.000000000000000000, -1.000000000000000000, -0.000000000000000000 ) ) ;
#16494 = CARTESIAN_POINT ( 'NONE',  ( 101.8468681455906903, 4.458734125000016313, 13.12500000136559208 ) ) ;
#16495 = CARTESIAN_POINT ( 'NONE',  ( 107.0000000000000000, 107.7255621263696241, -47.60000000546237686 ) ) ;
#16496 = ORIENTED_EDGE ( 'NONE', *, *, #18439, .T. ) ;
#16497 = CARTESIAN_POINT ( 'NONE',  ( -10.54595693695916125, 36.00000000000001421, -8.172591659953413412 ) ) ;
#16498 = CARTESIAN_POINT ( 'NONE',  ( 5.622872871577878406, 39.66054687500000142, 13.57481594606304576 ) ) ;
#16499 = CARTESIAN_POINT ( 'NONE',  ( 6.944426393311538881, 31.55306875057403104, -11.16113171639042356 ) ) ;
#16500 = CARTESIAN_POINT ( 'NONE',  ( -9.295050272127046043, 33.31054687608393294, -9.295050272127046043 ) ) ;
#16501 = EDGE_CURVE ( 'NONE', #19839, #26327, #3765, .T. ) ;
#16502 = AXIS2_PLACEMENT_3D ( 'NONE', #25566, #14993, #15128 ) ;
#16503 = CARTESIAN_POINT ( 'NONE',  ( -9.598844408820454532, 33.26093750216787726, 9.598844408820459861 ) ) ;
#16504 = FACE_OUTER_BOUND ( 'NONE', #5205, .T. ) ;
#16505 = CARTESIAN_POINT ( 'NONE',  ( 101.8468681455906903, 84.00000000136560629, 4.458734124999987891 ) ) ;
#16506 = CARTESIAN_POINT ( 'NONE',  ( 74.29505027212704249, 40.45429687608393721, -9.295050272127046043 ) ) ;
#16507 = CARTESIAN_POINT ( 'NONE',  ( 97.50236033167492167, 117.6869444889999841, -45.77500000273119696 ) ) ;
#16508 = CARTESIAN_POINT ( 'NONE',  ( 99.99999999999998579, 93.74999999999998579, 4.999999999999984013 ) ) ;
#16509 = VERTEX_POINT ( 'NONE', #1356 ) ;
#16510 = CARTESIAN_POINT ( 'NONE',  ( 99.99999999999998579, 122.7500000010924879, -2.066987299999998751 ) ) ;
#16511 = CARTESIAN_POINT ( 'NONE',  ( 101.7677669209684552, 123.0000000000000000, 1.767766984964258992 ) ) ;
#16512 = CARTESIAN_POINT ( 'NONE',  ( 107.0000000000000000, 112.2744378736303332, -47.39999999453763735 ) ) ;
#16513 = CARTESIAN_POINT ( 'NONE',  ( 116.8548138422182063, 36.03906250108394005, 5.444914386472304635 ) ) ;
#16514 = ORIENTED_EDGE ( 'NONE', *, *, #6390, .F. ) ;
#16515 = CARTESIAN_POINT ( 'NONE',  ( 139.5988444088204403, 37.62656250216787157, -9.598844408820458085 ) ) ;
#16516 = CARTESIAN_POINT ( 'NONE',  ( 65.00000000000000000, 38.12265625216787157, 13.57481594606304576 ) ) ;
#16517 = CARTESIAN_POINT ( 'NONE',  ( 95.54126587499995082, 84.37500000136562051, -1.846868145590750077 ) ) ;
#16518 = CARTESIAN_POINT ( 'NONE',  ( 143.1451861577818079, 38.61875000108393152, -5.444914386472297529 ) ) ;
#16519 = CARTESIAN_POINT ( 'NONE',  ( 51.84732309041283571, 36.00000000000001421, 0.5874252385153132527 ) ) ;
#16520 = CARTESIAN_POINT ( 'NONE',  ( 93.46109445667489979, 114.7507929638356785, -53.82499999726881867 ) ) ;
#16521 = CARTESIAN_POINT ( 'NONE',  ( -9.598844408820454532, 38.81718750216787583, 9.598844408820459861 ) ) ;
#16522 = ORIENTED_EDGE ( 'NONE', *, *, #25146, .T. ) ;
#16523 = VECTOR ( 'NONE', #24456, 1000.000000000000000 ) ;
#16524 = CARTESIAN_POINT ( 'NONE',  ( 97.92893218813451028, -4.999999999999989342, 8.187500000000000000 ) ) ;
#16525 = ORIENTED_EDGE ( 'NONE', *, *, #12453, .F. ) ;
#16526 = CARTESIAN_POINT ( 'NONE',  ( -5.444914386472299306, 34.55078125108393294, 13.14518615778179722 ) ) ;
#16527 = CARTESIAN_POINT ( 'NONE',  ( 204.2950502721270425, 39.26367187608393294, 9.295050272127046043 ) ) ;
#16528 = CARTESIAN_POINT ( 'NONE',  ( -8.312177448680279460E-16, 36.93203125216787441, -13.57481594606304576 ) ) ;
#16529 = CARTESIAN_POINT ( 'NONE',  ( 104.9999999999999574, 2.071067811865491937, 13.68750000273118772 ) ) ;
#16530 = CARTESIAN_POINT ( 'NONE',  ( 120.7049497278729575, 38.27148437608393294, 9.295050272127047819 ) ) ;
#16531 = EDGE_CURVE ( 'NONE', #22274, #17326, #6760, .T. ) ;
#16532 = CARTESIAN_POINT ( 'NONE',  ( 98.23223304703363112, 123.4000000021849530, -1.767766952966370209 ) ) ;
#16533 = CARTESIAN_POINT ( 'NONE',  ( 95.54126587499996504, 1.387778780781445676E-14, 14.43750000136559208 ) ) ;
#16534 = CARTESIAN_POINT ( 'NONE',  ( 103.1528011352953484, 94.43749999863440792, -3.152801135295366208 ) ) ;
#16535 = CARTESIAN_POINT ( 'NONE',  ( 101.0355339059327378, 123.6500000000000199, 2.499999999999977796 ) ) ;
#16536 = CARTESIAN_POINT ( 'NONE',  ( 181.4251840539369596, 39.36289062499999858, -5.622872871577873077 ) ) ;
#16537 = EDGE_CURVE ( 'NONE', #17550, #15224, #7463, .T. ) ;
#16538 = APPLICATION_PROTOCOL_DEFINITION ( 'draft international standard', 'automotive_design', 1998, #18624 ) ;
#16539 = CARTESIAN_POINT ( 'NONE',  ( 127.7020394139926651, 36.00000000000000000, 12.97104423350695690 ) ) ;
#16540 = CARTESIAN_POINT ( 'NONE',  ( 95.54126587499995082, -1.846868145590724986, 5.750000001365591196 ) ) ;
#16541 = CARTESIAN_POINT ( 'NONE',  ( 195.0000000000000000, 36.83281249999999574, -13.57481594606304576 ) ) ;
#16542 = CARTESIAN_POINT ( 'NONE',  ( 96.84719886470459471, -3.152801135295355994, 6.562500001365592084 ) ) ;
#16543 = CARTESIAN_POINT ( 'NONE',  ( 102.1631189606246295, 116.6573956140660897, -47.10000000546237686 ) ) ;
#16544 = CARTESIAN_POINT ( 'NONE',  ( 96.84719886470463734, 94.93749999863440792, -3.152801135295366208 ) ) ;
#16545 = CARTESIAN_POINT ( 'NONE',  ( 5.622872871577796694, 39.95820312499999716, -13.57481594606312036 ) ) ;
#16546 = DIRECTION ( 'NONE',  ( 0.000000000000000000, 1.000000000000000000, 0.000000000000000000 ) ) ;
#16547 = CARTESIAN_POINT ( 'NONE',  ( -5.444914386472299306, 34.55078125108393294, 13.14518615778179722 ) ) ;
#16548 = VERTEX_POINT ( 'NONE', #5628 ) ;
#16549 = CARTESIAN_POINT ( 'NONE',  ( 96.84719886470459471, 81.81250000136559208, 3.152801135295355994 ) ) ;
#16550 = CARTESIAN_POINT ( 'NONE',  ( 96.84719886470463734, 90.68749999863440792, -3.152801135295366208 ) ) ;
#16551 = CARTESIAN_POINT ( 'NONE',  ( 200.4449143864723055, 33.16171875108393152, -13.14518615778179900 ) ) ;
#16552 = VERTEX_POINT ( 'NONE', #23150 ) ;
#16553 =( BOUNDED_CURVE ( )  B_SPLINE_CURVE ( 2, ( #16836, #14268, #25533, #12121, #16560, #22987, #10407, #25398, #14812, #3456, #3737, #3870, #10261, #16699, #19114, #18971, #27679, #27821, #8142, #1326, #5878, #8275, #3600, #16965, #25665, #18702, #10122, #1883, #27270, #12397, #27405, #21260, #14548, #23537, #7866, #1742, #20985, #18835, #23397, #5741, #16418, #4013, #21118, #25251, #12679, #23263, #7999, #23125, #14409, #21405, #10546, #1466, #7726, #25115, #1605, #21827, #300, #17675, #17248, #21682, #4154, #26382, #28094, #17390, #10818, #13087, #8557, #22106, #27955, #2302, #2442, #14958, #21965, #19673, #11103, #15, #10962, #12814, #21537, #17101, #4718, #8412, #158, #25949, #19533, #19817, #15528, #23677, #2014, #19254, #12948, #10682, #26089, #24235, #19389, #25804, #6423, #13377, #15380, #23812, #15092, #2585, #8841, #4289, #6837, #2158, #8985, #6281, #8699, #6555, #15235, #23955, #17532, #4435, #26234, #6692, #24095, #4571, #13231, #7402, #2725, #24374, #24943, #16096, #15815, #13528, #13950, #24803, #11671, #9264, #14098, #2998, #22817, #5285, #20538, #11244, #17818, #24521, #24666, #15952, #27098, #2858, #4863, #5142, #26959, #20392, #22248, #878, #11388, #6978, #5007, #19963, #441, #20109, #20244, #26523, #11526, #13808, #9549, #11816, #26814, #22676, #22530, #729, #3149, #18251, #1021, #9692, #18392, #15674, #9402, #9125, #22386, #586, #7550, #16246, #5429, #18101, #17960, #13670, #26670, #7117, #7261 ),
 .UNSPECIFIED., .F., .F. ) 
 B_SPLINE_CURVE_WITH_KNOTS ( ( 3, 2, 2, 2, 2, 2, 2, 2, 2, 2, 2, 2, 2, 2, 2, 2, 2, 2, 2, 2, 2, 2, 2, 2, 2, 2, 2, 2, 2, 2, 2, 2, 2, 2, 2, 2, 2, 2, 2, 2, 2, 2, 2, 2, 2, 2, 2, 2, 2, 2, 2, 2, 2, 2, 2, 2, 2, 2, 2, 2, 2, 2, 2, 2, 2, 2, 2, 2, 2, 2, 2, 2, 2, 2, 2, 2, 2, 2, 2, 2, 2, 2, 2, 2, 2, 2, 2, 2, 2, 2, 2, 3 ),
 ( 0.000000000000000000, 0.01041666666666666609, 0.02083333333333333218, 0.03125000000000000000, 0.04166666666666666435, 0.05208333333333332871, 0.06250000000000000000, 0.07291666666666667129, 0.08333333333333332871, 0.09375000000000000000, 0.1041666666666666574, 0.1145833333333333287, 0.1250000000000000000, 0.1354166666666666574, 0.1458333333333333426, 0.1562500000000000000, 0.1666666666666666574, 0.1770833333333333426, 0.1875000000000000000, 0.1979166666666666574, 0.2083333333333333148, 0.2187500000000000000, 0.2291666666666666574, 0.2395833333333333426, 0.2500000000000000000, 0.2604166666666666852, 0.2708333333333333148, 0.2812500000000000000, 0.2916666666666666852, 0.3020833333333333148, 0.3125000000000000000, 0.3229166666666666852, 0.3333333333333333148, 0.3437500000000000000, 0.3541666666666666852, 0.3645833333333333148, 0.3750000000000000000, 0.3854166666666666852, 0.3958333333333333148, 0.4062500000000000000, 0.4166666666666666297, 0.4270833333333333148, 0.4375000000000000000, 0.4479166666666666852, 0.4583333333333333148, 0.4687500000000000000, 0.4791666666666666852, 0.4895833333333333148, 0.5000000000000000000, 0.5104166666666666297, 0.5208333333333333703, 0.5312500000000000000, 0.5416666666666666297, 0.5520833333333333703, 0.5625000000000000000, 0.5729166666666665186, 0.5833333333333333703, 0.5937500000000000000, 0.6041666666666666297, 0.6145833333333333703, 0.6250000000000000000, 0.6354166666666666297, 0.6458333333333333703, 0.6562500000000000000, 0.6666666666666666297, 0.6770833333333333703, 0.6875000000000000000, 0.6979166666666666297, 0.7083333333333333703, 0.7187500000000000000, 0.7291666666666666297, 0.7395833333333333703, 0.7500000000000000000, 0.7604166666666666297, 0.7708333333333333703, 0.7812500000000000000, 0.7916666666666666297, 0.8020833333333333703, 0.8125000000000000000, 0.8229166666666666297, 0.8333333333333332593, 0.8437500000000000000, 0.8541666666666666297, 0.8645833333333333703, 0.8750000000000000000, 0.8854166666666666297, 0.8958333333333333703, 0.9062500000000000000, 0.9166666666666666297, 0.9270833333333333703, 0.9375000000000000000, 0.9448586970929392370 ),
 .UNSPECIFIED. ) 
 CURVE ( )  GEOMETRIC_REPRESENTATION_ITEM ( )  RATIONAL_B_SPLINE_CURVE ( ( 1.000000000000000000, 0.9238795325112867385, 1.000000000000000000, 0.9238795325112867385, 1.000000000000000000, 0.9238795325112867385, 1.000000000000000000, 0.9238795325112867385, 1.000000000000000000, 0.9238795325112867385, 1.000000000000000000, 0.9238795325112867385, 1.000000000000000000, 0.9238795325112867385, 1.000000000000000000, 0.9238795325112867385, 1.000000000000000000, 0.9238795325112867385, 1.000000000000000000, 0.9238795325112867385, 1.000000000000000000, 0.9238795325112867385, 1.000000000000000000, 0.9238795325112867385, 1.000000000000000000, 0.9238795325112867385, 1.000000000000000000, 0.9238795325112867385, 1.000000000000000000, 0.9238795325112867385, 1.000000000000000000, 0.9238795325112867385, 1.000000000000000000, 0.9238795325112867385, 1.000000000000000000, 0.9238795325112867385, 1.000000000000000000, 0.9238795325112867385, 1.000000000000000000, 0.9238795325112867385, 1.000000000000000000, 0.9238795325112867385, 1.000000000000000000, 0.9238795325112867385, 1.000000000000000000, 0.9238795325112867385, 1.000000000000000000, 0.9238795325112867385, 1.000000000000000000, 0.9238795325112867385, 1.000000000000000000, 0.9238795325112867385, 1.000000000000000000, 0.9238795325112867385, 1.000000000000000000, 0.9238795325112867385, 1.000000000000000000, 0.9238795325112867385, 1.000000000000000000, 0.9238795325112867385, 1.000000000000000000, 0.9238795325112867385, 1.000000000000000000, 0.9238795325112867385, 1.000000000000000000, 0.9238795325112867385, 1.000000000000000000, 0.9238795325112867385, 1.000000000000000000, 0.9238795325112867385, 1.000000000000000000, 0.9238795325112867385, 1.000000000000000000, 0.9238795325112867385, 1.000000000000000000, 0.9238795325112867385, 1.000000000000000000, 0.9238795325112867385, 1.000000000000000000, 0.9238795325112867385, 1.000000000000000000, 0.9238795325112867385, 1.000000000000000000, 0.9238795325112867385, 1.000000000000000000, 0.9238795325112867385, 1.000000000000000000, 0.9238795325112867385, 1.000000000000000000, 0.9238795325112867385, 1.000000000000000000, 0.9238795325112867385, 1.000000000000000000, 0.9238795325112867385, 1.000000000000000000, 0.9238795325112867385, 1.000000000000000000, 0.9238795325112867385, 1.000000000000000000, 0.9238795325112867385, 1.000000000000000000, 0.9238795325112867385, 1.000000000000000000, 0.9238795325112867385, 1.000000000000000000, 0.9238795325112867385, 1.000000000000000000, 0.9238795325112867385, 1.000000000000000000, 0.9238795325112867385, 1.000000000000000000, 0.9238795325112867385, 1.000000000000000000, 0.9238795325112867385, 1.000000000000000000, 0.9238795325112867385, 1.000000000000000000, 0.9238795325112867385, 1.000000000000000000, 0.9238795325112867385, 1.000000000000000000, 0.9238795325112867385, 1.000000000000000000, 0.9238795325112867385, 1.000000000000000000, 0.9238795325112867385, 1.000000000000000000, 0.9238795325112867385, 1.000000000000000000, 0.9238795325112867385, 1.000000000000000000, 0.9238795325112867385, 1.000000000000000000, 0.9238795325112867385, 1.000000000000000000, 0.9238795325112867385, 1.000000000000000000, 0.9238795325112867385, 1.000000000000000000, 0.9238795325112867385, 1.000000000000000000, 0.9238795325112867385, 1.000000000000000000, 0.9238795325112867385, 1.000000000000000000, 0.9238795325112867385, 1.000000000000000000, 0.9238795325112867385, 1.000000000000000000, 0.9238795325112867385, 1.000000000000000000, 0.9238795325112867385, 1.000000000000000000, 0.9238795325112867385, 1.000000000000000000, 0.9238795325112867385, 1.000000000000000000, 0.9238795325112867385, 1.000000000000000000, 0.9238795325112867385, 1.000000000000000000, 0.9238795325112867385, 1.000000000000000000, 0.9238795325112867385, 1.000000000000000000, 0.9238795325112867385, 1.000000000000000000, 0.9238795325112867385, 1.000000000000000000, 0.9238795325112867385, 1.000000000000000000, 0.9238795325112867385, 1.000000000000000000, 0.9238795325112867385, 1.000000000000000000, 0.9238795325112867385, 1.000000000000000000, 0.9238795325112867385, 1.000000000000000000, 0.9238795325112867385, 1.000000000000000000, 0.9462258435690522607, 0.9684275710300105366 ) ) 
 REPRESENTATION_ITEM ( '' )  );
#16554 = CARTESIAN_POINT ( 'NONE',  ( 193.4945078184423153, 53.60078691996476152, -15.00000000000000000 ) ) ;
#16555 = CARTESIAN_POINT ( 'NONE',  ( 99.99999999999995737, 4.458734125000016313, 5.437500001365592972 ) ) ;
#16556 = ORIENTED_EDGE ( 'NONE', *, *, #7420, .T. ) ;
#16557 = CARTESIAN_POINT ( 'NONE',  ( 95.00472066334982912, 116.8754121666685393, -45.67500000273119554 ) ) ;
#16558 = CARTESIAN_POINT ( 'NONE',  ( -13.14518615778179544, 33.40976562608393863, 0.000000000000000000 ) ) ;
#16559 = DIRECTION ( 'NONE',  ( -0.000000000000000000, -0.000000000000000000, -1.000000000000000000 ) ) ;
#16560 = CARTESIAN_POINT ( 'NONE',  ( -8.049105076161786076E-16, 40.35507812608393152, -13.14518615778179544 ) ) ;
#16561 = CARTESIAN_POINT ( 'NONE',  ( 5.444914386472302859, 37.03125000108393294, 13.14518615778179189 ) ) ;
#16562 = CIRCLE ( 'NONE', #21570, 4.999999999999997335 ) ;
#16563 = CARTESIAN_POINT ( 'NONE',  ( -13.14518615778179189, 32.66562500108393863, 5.444914386472304635 ) ) ;
#16564 = CARTESIAN_POINT ( 'NONE',  ( 103.1528011352953484, 93.68749999863440792, -3.152801135295366208 ) ) ;
#16565 = DIRECTION ( 'NONE',  ( 0.000000000000000000, 0.000000000000000000, 1.000000000000000000 ) ) ;
#16566 = LINE ( 'NONE', #9868, #1665 ) ;
#16567 = CARTESIAN_POINT ( 'NONE',  ( -13.14518615778179189, 32.86406250108393579, 5.444914386472304635 ) ) ;
#16568 = CARTESIAN_POINT ( 'NONE',  ( 103.1528011352953342, -3.152801135295355106, 2.062500001365591640 ) ) ;
#16569 = CARTESIAN_POINT ( 'NONE',  ( 130.0000000000000000, 50.00000000000000000, -1.503427012513233026E-14 ) ) ;
#16570 = CARTESIAN_POINT ( 'NONE',  ( -13.14518615778179544, 37.37851562608393863, 0.000000000000000000 ) ) ;
#16571 = CARTESIAN_POINT ( 'NONE',  ( 181.4251840539369596, 38.61874999999999147, 0.000000000000000000 ) ) ;
#16572 = VERTEX_POINT ( 'NONE', #23010 ) ;
#16573 = CARTESIAN_POINT ( 'NONE',  ( -13.14518615778179722, 32.76484375108393010, -5.444914386472297529 ) ) ;
#16574 = CARTESIAN_POINT ( 'NONE',  ( 97.50000000000000000, 122.7500000021849615, 1.035533905932725096 ) ) ;
#16575 = CARTESIAN_POINT ( 'NONE',  ( 99.99999999999998579, 92.81249999863440792, -4.458734124999994997 ) ) ;
#16576 = LINE ( 'NONE', #10141, #16381 ) ;
#16577 = CARTESIAN_POINT ( 'NONE',  ( 106.5389055433250860, 114.7507929638356785, -54.67499999726882720 ) ) ;
#16578 = PRODUCT_RELATED_PRODUCT_CATEGORY ( 'part', '', ( #20393 ) ) ;
#16579 = EDGE_CURVE ( 'NONE', #16552, #2330, #25087, .T. ) ;
#16580 = CARTESIAN_POINT ( 'NONE',  ( 95.54126587499996504, 1.387778780781445676E-14, 0.5625000013655921949 ) ) ;
#16581 = CARTESIAN_POINT ( 'NONE',  ( -13.14518615778179544, 31.82226562608393650, 0.000000000000000000 ) ) ;
#16582 = ORIENTED_EDGE ( 'NONE', *, *, #24638, .T. ) ;
#16583 = CARTESIAN_POINT ( 'NONE',  ( 59.55508561352770158, 36.63437500108393863, -13.14518615778179722 ) ) ;
#16584 = DIRECTION ( 'NONE',  ( -0.000000000000000000, -1.000000000000000000, -0.000000000000000000 ) ) ;
#16585 = CARTESIAN_POINT ( 'NONE',  ( 13.57481594606304576, 35.04687499999999289, -1.662435489736055892E-15 ) ) ;
#16586 = ORIENTED_EDGE ( 'NONE', *, *, #14698, .T. ) ;
#16587 = CARTESIAN_POINT ( 'NONE',  ( 105.6631189606246295, 114.1144967660473242, -54.80000000000001137 ) ) ;
#16588 = VECTOR ( 'NONE', #17553, 1000.000000000000000 ) ;
#16589 = CARTESIAN_POINT ( 'NONE',  ( -4.858499290463643483, 49.99999999891524283, -12.70434618648844705 ) ) ;
#16590 = CARTESIAN_POINT ( 'NONE',  ( 198.0393970508025063, 53.88964894337311051, 14.99999999999994671 ) ) ;
#16591 = CARTESIAN_POINT ( 'NONE',  ( 124.3771271284221314, 34.60039062716786873, -13.57481594606304753 ) ) ;
#16592 =( BOUNDED_CURVE ( )  B_SPLINE_CURVE ( 2, ( #16508, #1556, #27493, #23070, #23211, #1415, #5688, #10209, #20516 ),
 .UNSPECIFIED., .F., .F. ) 
 B_SPLINE_CURVE_WITH_KNOTS ( ( 3, 2, 2, 2, 3 ),
 ( 0.7500000000000006661, 0.7750000000000006883, 0.8000000000000007105, 0.8250000000000007327, 0.8500000000000007550 ),
 .UNSPECIFIED. ) 
 CURVE ( )  GEOMETRIC_REPRESENTATION_ITEM ( )  RATIONAL_B_SPLINE_CURVE ( ( 0.9999999999999980016, 0.9238795325112887369, 1.000000000000000000, 0.9238795325112867385, 1.000000000000000000, 0.9238795325112867385, 1.000000000000000000, 0.9238795325112844070, 1.000000000000002442 ) ) 
 REPRESENTATION_ITEM ( '' )  );
#16593 = CARTESIAN_POINT ( 'NONE',  ( 93.00000000000000000, 107.7255621263696668, -44.40000000546237402 ) ) ;
#16594 = CARTESIAN_POINT ( 'NONE',  ( 13.57481594606304753, 32.02070312716787015, -5.622872871577873966 ) ) ;
#16595 = CARTESIAN_POINT ( 'NONE',  ( 189.5550856135277229, 36.93203125108394147, 13.14518615778179722 ) ) ;
#16596 = ORIENTED_EDGE ( 'NONE', *, *, #9191, .T. ) ;
#16597 = VERTEX_POINT ( 'NONE', #20871 ) ;
#16598 =( LENGTH_UNIT ( ) NAMED_UNIT ( * ) SI_UNIT ( .MILLI., .METRE. ) );
#16599 = CARTESIAN_POINT ( 'NONE',  ( 103.1528011352953342, 3.152801135295383084, 1.062500001365592528 ) ) ;
#16600 = CARTESIAN_POINT ( 'NONE',  ( 99.99999999999995737, 4.458734125000016313, 14.43750000136559208 ) ) ;
#16601 = CARTESIAN_POINT ( 'NONE',  ( 2.493653234604083739E-15, 33.36015625216786873, 13.57481594606304576 ) ) ;
#16602 = CARTESIAN_POINT ( 'NONE',  ( 95.54126587499996504, 83.50000000136560629, 1.846868145590724986 ) ) ;
#16603 = DIRECTION ( 'NONE',  ( 0.000000000000000000, 1.000000000000000000, 0.000000000000000000 ) ) ;
#16604 =( LENGTH_UNIT ( ) NAMED_UNIT ( * ) SI_UNIT ( .MILLI., .METRE. ) );
#16605 = CARTESIAN_POINT ( 'NONE',  ( 2.414731522848535132E-15, 40.15664062608393436, 13.14518615778179544 ) ) ;
#16606 = CARTESIAN_POINT ( 'NONE',  ( 95.54126587499996504, 79.68750000136559208, -1.387778780781445676E-14 ) ) ;
#16607 = VECTOR ( 'NONE', #27776, 1000.000000000000114 ) ;
#16608 = CARTESIAN_POINT ( 'NONE',  ( 94.99999999999995737, 82.93750000000001421, -2.071067811865491493 ) ) ;
#16609 = CARTESIAN_POINT ( 'NONE',  ( 104.9952793366501709, 103.1245878333314323, -48.92499999726882010 ) ) ;
#16610 = ORIENTED_EDGE ( 'NONE', *, *, #9167, .T. ) ;
#16611 = EDGE_LOOP ( 'NONE', ( #10022, #904, #22606, #6551 ) ) ;
#16612 = CARTESIAN_POINT ( 'NONE',  ( -5.622872871577965448, 37.27929687716785878, 13.57481594606295161 ) ) ;
#16613 = UNCERTAINTY_MEASURE_WITH_UNIT (LENGTH_MEASURE( 1.000000000000000082E-05 ), #16598, 'distance_accuracy_value', 'NONE');
#16614 = CARTESIAN_POINT ( 'NONE',  ( 6.944423624769117787, 31.75150628229955529, -11.16113343896966370 ) ) ;
#16615 = CARTESIAN_POINT ( 'NONE',  ( -13.14518615778179544, 40.55351562608393579, 0.000000000000000000 ) ) ;
#16616 = CARTESIAN_POINT ( 'NONE',  ( 104.9999999999999574, -2.071067811865462627, 5.562500002731184168 ) ) ;
#16617 = CARTESIAN_POINT ( 'NONE',  ( 116.8548138422182063, 39.90859375108394147, -5.444914386472297529 ) ) ;
#16618 = ADVANCED_FACE ( 'NONE', ( #10020 ), #18728, .T. ) ;
#16619 = CARTESIAN_POINT ( 'NONE',  ( 51.85481384221820633, 35.84062500108394289, 5.444914386472304635 ) ) ;
#16620 = ADVANCED_FACE ( 'NONE', ( #5765 ), #3626, .F. ) ;
#16621 = CARTESIAN_POINT ( 'NONE',  ( 1.137167824540872951, 35.99999999999998579, 13.09590655363602707 ) ) ;
#16622 = CARTESIAN_POINT ( 'NONE',  ( 9.295050272127047819, 34.50117187608393010, 9.295050272127046043 ) ) ;
#16623 = CARTESIAN_POINT ( 'NONE',  ( 101.7677669529663547, 124.0000000021849615, -1.767766952966370209 ) ) ;
#16624 = CARTESIAN_POINT ( 'NONE',  ( 0.000000000000000000, 40.99999999999999289, 0.000000000000000000 ) ) ;
#16625 = LINE ( 'NONE', #8204, #24461 ) ;
#16626 = CARTESIAN_POINT ( 'NONE',  ( -15.00000000000000000, 75.00000000000000000, 10.00000000000000000 ) ) ;
#16627 = CARTESIAN_POINT ( 'NONE',  ( -9.295050272127044266, 37.47773437608393010, 9.295050272127047819 ) ) ;
#16628 = DIRECTION ( 'NONE',  ( 0.000000000000000000, -0.000000000000000000, 1.000000000000000000 ) ) ;
#16629 = CARTESIAN_POINT ( 'NONE',  ( 102.4999999999999716, 123.0569999999781459, -1.035533905932742638 ) ) ;
#16630 = EDGE_CURVE ( 'NONE', #7460, #17097, #25914, .T. ) ;
#16631 = CARTESIAN_POINT ( 'NONE',  ( 97.93301270000000613, 123.9500000010924765, -9.540979117872439019E-15 ) ) ;
#16632 = CARTESIAN_POINT ( 'NONE',  ( 181.4251840539369596, 39.46210937499999005, 5.622872871577880183 ) ) ;
#16633 = LINE ( 'NONE', #1403, #4049 ) ;
#16634 = CARTESIAN_POINT ( 'NONE',  ( 103.1528011352953342, -3.152801135295355106, 13.81250000136559208 ) ) ;
#16635 = CARTESIAN_POINT ( 'NONE',  ( -5.622872871577873077, 32.11992187499999574, -13.57481594606304753 ) ) ;
#16636 = AXIS2_PLACEMENT_3D ( 'NONE', #18898, #27608, #8066 ) ;
#16637 = VECTOR ( 'NONE', #24248, 999.9999999999998863 ) ;
#16638 = EDGE_LOOP ( 'NONE', ( #5929, #14575, #4574, #13968 ) ) ;
#16639 = CARTESIAN_POINT ( 'NONE',  ( -8.049105076161786076E-16, 32.61601562608393579, -13.14518615778179544 ) ) ;
#16640 = CARTESIAN_POINT ( 'NONE',  ( 9.295050272127046043, 32.31835937608393294, -9.295050272127046043 ) ) ;
#16641 = CARTESIAN_POINT ( 'NONE',  ( -5.622872871577873077, 31.72304687716787441, 13.57481594606304753 ) ) ;
#16642 = DIRECTION ( 'NONE',  ( -0.000000000000000000, -1.000000000000000000, -0.000000000000000000 ) ) ;
#16643 = CARTESIAN_POINT ( 'NONE',  ( 98.15313185440925281, 80.62500000136559208, 4.458734124999987891 ) ) ;
#16644 = CARTESIAN_POINT ( 'NONE',  ( 74.29505027212704249, 37.27929687608394005, -9.295050272127046043 ) ) ;
#16645 = CARTESIAN_POINT ( 'NONE',  ( 95.00472066334982912, 116.8754121666685393, -49.67500000273118843 ) ) ;
#16646 = DIRECTION ( 'NONE',  ( 0.8660254037844407060, 0.4999999999999963363, 0.000000000000000000 ) ) ;
#16647 = DIRECTION ( 'NONE',  ( 0.000000000000000000, -1.000000000000000000, -0.000000000000000000 ) ) ;
#16648 = DIRECTION ( 'NONE',  ( 1.000000000000000000, 0.000000000000000000, -7.228014483236696740E-18 ) ) ;
#16649 = CARTESIAN_POINT ( 'NONE',  ( 93.00000000000000000, 107.7255621263696526, -54.39999999453763024 ) ) ;
#16650 = CARTESIAN_POINT ( 'NONE',  ( 116.8548138422182063, 35.24531250108393721, 5.444914386472304635 ) ) ;
#16651 = EDGE_CURVE ( 'NONE', #1089, #3050, #24640, .T. ) ;
#16652 = ORIENTED_EDGE ( 'NONE', *, *, #12250, .T. ) ;
#16653 = FACE_OUTER_BOUND ( 'NONE', #12899, .T. ) ;
#16654 = CARTESIAN_POINT ( 'NONE',  ( 9.295050272127046043, 40.45429687608393721, -9.295050272127046043 ) ) ;
#16655 = CARTESIAN_POINT ( 'NONE',  ( 13.57481594606304576, 39.11484375216787157, -1.662435489736055892E-15 ) ) ;
#16656 = CARTESIAN_POINT ( 'NONE',  ( 143.1451861577818079, 39.31328125108392868, 5.444914386472293977 ) ) ;
#16657 = ADVANCED_FACE ( 'NONE', ( #16861 ), #13692, .T. ) ;
#16658 = CARTESIAN_POINT ( 'NONE',  ( 78.57481594606304043, 35.98945312716787015, -5.622872871577873077 ) ) ;
#16659 = CARTESIAN_POINT ( 'NONE',  ( 102.4976396683250783, 117.6869444889999841, -52.22499999726882436 ) ) ;
#16660 = CARTESIAN_POINT ( 'NONE',  ( 13.57481594606304576, 38.32109375216786873, -1.662435489736055892E-15 ) ) ;
#16661 = AXIS2_PLACEMENT_3D ( 'NONE', #15042, #19480, #23759 ) ;
#16662 = ORIENTED_EDGE ( 'NONE', *, *, #13926, .F. ) ;
#16663 = EDGE_CURVE ( 'NONE', #18889, #8895, #26077, .T. ) ;
#16664 = CARTESIAN_POINT ( 'NONE',  ( 99.99999999999995737, 5.000000000000018652, 10.75000000000000000 ) ) ;
#16665 = CARTESIAN_POINT ( 'NONE',  ( 95.67376207875072680, 115.9545556584642867, -52.30000000000000426 ) ) ;
#16666 = CARTESIAN_POINT ( 'NONE',  ( -9.295050272127046043, 32.71523437608393436, -9.295050272127046043 ) ) ;
#16667 = CARTESIAN_POINT ( 'NONE',  ( 185.4011555911795313, 31.47500000216787441, -9.598844408820458085 ) ) ;
#16668 = CARTESIAN_POINT ( 'NONE',  ( 0.000000000000000000, 20.00000000000000000, 0.000000000000000000 ) ) ;
#16669 = CARTESIAN_POINT ( 'NONE',  ( 124.5550856135277087, 38.32109375108394289, 13.14518615778179722 ) ) ;
#16670 = CARTESIAN_POINT ( 'NONE',  ( -13.14518615778179189, 32.86406250108393579, 5.444914386472304635 ) ) ;
#16671 = CARTESIAN_POINT ( 'NONE',  ( 2.493653234604083739E-15, 34.05468749999999289, 13.57481594606304576 ) ) ;
#16672 = CYLINDRICAL_SURFACE ( 'NONE', #8758, 13.57481594606304576 ) ;
#16673 = CARTESIAN_POINT ( 'NONE',  ( 98.23223304703363112, 123.2999999999999972, -1.767766952966370209 ) ) ;
#16674 = CARTESIAN_POINT ( 'NONE',  ( 189.3771271284221314, 37.18007812500000853, 13.57481594606304753 ) ) ;
#16675 = CARTESIAN_POINT ( 'NONE',  ( 99.99999999999995737, 85.00000000000000000, -5.000000000000018652 ) ) ;
#16676 = CARTESIAN_POINT ( 'NONE',  ( 95.54126587499996504, 1.387778780781445676E-14, 4.687500001365592084 ) ) ;
#16677 = CARTESIAN_POINT ( 'NONE',  ( 65.00000000000000000, 38.76757812608393294, -13.14518615778179544 ) ) ;
#16678 = CARTESIAN_POINT ( 'NONE',  ( 95.54126587499996504, 1.846868145590750077, 5.375000001365592972 ) ) ;
#16679 = CARTESIAN_POINT ( 'NONE',  ( 104.3262379212492590, 104.0454443415356991, -45.80000000546238681 ) ) ;
#16680 = CARTESIAN_POINT ( 'NONE',  ( 98.15313185440925281, 95.24999999863437949, 4.458734124999979898 ) ) ;
#16681 = CIRCLE ( 'NONE', #2591, 4.999999999999999112 ) ;
#16682 = CARTESIAN_POINT ( 'NONE',  ( 204.5988444088204687, 39.71015624999999716, 9.598844408820456309 ) ) ;
#16683 = LINE ( 'NONE', #3853, #8899 ) ;
#16684 = CARTESIAN_POINT ( 'NONE',  ( 9.598844408820459861, 40.50390624999999289, 9.598844408820456309 ) ) ;
#16685 = ORIENTED_EDGE ( 'NONE', *, *, #22385, .T. ) ;
#16686 = CARTESIAN_POINT ( 'NONE',  ( 103.1528011352953342, 83.31250000136560629, -3.152801135295383084 ) ) ;
#16687 = CARTESIAN_POINT ( 'NONE',  ( 195.0000000000000000, -7.395377635281828788, -13.57481594606306707 ) ) ;
#16688 = ORIENTED_EDGE ( 'NONE', *, *, #23758, .F. ) ;
#16689 = ORIENTED_EDGE ( 'NONE', *, *, #15254, .T. ) ;
#16690 = VECTOR ( 'NONE', #24522, 1000.000000000000000 ) ;
#16691 = CARTESIAN_POINT ( 'NONE',  ( 185.8198241863519229, 49.99999999999996447, -15.00000000000000000 ) ) ;
#16692 = ADVANCED_FACE ( 'NONE', ( #14707 ), #23564, .T. ) ;
#16693 = CARTESIAN_POINT ( 'NONE',  ( 98.15313185440925281, 4.458734125000016313, 8.500000001365592084 ) ) ;
#16694 = ORIENTED_EDGE ( 'NONE', *, *, #21317, .T. ) ;
#16695 = CARTESIAN_POINT ( 'NONE',  ( 91.91746824999999887, 110.0000000000000000, -49.37500000273119838 ) ) ;
#16696 = CARTESIAN_POINT ( 'NONE',  ( -8.049105076161786076E-16, 32.41757812608393863, -13.14518615778179544 ) ) ;
#16697 = AXIS2_PLACEMENT_3D ( 'NONE', #27132, #3316, #221 ) ;
#16698 = CARTESIAN_POINT ( 'NONE',  ( 99.99999999999995737, 85.00000000000000000, -5.000000000000018652 ) ) ;
#16699 = CARTESIAN_POINT ( 'NONE',  ( -5.444914386472299306, 39.90859375108392726, 13.14518615778179722 ) ) ;
#16700 = CARTESIAN_POINT ( 'NONE',  ( 106.5389055433251002, 105.2492070361643215, -50.32500000273120122 ) ) ;
#16701 = AXIS2_PLACEMENT_3D ( 'NONE', #27970, #25678, #8428 ) ;
#16702 = CARTESIAN_POINT ( 'NONE',  ( 143.1451861577818363, 38.71796875108393721, 5.444914386472293977 ) ) ;
#16703 = CARTESIAN_POINT ( 'NONE',  ( 13.14518615778179900, 32.16953125108393152, 5.444914386472293977 ) ) ;
#16704 = VERTEX_POINT ( 'NONE', #10712 ) ;
#16705 = CARTESIAN_POINT ( 'NONE',  ( 55.40115559117954547, 39.31328124999999574, -9.598844408820458085 ) ) ;
#16706 = DIRECTION ( 'NONE',  ( -0.000000000000000000, 1.000000000000000000, -0.000000000000000000 ) ) ;
#16707 = CARTESIAN_POINT ( 'NONE',  ( 78.57481594606305464, 38.27148437500000711, -5.622872871577873966 ) ) ;
#16708 = CARTESIAN_POINT ( 'NONE',  ( 95.54126587499995082, 1.846868145590750077, 2.375000001365592084 ) ) ;
#16709 = CARTESIAN_POINT ( 'NONE',  ( 2.414731522848535132E-15, 32.21914062608393436, 13.14518615778179544 ) ) ;
#16710 = CARTESIAN_POINT ( 'NONE',  ( 103.1528011352953342, -3.152801135295355106, 5.062500001365592972 ) ) ;
#16711 = AXIS2_PLACEMENT_3D ( 'NONE', #26100, #28104, #8568 ) ;
#16712 = CARTESIAN_POINT ( 'NONE',  ( 98.15313185440923860, 83.87500000136560629, 4.458734124999987891 ) ) ;
#16713 = CARTESIAN_POINT ( 'NONE',  ( 2.414731522848535132E-15, 32.81445312608393294, 13.14518615778179544 ) ) ;
#16714 = FACE_OUTER_BOUND ( 'NONE', #17707, .T. ) ;
#16715 = CARTESIAN_POINT ( 'NONE',  ( 185.4011555911795313, 38.51953124999999289, -9.598844408820458085 ) ) ;
#16716 = ORIENTED_EDGE ( 'NONE', *, *, #11191, .T. ) ;
#16717 = LINE ( 'NONE', #19133, #23637 ) ;
#16718 =( BOUNDED_CURVE ( )  B_SPLINE_CURVE ( 2, ( #5554, #24499, #3128, #22798, #999, #24783, #9809, #9668, #18371 ),
 .UNSPECIFIED., .F., .F. ) 
 B_SPLINE_CURVE_WITH_KNOTS ( ( 3, 2, 2, 2, 3 ),
 ( 0.2291666666666665741, 0.2395833333333332316, 0.2499999999999998335, 0.2604166666666665186, 0.2708333333333330928 ),
 .UNSPECIFIED. ) 
 CURVE ( )  GEOMETRIC_REPRESENTATION_ITEM ( )  RATIONAL_B_SPLINE_CURVE ( ( 1.000000000000000666, 0.9238795325112861834, 1.000000000000000000, 0.9238795325112867385, 1.000000000000000000, 0.9238795325112867385, 1.000000000000000000, 0.9238795325112884038, 0.9999999999999983347 ) ) 
 REPRESENTATION_ITEM ( '' )  );
#16719 = CARTESIAN_POINT ( 'NONE',  ( 104.3262379212492448, 104.0454443415356991, -53.79999999453763593 ) ) ;
#16720 = CARTESIAN_POINT ( 'NONE',  ( 104.4587341249999923, 92.62499999863439371, -1.846868145590737198 ) ) ;
#16721 = CARTESIAN_POINT ( 'NONE',  ( 9.598844408820459861, 31.87187500216787228, 9.598844408820456309 ) ) ;
#16722 = CARTESIAN_POINT ( 'NONE',  ( 102.3302406096647843, 122.9999999999999289, -0.7272111440987778508 ) ) ;
#16723 = CARTESIAN_POINT ( 'NONE',  ( 2.493653234604083739E-15, 32.46718749999999432, 13.57481594606304576 ) ) ;
#16724 = ORIENTED_EDGE ( 'NONE', *, *, #8967, .T. ) ;
#16725 = CARTESIAN_POINT ( 'NONE',  ( 65.00000000000000000, 38.17226562608394147, -13.14518615778179544 ) ) ;
#16726 = FACE_OUTER_BOUND ( 'NONE', #11365, .T. ) ;
#16727 = CARTESIAN_POINT ( 'NONE',  ( 9.598844408820459861, 34.94765624999999432, 9.598844408820456309 ) ) ;
#16728 = VERTEX_POINT ( 'NONE', #19285 ) ;
#16729 = CARTESIAN_POINT ( 'NONE',  ( 93.00000000000001421, 112.2744378736303332, -54.10000000000000853 ) ) ;
#16730 = CARTESIAN_POINT ( 'NONE',  ( -7.621963534194025947, 54.91641323977498246, -15.00000000000000000 ) ) ;
#16731 = CARTESIAN_POINT ( 'NONE',  ( -5.622872871577965448, 34.00507812499998295, 13.57481594606295161 ) ) ;
#16732 = CARTESIAN_POINT ( 'NONE',  ( 116.4251840539369596, 33.16171875216787868, 0.000000000000000000 ) ) ;
#16733 = DIRECTION ( 'NONE',  ( 0.000000000000000000, 0.000000000000000000, 1.000000000000000000 ) ) ;
#16734 = CARTESIAN_POINT ( 'NONE',  ( 104.9999999999999716, 1.449011120738813565E-14, 3.625000002731184612 ) ) ;
#16735 = CARTESIAN_POINT ( 'NONE',  ( 204.2950502721270425, 37.87460937608393863, 9.295050272127046043 ) ) ;
#16736 = ORIENTED_EDGE ( 'NONE', *, *, #9081, .T. ) ;
#16737 = ADVANCED_FACE ( 'NONE', ( #23424 ), #2186, .T. ) ;
#16738 =( LENGTH_UNIT ( ) NAMED_UNIT ( * ) SI_UNIT ( .MILLI., .METRE. ) );
#16739 = CARTESIAN_POINT ( 'NONE',  ( 104.4587341249999781, 1.846868145590750521, 13.25000000136559564 ) ) ;
#16740 = CARTESIAN_POINT ( 'NONE',  ( 5.622872871577786924, 38.07304687499999574, 13.57481594606313813 ) ) ;
#16741 = CARTESIAN_POINT ( 'NONE',  ( 94.33688103937537051, 105.8855032339526758, -52.30000000546237970 ) ) ;
#16742 = CARTESIAN_POINT ( 'NONE',  ( 99.99999999999998579, 90.00000000000000000, -6.938893903907228378E-15 ) ) ;
#16743 = CARTESIAN_POINT ( 'NONE',  ( 13.14518615778179722, 39.61093750108393863, -5.444914386472297529 ) ) ;
#16744 = DIRECTION ( 'NONE',  ( 0.000000000000000000, 0.000000000000000000, -1.000000000000000000 ) ) ;
#16745 = CARTESIAN_POINT ( 'NONE',  ( 13.01985494039037050, 36.00000000000000711, 3.369129453356577208 ) ) ;
#16746 = DIRECTION ( 'NONE',  ( -0.000000000000000000, -0.000000000000000000, -1.000000000000000000 ) ) ;
#16747 = CARTESIAN_POINT ( 'NONE',  ( 95.00472066334982912, 103.1245878333314323, -49.32499999726881157 ) ) ;
#16748 = ORIENTED_EDGE ( 'NONE', *, *, #11387, .F. ) ;
#16749 = CARTESIAN_POINT ( 'NONE',  ( 5.622872871577878406, 40.45429687500001137, 13.57481594606304576 ) ) ;
#16750 = CARTESIAN_POINT ( 'NONE',  ( 2.414731522848535132E-15, 39.16445312608392726, 13.14518615778179544 ) ) ;
#16751 = CARTESIAN_POINT ( 'NONE',  ( 104.9999999999999574, -2.071067811865462627, 7.562500002731187720 ) ) ;
#16752 = CARTESIAN_POINT ( 'NONE',  ( 135.4449143864723055, 39.41250000108393436, 13.14518615778179189 ) ) ;
#16753 = CARTESIAN_POINT ( 'NONE',  ( 55.70494972787295751, 35.89023437608393152, 9.295050272127047819 ) ) ;
#16754 =( BOUNDED_CURVE ( )  B_SPLINE_CURVE ( 2, ( #3225, #11892, #19443, #1789, #10308 ),
 .UNSPECIFIED., .F., .F. ) 
 B_SPLINE_CURVE_WITH_KNOTS ( ( 3, 2, 3 ),
 ( 0.7499999999999997780, 0.7916666666666665186, 0.8333333333333333703 ),
 .UNSPECIFIED. ) 
 CURVE ( )  GEOMETRIC_REPRESENTATION_ITEM ( )  RATIONAL_B_SPLINE_CURVE ( ( 1.000000000000000444, 0.9238795325112862944, 1.000000000000000000, 0.9238795325112867385, 1.000000000000000000 ) ) 
 REPRESENTATION_ITEM ( '' )  );
#16755 = CARTESIAN_POINT ( 'NONE',  ( -2.955559473995892819E-15, 1.500000000000001332, -24.13397459621556607 ) ) ;
#16756 = CARTESIAN_POINT ( 'NONE',  ( -9.295050272127046043, 36.48554687608393721, -9.295050272127046043 ) ) ;
#16757 = CARTESIAN_POINT ( 'NONE',  ( 185.1606183911117967, 36.00000000000000711, -9.004033604612759589 ) ) ;
#16758 = CARTESIAN_POINT ( 'NONE',  ( 97.83688103937538472, 116.6573956140660897, -48.40000000000000568 ) ) ;
#16759 = CARTESIAN_POINT ( 'NONE',  ( -15.00000000000000355, 80.00000000000000000, -9.999999999999998224 ) ) ;
#16760 = ORIENTED_EDGE ( 'NONE', *, *, #1510, .F. ) ;
#16761 = LINE ( 'NONE', #25462, #8427 ) ;
#16762 = CARTESIAN_POINT ( 'NONE',  ( -9.295050272127044266, 38.27148437608393294, 9.295050272127047819 ) ) ;
#16763 = CARTESIAN_POINT ( 'NONE',  ( 137.7541239759952703, 36.00000000000000000, 10.77549638133723953 ) ) ;
#16764 = CARTESIAN_POINT ( 'NONE',  ( 99.99999999999998579, 124.0000000000000000, -2.499999999999997780 ) ) ;
#16765 = VECTOR ( 'NONE', #7783, 1000.000000000000000 ) ;
#16766 = CARTESIAN_POINT ( 'NONE',  ( 65.00000000000000000, 40.00781250000000000, -13.57481594606304576 ) ) ;
#16767 = CARTESIAN_POINT ( 'NONE',  ( 97.93301270000000613, 124.7500000010924737, -9.540979117872439019E-15 ) ) ;
#16768 = CARTESIAN_POINT ( 'NONE',  ( 1.662435489736055892E-15, 40.99999999999999289, 13.57481594606304576 ) ) ;
#16769 = CARTESIAN_POINT ( 'NONE',  ( 108.0825317500000153, 110.0000000000000000, -46.37500000273119838 ) ) ;
#16770 = CARTESIAN_POINT ( 'NONE',  ( 104.4587341249999781, 1.846868145590750299, 12.00000000136559208 ) ) ;
#16771 = CARTESIAN_POINT ( 'NONE',  ( -13.57481594606304753, 32.31835937716787299, -5.622872871577872189 ) ) ;
#16772 = ORIENTED_EDGE ( 'NONE', *, *, #2740, .F. ) ;
#16773 = CARTESIAN_POINT ( 'NONE',  ( 101.0355339059327378, 123.7500000021849615, 2.499999999999977796 ) ) ;
#16774 = CARTESIAN_POINT ( 'NONE',  ( 13.57481594606304931, 38.96601562499999005, 5.622872871577869525 ) ) ;
#16775 = CARTESIAN_POINT ( 'NONE',  ( 102.0710678118654329, 5.000000000000018652, 8.687499999999998224 ) ) ;
#16776 = CARTESIAN_POINT ( 'NONE',  ( 2.493653234604083739E-15, 33.36015625216786873, 13.57481594606304576 ) ) ;
#16777 = CARTESIAN_POINT ( 'NONE',  ( 185.4011555911795597, 36.43593750216787441, 9.598844408820459861 ) ) ;
#16778 = CARTESIAN_POINT ( 'NONE',  ( 95.54126587499996504, 80.43750000136559208, -1.387778780781445676E-14 ) ) ;
#16779 = CARTESIAN_POINT ( 'NONE',  ( 51.85481384221819923, 37.52734375108393294, -5.444914386472297529 ) ) ;
#16780 = ADVANCED_FACE ( 'NONE', ( #8585 ), #10846, .F. ) ;
#16781 = CARTESIAN_POINT ( 'NONE',  ( 91.91746824999999887, 110.0000000000000000, -49.37500000273119838 ) ) ;
#16782 = DIRECTION ( 'NONE',  ( 0.000000000000000000, 0.000000000000000000, 1.000000000000000000 ) ) ;
#16783 = CARTESIAN_POINT ( 'NONE',  ( 99.99999999999998579, 123.7500000010924737, -2.066987299999998751 ) ) ;
#16784 = CARTESIAN_POINT ( 'NONE',  ( 51.42518405393695957, 38.66835937716787441, -5.622872871577872189 ) ) ;
#16785 = CARTESIAN_POINT ( 'NONE',  ( 105.6631189606246153, 114.1144967660473242, -53.29999999453764303 ) ) ;
#16786 = CARTESIAN_POINT ( 'NONE',  ( 130.0000000000000000, 32.21914062608393436, 13.14518615778179544 ) ) ;
#16787 = ORIENTED_EDGE ( 'NONE', *, *, #26334, .T. ) ;
#16788 = CARTESIAN_POINT ( 'NONE',  ( 130.0000000000000000, 37.32890625216786873, 13.57481594606304576 ) ) ;
#16789 = CARTESIAN_POINT ( 'NONE',  ( 5.444914386472297529, 40.50390625108394005, -13.14518615778179900 ) ) ;
#16790 = CARTESIAN_POINT ( 'NONE',  ( 95.54126587499995082, 81.50000000136560629, 1.846868145590724986 ) ) ;
#16791 = CARTESIAN_POINT ( 'NONE',  ( 116.8548138422182063, 38.22187500108393010, 5.444914386472304635 ) ) ;
#16792 = CARTESIAN_POINT ( 'NONE',  ( 70.62287287157788285, 36.58476562716787583, 13.57481594606304576 ) ) ;
#16793 = CARTESIAN_POINT ( 'NONE',  ( 102.4976396683250783, 102.3130555110000159, -51.02499999726882152 ) ) ;
#16794 = CIRCLE ( 'NONE', #14037, 5.000000000000000000 ) ;
#16795 = CARTESIAN_POINT ( 'NONE',  ( 13.57481594606304576, 35.14609375216787157, -1.662435489736055892E-15 ) ) ;
#16796 = ORIENTED_EDGE ( 'NONE', *, *, #11414, .T. ) ;
#16797 = CARTESIAN_POINT ( 'NONE',  ( 99.99999999999995737, -4.999999999999990230, 10.24999999999999822 ) ) ;
#16798 = CARTESIAN_POINT ( 'NONE',  ( 104.3262379212492590, 115.9545556584642867, -52.70000000000000284 ) ) ;
#16799 = ADVANCED_FACE ( 'NONE', ( #17417 ), #3898, .T. ) ;
#16800 = CARTESIAN_POINT ( 'NONE',  ( -8.049105076161786076E-16, 34.20351562608394147, -13.14518615778179544 ) ) ;
#16801 = CARTESIAN_POINT ( 'NONE',  ( 189.5550856135277229, 36.43593750108392726, -13.14518615778179900 ) ) ;
#16802 = CARTESIAN_POINT ( 'NONE',  ( 99.99999999999998579, 129.0000000000000000, -5.204170427930421283E-15 ) ) ;
#16803 = CARTESIAN_POINT ( 'NONE',  ( 130.0000000000000000, 37.18007812608393436, -13.14518615778179544 ) ) ;
#16804 = ADVANCED_FACE ( 'NONE', ( #15119 ), #6581, .T. ) ;
#16805 = CARTESIAN_POINT ( 'NONE',  ( 99.99999999999995737, 85.00000000000000000, -5.000000000000018652 ) ) ;
#16806 = CARTESIAN_POINT ( 'NONE',  ( 130.0000000000000000, -7.395377635281828788, -1.503427012513233026E-14 ) ) ;
#16807 = CARTESIAN_POINT ( 'NONE',  ( 104.4587341249999781, 94.31249999863440792, -6.938893903907228378E-15 ) ) ;
#16808 = CARTESIAN_POINT ( 'NONE',  ( -5.444914386472297529, 38.81718750108393579, -13.14518615778179900 ) ) ;
#16809 = ADVANCED_FACE ( 'NONE', ( #4460 ), #19142, .T. ) ;
#16810 = CARTESIAN_POINT ( 'NONE',  ( 204.5988444088204403, 37.52734375000000000, -9.598844408820458085 ) ) ;
#16811 = ITEM_DEFINED_TRANSFORMATION ( 'NONE', 'NONE', #3112,  #26844 ) ;
#16812 = CARTESIAN_POINT ( 'NONE',  ( 99.99999999999995737, 1.387778780781445676E-14, 34.79898987322334136 ) ) ;
#16813 = CARTESIAN_POINT ( 'NONE',  ( 104.4587341249999639, 1.442382525525748735E-14, 1.187500001365592750 ) ) ;
#16814 = CARTESIAN_POINT ( 'NONE',  ( 51.85481384221820633, 39.01562500108393294, 5.444914386472304635 ) ) ;
#16815 = EDGE_CURVE ( 'NONE', #19989, #18417, #2783, .T. ) ;
#16816 = CARTESIAN_POINT ( 'NONE',  ( 99.99999999999995737, -4.458734124999988779, 6.687500001365592084 ) ) ;
#16817 = CARTESIAN_POINT ( 'NONE',  ( 99.99999999999998579, 117.3602355696678501, -49.00000000546238965 ) ) ;
#16818 = CARTESIAN_POINT ( 'NONE',  ( 95.54126587500000767, 90.81249999863440792, -7.484931351350258973E-15 ) ) ;
#16819 = CIRCLE ( 'NONE', #17712, 7.000000000000006217 ) ;
#16820 = CARTESIAN_POINT ( 'NONE',  ( 0.7050241099688876467, 36.00000000000002842, 13.13343125082108820 ) ) ;
#16821 = CARTESIAN_POINT ( 'NONE',  ( -9.598844408820458085, 40.10703124999999147, -9.598844408820458085 ) ) ;
#16822 = CARTESIAN_POINT ( 'NONE',  ( 135.4449143864723055, 40.50390625108394005, -13.14518615778179900 ) ) ;
#16823 = ADVANCED_FACE ( 'NONE', ( #27338 ), #18496, .F. ) ;
#16824 = ORIENTED_EDGE ( 'NONE', *, *, #8435, .F. ) ;
#16825 = CARTESIAN_POINT ( 'NONE',  ( 99.99999999999995737, 82.93750000136560629, 4.458734124999988779 ) ) ;
#16826 = CARTESIAN_POINT ( 'NONE',  ( -5.622872871577873966, 31.42539062716787157, -13.57481594606304753 ) ) ;
#16827 = ORIENTED_EDGE ( 'NONE', *, *, #24638, .F. ) ;
#16828 = EDGE_CURVE ( 'NONE', #18529, #4666, #17066, .T. ) ;
#16829 = ORIENTED_EDGE ( 'NONE', *, *, #15572, .T. ) ;
#16830 = CARTESIAN_POINT ( 'NONE',  ( 128.1124712741236067, 53.66306546785492060, -15.00000000000000178 ) ) ;
#16831 = CARTESIAN_POINT ( 'NONE',  ( 96.84719886470459471, -3.152801135295355994, 5.812500001365591196 ) ) ;
#16832 = ORIENTED_EDGE ( 'NONE', *, *, #5505, .F. ) ;
#16833 = CARTESIAN_POINT ( 'NONE',  ( 93.46109445667491400, 105.2492070361643215, -47.17500000273119554 ) ) ;
#16834 = CARTESIAN_POINT ( 'NONE',  ( -9.295050272127044266, 33.50898437608393010, 9.295050272127047819 ) ) ;
#16835 = CARTESIAN_POINT ( 'NONE',  ( 204.5988444088204403, 37.62656250216787157, -9.598844408820458085 ) ) ;
#16836 = CARTESIAN_POINT ( 'NONE',  ( -13.14518615778179544, 40.55351562608393579, 0.000000000000000000 ) ) ;
#16837 = CARTESIAN_POINT ( 'NONE',  ( 102.4976396683250925, 102.3130555110000159, -46.52500000273119696 ) ) ;
#16838 = CARTESIAN_POINT ( 'NONE',  ( 194.1610731307196147, 53.50081894914376335, 14.99999999999994671 ) ) ;
#16839 = CARTESIAN_POINT ( 'NONE',  ( 135.4449143864723339, 38.12265625108393863, -13.14518615778179722 ) ) ;
#16840 = CARTESIAN_POINT ( 'NONE',  ( 9.295050272127047819, 32.91367187608393152, 9.295050272127046043 ) ) ;
#16841 = ORIENTED_EDGE ( 'NONE', *, *, #571, .F. ) ;
#16842 = CARTESIAN_POINT ( 'NONE',  ( 51.42518405393695957, 39.41249999999999432, 0.000000000000000000 ) ) ;
#16843 = LINE ( 'NONE', #3606, #14122 ) ;
#16844 = CARTESIAN_POINT ( 'NONE',  ( 205.5630829503605810, 36.00000000000001421, 8.196709705856925154 ) ) ;
#16845 = CARTESIAN_POINT ( 'NONE',  ( 96.84719886470459471, -3.152801135295355994, 2.562500001365592084 ) ) ;
#16846 = CARTESIAN_POINT ( 'NONE',  ( 13.14518615778179900, 33.26093750108393721, -5.444914386472297529 ) ) ;
#16847 = CARTESIAN_POINT ( 'NONE',  ( 101.8468681455907046, 4.458734125000016313, 4.375000001365592084 ) ) ;
#16848 = CARTESIAN_POINT ( 'NONE',  ( -9.295050272127044266, 31.92148437608393508, 9.295050272127047819 ) ) ;
#16849 = CARTESIAN_POINT ( 'NONE',  ( -13.14518615778179544, 39.16445312608393436, 0.000000000000000000 ) ) ;
#16850 = EDGE_CURVE ( 'NONE', #13418, #540, #12246, .T. ) ;
#16851 = DIRECTION ( 'NONE',  ( 0.000000000000000000, 1.000000000000000000, 0.000000000000000000 ) ) ;
#16852 = ORIENTED_EDGE ( 'NONE', *, *, #18362, .F. ) ;
#16853 = CARTESIAN_POINT ( 'NONE',  ( 13.14518615778179722, 32.46718750108393436, -5.444914386472297529 ) ) ;
#16854 = DIRECTION ( 'NONE',  ( -5.782411586589357392E-17, -0.000000000000000000, -1.000000000000000000 ) ) ;
#16855 = CARTESIAN_POINT ( 'NONE',  ( 103.1528011352953484, 94.68749999863440792, -3.152801135295366208 ) ) ;
#16856 = CARTESIAN_POINT ( 'NONE',  ( 195.0000000000000000, 36.18789062608393436, 13.14518615778179544 ) ) ;
#16857 = CARTESIAN_POINT ( 'NONE',  ( -13.57481594606304576, 40.20624999999999005, 0.000000000000000000 ) ) ;
#16858 = CARTESIAN_POINT ( 'NONE',  ( -13.57481594606304753, 32.21914062499999432, -5.622872871577872189 ) ) ;
#16859 = ORIENTED_EDGE ( 'NONE', *, *, #9818, .F. ) ;
#16860 = CARTESIAN_POINT ( 'NONE',  ( 74.29505027212704249, 37.08085937608393579, 9.295050272127046043 ) ) ;
#16861 = FACE_OUTER_BOUND ( 'NONE', #13404, .T. ) ;
#16862 = CARTESIAN_POINT ( 'NONE',  ( 116.6399989480775901, 40.87597656304196647, 0.000000000000000000 ) ) ;
#16863 = ORIENTED_EDGE ( 'NONE', *, *, #11904, .F. ) ;
#16864 = CARTESIAN_POINT ( 'NONE',  ( -15.00000000000000355, 55.00000000000000000, -10.00000000000000000 ) ) ;
#16865 = CARTESIAN_POINT ( 'NONE',  ( 116.4251840539369738, 37.87460937499999147, 5.622872871577880183 ) ) ;
#16866 = DIRECTION ( 'NONE',  ( 0.000000000000000000, 0.000000000000000000, 1.000000000000000000 ) ) ;
#16867 = CARTESIAN_POINT ( 'NONE',  ( 130.0000000000000000, 35.34453125216787583, -13.57481594606304576 ) ) ;
#16868 =( BOUNDED_CURVE ( )  B_SPLINE_CURVE ( 2, ( #5439, #9972, #18261, #14107, #3297, #20403, #27387, #25231, #26969, #3432, #7846 ),
 .UNSPECIFIED., .F., .F. ) 
 B_SPLINE_CURVE_WITH_KNOTS ( ( 3, 2, 2, 2, 2, 3 ),
 ( 0.000000000000000000, 0.02000000000000000042, 0.04000000000000000083, 0.05999999999999999778, 0.08000000000000000167, 0.1000000000000000194 ),
 .UNSPECIFIED. ) 
 CURVE ( )  GEOMETRIC_REPRESENTATION_ITEM ( )  RATIONAL_B_SPLINE_CURVE ( ( 1.000000000000000000, 0.9510565162951535312, 1.000000000000000000, 0.9510565162951535312, 1.000000000000000000, 0.9510565162951535312, 1.000000000000000000, 0.9510565162951535312, 1.000000000000000000, 0.9510565162951535312, 1.000000000000000000 ) ) 
 REPRESENTATION_ITEM ( '' )  );
#16869 = CARTESIAN_POINT ( 'NONE',  ( 107.0000000000000142, 110.0000000000000000, -43.50000000546237544 ) ) ;
#16870 = DIRECTION ( 'NONE',  ( 1.000000000000000000, 0.000000000000000000, -5.782411586589357392E-17 ) ) ;
#16871 = MANIFOLD_SOLID_BREP ( 'Cavity1', #26271 ) ;
#16872 = CARTESIAN_POINT ( 'NONE',  ( 181.8548138422181921, 39.21406250108392300, 5.444914386472304635 ) ) ;
#16873 = ORIENTED_EDGE ( 'NONE', *, *, #24827, .F. ) ;
#16874 = ORIENTED_EDGE ( 'NONE', *, *, #9081, .F. ) ;
#16875 =( LENGTH_UNIT ( ) NAMED_UNIT ( * ) SI_UNIT ( .MILLI., .METRE. ) );
#16876 = CARTESIAN_POINT ( 'NONE',  ( 99.99999999999995737, 83.75000000000000000, -5.000000000000018652 ) ) ;
#16877 = CARTESIAN_POINT ( 'NONE',  ( 99.99999999999998579, 102.6397644303321215, -52.00000000546236834 ) ) ;
#16878 = DIRECTION ( 'NONE',  ( -0.000000000000000000, 1.000000000000000000, -0.000000000000000000 ) ) ;
#16879 = CARTESIAN_POINT ( 'NONE',  ( 130.0000000000000000, 39.71015625216787015, 13.57481594606304576 ) ) ;
#16880 = FACE_OUTER_BOUND ( 'NONE', #18320, .T. ) ;
#16881 = DIRECTION ( 'NONE',  ( -1.000000000000000000, 0.000000000000000000, 5.782411586589357392E-17 ) ) ;
#16882 = CARTESIAN_POINT ( 'NONE',  ( 120.4011555911795455, 32.16953124999999147, -9.598844408820458085 ) ) ;
#16883 = ORIENTED_EDGE ( 'NONE', *, *, #9667, .F. ) ;
#16884 = CARTESIAN_POINT ( 'NONE',  ( -8.312177448680279460E-16, 39.21406249999999716, -13.57481594606304576 ) ) ;
#16885 = CARTESIAN_POINT ( 'NONE',  ( -13.57481594606304576, 32.41757812716787157, 5.622872871577880183 ) ) ;
#16886 = CARTESIAN_POINT ( 'NONE',  ( 99.99999999999995737, 5.000000000000018652, 2.875000002731185944 ) ) ;
#16887 = CARTESIAN_POINT ( 'NONE',  ( 143.1451861577818079, 38.71796875108393721, 5.444914386472293977 ) ) ;
#16888 = CARTESIAN_POINT ( 'NONE',  ( 70.44491438647230552, 37.13046875108393152, -13.14518615778179900 ) ) ;
#16889 = CARTESIAN_POINT ( 'NONE',  ( 200.4449143864723055, 32.07031250108393294, 13.14518615778179189 ) ) ;
#16890 = ORIENTED_EDGE ( 'NONE', *, *, #23765, .T. ) ;
#16891 = CARTESIAN_POINT ( 'NONE',  ( 130.0000000000000000, 40.40468749999999432, 13.57481594606304576 ) ) ;
#16892 = CARTESIAN_POINT ( 'NONE',  ( -8.049105076161786076E-16, 35.59257812608393579, -13.14518615778179544 ) ) ;
#16893 = CARTESIAN_POINT ( 'NONE',  ( 198.6286142932848691, 36.00000000000000000, -13.08307257738122686 ) ) ;
#16894 = DIRECTION ( 'NONE',  ( -1.000000000000000000, 0.000000000000000000, 0.000000000000000000 ) ) ;
#16895 = FACE_OUTER_BOUND ( 'NONE', #14997, .T. ) ;
#16896 = CARTESIAN_POINT ( 'NONE',  ( -13.14518615778179900, 37.32890625108393579, -5.444914386472297529 ) ) ;
#16897 = CARTESIAN_POINT ( 'NONE',  ( 99.99999999999998579, 124.0000000000000000, -2.499999999999997780 ) ) ;
#16898 = CARTESIAN_POINT ( 'NONE',  ( 98.23223304703363112, 124.8999999999999915, -1.767766952966370209 ) ) ;
#16899 = CARTESIAN_POINT ( 'NONE',  ( 102.0669872999999939, 124.3000000010924566, 0.8561741729129311862 ) ) ;
#16900 = CARTESIAN_POINT ( 'NONE',  ( 100.8561741729129437, 124.2000000010924623, 2.066987299999979655 ) ) ;
#16901 =( NAMED_UNIT ( * ) PLANE_ANGLE_UNIT ( ) SI_UNIT ( $, .RADIAN. ) );
#16902 = CARTESIAN_POINT ( 'NONE',  ( 104.4587341249999781, 1.846868145590750299, 11.00000000136559208 ) ) ;
#16903 = CARTESIAN_POINT ( 'NONE',  ( 104.9999999999999574, -2.071067811865468844, 13.56250000273118417 ) ) ;
#16904 = VERTEX_POINT ( 'NONE', #23192 ) ;
#16905 = CARTESIAN_POINT ( 'NONE',  ( 97.83688103937537051, 103.3426043859339103, -53.60000000000000853 ) ) ;
#16906 = CARTESIAN_POINT ( 'NONE',  ( -9.295050272127046043, 31.92148437608393508, -9.295050272127046043 ) ) ;
#16907 = CARTESIAN_POINT ( 'NONE',  ( 13.14518615778179544, 33.01289062608393010, -1.609821015232357215E-15 ) ) ;
#16908 = CARTESIAN_POINT ( 'NONE',  ( -5.622872871577873077, 34.10429687716786873, 13.57481594606304753 ) ) ;
#16909 = CARTESIAN_POINT ( 'NONE',  ( 94.99999999999995737, 1.387778780781445676E-14, 3.125000002731185944 ) ) ;
#16910 = CARTESIAN_POINT ( 'NONE',  ( 98.15313185440925281, 83.87500000136560629, 4.458734124999987891 ) ) ;
#16911 = CARTESIAN_POINT ( 'NONE',  ( 59.55508561352770158, 38.51953125108393294, 13.14518615778179722 ) ) ;
#16912 = CARTESIAN_POINT ( 'NONE',  ( 108.0825317500000011, 112.6261737610028320, -46.27500000273120406 ) ) ;
#16913 = FACE_OUTER_BOUND ( 'NONE', #26238, .T. ) ;
#16914 = CARTESIAN_POINT ( 'NONE',  ( 102.0669872999999797, 122.7500000010924737, -9.794112055954760458E-15 ) ) ;
#16915 = CARTESIAN_POINT ( 'NONE',  ( 139.5988444088204687, 38.91640624999999432, 9.598844408820456309 ) ) ;
#16916 = CARTESIAN_POINT ( 'NONE',  ( 95.67376207875069838, 104.0454443415356991, -54.19999999453764161 ) ) ;
#16917 = CARTESIAN_POINT ( 'NONE',  ( 135.6228728715778686, 39.16445312499999432, -13.57481594606304753 ) ) ;
#16918 = VERTEX_POINT ( 'NONE', #1257 ) ;
#16919 = CARTESIAN_POINT ( 'NONE',  ( 99.99999999999998579, 92.62499999726881583, 4.999999999999984013 ) ) ;
#16920 =( BOUNDED_CURVE ( )  B_SPLINE_CURVE ( 2, ( #28047, #6241, #13181, #21920, #28184, #17343, #25904, #22055, #21488, #1969, #12900 ),
 .UNSPECIFIED., .F., .F. ) 
 B_SPLINE_CURVE_WITH_KNOTS ( ( 3, 2, 2, 2, 2, 3 ),
 ( 0.9000000000000000222, 0.9200000000000000400, 0.9399999999999999467, 0.9599999999999999645, 0.9799999999999999822, 1.000000000000000000 ),
 .UNSPECIFIED. ) 
 CURVE ( )  GEOMETRIC_REPRESENTATION_ITEM ( )  RATIONAL_B_SPLINE_CURVE ( ( 1.000000000000000000, 0.9510565162951535312, 1.000000000000000000, 0.9510565162951535312, 1.000000000000000000, 0.9510565162951535312, 1.000000000000000000, 0.9510565162951535312, 1.000000000000000000, 0.9510565162951535312, 1.000000000000000000 ) ) 
 REPRESENTATION_ITEM ( '' )  );
#16921 = CARTESIAN_POINT ( 'NONE',  ( 13.14518615778179900, 38.71796875108393721, 5.444914386472293977 ) ) ;
#16922 = CARTESIAN_POINT ( 'NONE',  ( -13.57481594606304753, 40.25585937716787299, -5.622872871577873077 ) ) ;
#16923 = CARTESIAN_POINT ( 'NONE',  ( 116.8548138422182205, 40.55351562608393579, 0.000000000000000000 ) ) ;
#16924 = CARTESIAN_POINT ( 'NONE',  ( 78.57481594606305464, 36.73359375216787015, -1.662435489736055892E-15 ) ) ;
#16925 = EDGE_CURVE ( 'NONE', #27294, #22247, #20913, .T. ) ;
#16926 = FACE_OUTER_BOUND ( 'NONE', #1520, .T. ) ;
#16927 = CARTESIAN_POINT ( 'NONE',  ( -9.598844408820454532, 34.84843750216787583, 9.598844408820459861 ) ) ;
#16928 = ORIENTED_EDGE ( 'NONE', *, *, #6682, .T. ) ;
#16929 = CARTESIAN_POINT ( 'NONE',  ( 104.9999999999999574, 2.071067811865491937, 5.562500000000000000 ) ) ;
#16930 = CARTESIAN_POINT ( 'NONE',  ( 204.2950502721270425, 36.08867187608392868, 9.295050272127046043 ) ) ;
#16931 = DIRECTION ( 'NONE',  ( 0.000000000000000000, 0.000000000000000000, 1.000000000000000000 ) ) ;
#16932 = CARTESIAN_POINT ( 'NONE',  ( 124.5550856135277087, 39.11484375108393863, 13.14518615778179722 ) ) ;
#16933 = DIRECTION ( 'NONE',  ( 5.782411586589358625E-17, -0.000000000000000000, 1.000000000000000000 ) ) ;
#16934 = CARTESIAN_POINT ( 'NONE',  ( 96.46446609406721961, -3.535533905932727539, 11.12500000000000000 ) ) ;
#16935 = CARTESIAN_POINT ( 'NONE',  ( 98.15313185440923860, 94.99999999863439371, 4.458734124999980786 ) ) ;
#16936 = CARTESIAN_POINT ( 'NONE',  ( 195.0000000000000000, 52.00000000000000711, -2.255140518769849538E-14 ) ) ;
#16937 = CARTESIAN_POINT ( 'NONE',  ( 2.414731522848535132E-15, 38.37070312608393152, 13.14518615778179544 ) ) ;
#16938 = CARTESIAN_POINT ( 'NONE',  ( 181.4251840539369596, 37.03124999999999289, 0.000000000000000000 ) ) ;
#16939 = CARTESIAN_POINT ( 'NONE',  ( 102.0710678118654329, -4.999999999999989342, 8.437500002731185944 ) ) ;
#16940 = CARTESIAN_POINT ( 'NONE',  ( 96.84719886470459471, -3.152801135295355994, 2.812500001365592528 ) ) ;
#16941 = CARTESIAN_POINT ( 'NONE',  ( 78.14518615778179367, 37.82500000108392868, -5.444914386472297529 ) ) ;
#16942 = CARTESIAN_POINT ( 'NONE',  ( 98.15313185440923860, -4.458734124999987891, 7.625000001365592084 ) ) ;
#16943 = CARTESIAN_POINT ( 'NONE',  ( 109.0000000000000142, 110.0000000000000000, -55.00000000000000711 ) ) ;
#16944 = CARTESIAN_POINT ( 'NONE',  ( 104.4587341249999923, 94.49999999863442213, 1.846868145590726318 ) ) ;
#16945 = CARTESIAN_POINT ( 'NONE',  ( -12.83975123685816833, 36.00000000000000000, 2.850296047819892209 ) ) ;
#16946 = CARTESIAN_POINT ( 'NONE',  ( -5.622872871577873077, 38.76757812500000000, 13.57481594606304753 ) ) ;
#16947 = CARTESIAN_POINT ( 'NONE',  ( 124.5550856135277087, 39.80937500108392868, -13.14518615778179900 ) ) ;
#16948 = ORIENTED_EDGE ( 'NONE', *, *, #1313, .F. ) ;
#16949 = CARTESIAN_POINT ( 'NONE',  ( 104.4587341249999639, 82.18750000136559208, -1.442382525525748735E-14 ) ) ;
#16950 = EDGE_CURVE ( 'NONE', #23060, #10301, #12518, .T. ) ;
#16951 = CARTESIAN_POINT ( 'NONE',  ( 104.4587341249999923, 90.37499999863440792, -1.846868145590737198 ) ) ;
#16952 = ORIENTED_EDGE ( 'NONE', *, *, #14397, .T. ) ;
#16953 = VECTOR ( 'NONE', #16063, 999.9999999999998863 ) ;
#16954 = DIRECTION ( 'NONE',  ( 1.000000000000000000, 0.000000000000000000, -7.228014483236696740E-18 ) ) ;
#16955 = CARTESIAN_POINT ( 'NONE',  ( 59.55508561352770158, 35.34453125108393579, 13.14518615778179722 ) ) ;
#16956 = EDGE_LOOP ( 'NONE', ( #25172, #21256, #16444, #16824 ) ) ;
#16957 = ADVANCED_FACE ( 'NONE', ( #1535 ), #10187, .T. ) ;
#16958 = CARTESIAN_POINT ( 'NONE',  ( 91.91746824999998466, 110.0000000000000000, -55.62499999726882294 ) ) ;
#16959 = CARTESIAN_POINT ( 'NONE',  ( 103.1528011352953342, -3.152801135295355106, 6.062500001365592084 ) ) ;
#16960 = EDGE_CURVE ( 'NONE', #10089, #12843, #16761, .T. ) ;
#16961 = ORIENTED_EDGE ( 'NONE', *, *, #22061, .F. ) ;
#16962 = CARTESIAN_POINT ( 'NONE',  ( 5.444914386472302859, 35.44375000108393436, 13.14518615778179189 ) ) ;
#16963 = CARTESIAN_POINT ( 'NONE',  ( -5.444914386472297529, 32.46718750108393436, -13.14518615778179900 ) ) ;
#16964 = CARTESIAN_POINT ( 'NONE',  ( 204.5988444088204687, 36.63437500216787157, 9.598844408820456309 ) ) ;
#16965 = CARTESIAN_POINT ( 'NONE',  ( 13.14518615778179722, 39.41250000108393436, -5.444914386472297529 ) ) ;
#16966 = EDGE_CURVE ( 'NONE', #13215, #12839, #5941, .T. ) ;
#16967 = DIRECTION ( 'NONE',  ( 1.000000000000000000, -0.000000000000000000, -5.782411586589357392E-17 ) ) ;
#16968 = CARTESIAN_POINT ( 'NONE',  ( 204.1801758136480203, 50.00000000000000000, 9.999999999999946709 ) ) ;
#16969 = CARTESIAN_POINT ( 'NONE',  ( 143.1451861577818079, 39.56132812608393579, -1.609821015232357215E-15 ) ) ;
#16970 = CARTESIAN_POINT ( 'NONE',  ( 5.444914386472302859, 38.61875000108393152, 13.14518615778179189 ) ) ;
#16971 = ORIENTED_EDGE ( 'NONE', *, *, #26189, .T. ) ;
#16972 = CARTESIAN_POINT ( 'NONE',  ( 65.00000000000000000, 36.83281249999999574, -13.57481594606304576 ) ) ;
#16973 = CARTESIAN_POINT ( 'NONE',  ( 99.99999999999995737, 79.87500000273119838, -5.000000000000018652 ) ) ;
#16974 = EDGE_CURVE ( 'NONE', #25528, #11744, #21996, .T. ) ;
#16975 = CARTESIAN_POINT ( 'NONE',  ( 91.91746824999998466, 110.0000000000000000, -45.62499999726882294 ) ) ;
#16976 = CARTESIAN_POINT ( 'NONE',  ( 99.99999999999995737, -4.458734124999988779, 4.687500001365592084 ) ) ;
#16977 = CARTESIAN_POINT ( 'NONE',  ( 103.5355339059327093, 3.535533905932755072, 3.750000002731185056 ) ) ;
#16978 =( REPRESENTATION_RELATIONSHIP ('NONE','NONE', #2411, #9145 ) REPRESENTATION_RELATIONSHIP_WITH_TRANSFORMATION ( #11217 )SHAPE_REPRESENTATION_RELATIONSHIP( ) );
#16979 = CARTESIAN_POINT ( 'NONE',  ( 96.84719886470459471, -3.152801135295355994, 2.812500001365592528 ) ) ;
#16980 = CARTESIAN_POINT ( 'NONE',  ( 95.54126587499996504, 79.68750000136559208, -1.387778780781445676E-14 ) ) ;
#16981 = CARTESIAN_POINT ( 'NONE',  ( -9.295050272127046043, 31.72304687608393081, -9.295050272127046043 ) ) ;
#16982 = CARTESIAN_POINT ( 'NONE',  ( -5.444914386472297529, 38.22187500108393010, -13.14518615778179900 ) ) ;
#16983 = CARTESIAN_POINT ( 'NONE',  ( 91.91746824999998466, 110.0000000000000000, -45.87499999726882294 ) ) ;
#16984 = ORIENTED_EDGE ( 'NONE', *, *, #17353, .T. ) ;
#16985 = DIRECTION ( 'NONE',  ( 1.000000000000000000, 0.000000000000000000, -0.000000000000000000 ) ) ;
#16986 = CARTESIAN_POINT ( 'NONE',  ( 104.9999999999999716, 83.62500000273119838, -1.449011120738813565E-14 ) ) ;
#16987 = CARTESIAN_POINT ( 'NONE',  ( 108.0825317500000011, 110.0000000000000000, -54.87499999726882294 ) ) ;
#16988 = EDGE_CURVE ( 'NONE', #18589, #1781, #13702, .T. ) ;
#16989 = CARTESIAN_POINT ( 'NONE',  ( 94.99999999999995737, -2.071067811865466624, 6.187500002731185056 ) ) ;
#16990 = EDGE_LOOP ( 'NONE', ( #25558, #19140, #22656, #11934 ) ) ;
#16991 = CARTESIAN_POINT ( 'NONE',  ( 78.14518615778179367, 38.76757812608393294, -1.609821015232357215E-15 ) ) ;
#16992 = CARTESIAN_POINT ( 'NONE',  ( 99.99999999999997158, 102.6397644303321215, -54.50000000000000711 ) ) ;
#16993 = CARTESIAN_POINT ( 'NONE',  ( -13.57481594606304398, 39.46210937499999005, 5.622872871577880183 ) ) ;
#16994 = AXIS2_PLACEMENT_3D ( 'NONE', #26051, #2267, #10927 ) ;
#16995 = ORIENTED_EDGE ( 'NONE', *, *, #19102, .T. ) ;
#16996 = CARTESIAN_POINT ( 'NONE',  ( 93.00000000000001421, 107.7255621263696668, -47.89999999999999858 ) ) ;
#16997 = PLANE ( 'NONE',  #4248 ) ;
#16998 = CARTESIAN_POINT ( 'NONE',  ( 99.99999999999998579, 93.12499999726881583, -4.999999999999997335 ) ) ;
#16999 = ADVANCED_FACE ( 'NONE', ( #15271 ), #13410, .T. ) ;
#17000 = CARTESIAN_POINT ( 'NONE',  ( 120.4011555911795455, 34.84843750216787583, 9.598844408820459861 ) ) ;
#17001 = CARTESIAN_POINT ( 'NONE',  ( 204.2950502721270425, 35.49335937608393721, 9.295050272127046043 ) ) ;
#17002 = VERTEX_POINT ( 'NONE', #6731 ) ;
#17003 = ORIENTED_EDGE ( 'NONE', *, *, #23995, .F. ) ;
#17004 = ORIENTED_EDGE ( 'NONE', *, *, #16950, .F. ) ;
#17005 = CARTESIAN_POINT ( 'NONE',  ( 5.444914386472297529, 33.16171875108393152, -13.14518615778179900 ) ) ;
#17006 = CARTESIAN_POINT ( 'NONE',  ( 99.99999999999995737, -4.458734124999988779, 13.93750000136559208 ) ) ;
#17007 = CARTESIAN_POINT ( 'NONE',  ( 9.598844408820459861, 33.45937500216787441, 9.598844408820456309 ) ) ;
#17008 = CARTESIAN_POINT ( 'NONE',  ( 98.15313185440923860, 83.62500000136560629, 4.458734124999987891 ) ) ;
#17009 = DIRECTION ( 'NONE',  ( -0.000000000000000000, 1.000000000000000000, -0.000000000000000000 ) ) ;
#17010 = CARTESIAN_POINT ( 'NONE',  ( 102.4999205310587058, 123.0000000000000000, 0.3311205932291627629 ) ) ;
#17011 = CARTESIAN_POINT ( 'NONE',  ( 104.7293670624999748, 95.15624999931721106, -6.938893903907228378E-15 ) ) ;
#17012 = CARTESIAN_POINT ( 'NONE',  ( 8.193155644909767332, 36.00000000000001421, 10.45682415286414546 ) ) ;
#17013 = CARTESIAN_POINT ( 'NONE',  ( 8.754898953241641024, 50.00000000000000000, 10.39041163855821637 ) ) ;
#17014 = CARTESIAN_POINT ( 'NONE',  ( 116.4251840539369596, 32.31835937499999289, 5.622872871577880183 ) ) ;
#17015 = ORIENTED_EDGE ( 'NONE', *, *, #1653, .T. ) ;
#17016 = AXIS2_PLACEMENT_3D ( 'NONE', #2039, #9009, #11122 ) ;
#17017 = CARTESIAN_POINT ( 'NONE',  ( 13.57481594606304753, 39.06523437499998863, -5.622872871577873077 ) ) ;
#17018 = CARTESIAN_POINT ( 'NONE',  ( -9.598844408820454532, 31.67343750216787512, 9.598844408820459861 ) ) ;
#17019 = CARTESIAN_POINT ( 'NONE',  ( 97.92893218813451028, 5.000000000000018652, 0.9375000027311859441 ) ) ;
#17020 = CARTESIAN_POINT ( 'NONE',  ( 143.1451861577818079, 35.64218750108393152, -5.444914386472297529 ) ) ;
#17021 = CARTESIAN_POINT ( 'NONE',  ( 65.00000000000000000, 36.78320312608393294, 13.14518615778179544 ) ) ;
#17022 = EDGE_CURVE ( 'NONE', #21964, #24113, #26662, .T. ) ;
#17023 = CARTESIAN_POINT ( 'NONE',  ( 181.8548138422181921, 32.66562500108393863, 5.444914386472304635 ) ) ;
#17024 = CARTESIAN_POINT ( 'NONE',  ( 55.28645250595090488, 35.99999999999999289, 8.898183052316495534 ) ) ;
#17025 = CARTESIAN_POINT ( 'NONE',  ( -9.295050272127046043, 34.89804687608393152, -9.295050272127046043 ) ) ;
#17026 =( BOUNDED_SURFACE ( )  B_SPLINE_SURFACE ( 1, 2, ( 
 ( #21454, #12444, #8329, #12313, #1380, #23314, #3649, #7914, #1651, #6064, #28008, #14730, #27591, #23449, #21309, #10171, #23584, #12862, #25717, #6200, #12730, #1932, #10600, #8472, #21034, #17159, #25861, #6333, #15007, #23729, #10041, #18753, #27453, #16609, #25303, #5790, #8051, #16747, #25447, #5928, #14595, #3786, #6749, #19867, #6472, #10877, #17299, #15579, #6893, #11010, #19723, #8751, #4916, #4343, #12999, #24009, #4767, #9179, #21879, #8894, #24427, #2490, #21591, #4626, #26141, #209, #19446, #13143, #26001, #17872, #28144, #13429, #17442, #2067, #10737, #17584, #26289, #19586, #21738, #22157, #498, #4486, #11295, #15435, #22013, #15146, #8612, #24149, #2355, #26434, #13283, #24286, #11151, #23864, #2212, #2635, #69, #20018, #353, #9038, #26577 ),
 ( #7026, #15724, #15292, #17732, #6607, #7167, #11439, #3335, #1071, #22442, #1213, #5339, #14148, #9879, #18585, #27155, #7607, #24574, #22586, #16298, #15864, #3054, #928, #18011, #24999, #22867, #5055, #9740, #5478, #13720, #12005, #18448, #13860, #20729, #27291, #7747, #16435, #18155, #25132, #14005, #13576, #22300, #18301, #5196, #20159, #2775, #640, #9599, #9313, #26721, #11865, #2909, #11578, #24718, #20298, #7456, #785, #9455, #11721, #26869, #20447, #7315, #27009, #16004, #16150, #24858, #22728, #3194, #20588, #10429, #27978, #18993, #4037, #3759, #1487, #10571, #21281, #14428, #10014, #20866, #19137, #8437, #12421, #12555, #10284, #19280, #27843, #8299, #16577, #14570, #16987, #27421, #23285, #21139, #18723, #25687, #14837, #7884, #1764, #6170, #25270 ) ),
 .UNSPECIFIED., .F., .F., .T. ) 
 B_SPLINE_SURFACE_WITH_KNOTS ( ( 2, 2 ),
 ( 3, 2, 2, 2, 2, 2, 2, 2, 2, 2, 2, 2, 2, 2, 2, 2, 2, 2, 2, 2, 2, 2, 2, 2, 2, 2, 2, 2, 2, 2, 2, 2, 2, 2, 2, 2, 2, 2, 2, 2, 2, 2, 2, 2, 2, 2, 2, 2, 2, 2, 3 ),
 ( 0.000000000000000000, 1.000000000000000000 ),
 ( 0.000000000000000000, 0.02000000000000000042, 0.04000000000000000083, 0.05999999999999999778, 0.08000000000000000167, 0.1000000000000000056, 0.1199999999999999956, 0.1400000000000000133, 0.1600000000000000033, 0.1799999999999999933, 0.2000000000000000111, 0.2200000000000000011, 0.2399999999999999911, 0.2600000000000000089, 0.2800000000000000266, 0.2999999999999999889, 0.3200000000000000067, 0.3400000000000000244, 0.3599999999999999867, 0.3800000000000000044, 0.4000000000000000222, 0.4199999999999999845, 0.4400000000000000022, 0.4600000000000000200, 0.4799999999999999822, 0.5000000000000000000, 0.5200000000000000178, 0.5400000000000000355, 0.5600000000000000533, 0.5799999999999999600, 0.5999999999999999778, 0.6199999999999999956, 0.6400000000000000133, 0.6600000000000000311, 0.6800000000000000488, 0.6999999999999999556, 0.7199999999999999734, 0.7399999999999999911, 0.7600000000000000089, 0.7800000000000000266, 0.8000000000000000444, 0.8199999999999999512, 0.8399999999999999689, 0.8599999999999999867, 0.8800000000000000044, 0.9000000000000000222, 0.9200000000000000400, 0.9399999999999999467, 0.9599999999999999645, 0.9799999999999999822, 1.000000000000000000 ),
 .UNSPECIFIED. ) 
 GEOMETRIC_REPRESENTATION_ITEM ( )  RATIONAL_B_SPLINE_SURFACE ( (
 ( 1.000000000000000000, 0.9510565162951535312, 1.000000000000000000, 0.9510565162951535312, 1.000000000000000000, 0.9510565162951535312, 1.000000000000000000, 0.9510565162951535312, 1.000000000000000000, 0.9510565162951535312, 1.000000000000000000, 0.9510565162951535312, 1.000000000000000000, 0.9510565162951535312, 1.000000000000000000, 0.9510565162951535312, 1.000000000000000000, 0.9510565162951535312, 1.000000000000000000, 0.9510565162951535312, 1.000000000000000000, 0.9510565162951535312, 1.000000000000000000, 0.9510565162951535312, 1.000000000000000000, 0.9510565162951535312, 1.000000000000000000, 0.9510565162951535312, 1.000000000000000000, 0.9510565162951535312, 1.000000000000000000, 0.9510565162951535312, 1.000000000000000000, 0.9510565162951535312, 1.000000000000000000, 0.9510565162951535312, 1.000000000000000000, 0.9510565162951535312, 1.000000000000000000, 0.9510565162951535312, 1.000000000000000000, 0.9510565162951535312, 1.000000000000000000, 0.9510565162951535312, 1.000000000000000000, 0.9510565162951535312, 1.000000000000000000, 0.9510565162951535312, 1.000000000000000000, 0.9510565162951535312, 1.000000000000000000, 0.9510565162951535312, 1.000000000000000000, 0.9510565162951535312, 1.000000000000000000, 0.9510565162951535312, 1.000000000000000000, 0.9510565162951535312, 1.000000000000000000, 0.9510565162951535312, 1.000000000000000000, 0.9510565162951535312, 1.000000000000000000, 0.9510565162951535312, 1.000000000000000000, 0.9510565162951535312, 1.000000000000000000, 0.9510565162951535312, 1.000000000000000000, 0.9510565162951535312, 1.000000000000000000, 0.9510565162951535312, 1.000000000000000000, 0.9510565162951535312, 1.000000000000000000, 0.9510565162951535312, 1.000000000000000000, 0.9510565162951535312, 1.000000000000000000, 0.9510565162951535312, 1.000000000000000000, 0.9510565162951535312, 1.000000000000000000, 0.9510565162951535312, 1.000000000000000000, 0.9510565162951535312, 1.000000000000000000, 0.9510565162951535312, 1.000000000000000000, 0.9510565162951535312, 1.000000000000000000, 0.9510565162951535312, 1.000000000000000000, 0.9510565162951535312, 1.000000000000000000, 0.9510565162951535312, 1.000000000000000000, 0.9510565162951535312, 1.000000000000000000, 0.9510565162951535312, 1.000000000000000000),
 ( 1.000000000000000000, 0.9510565162951535312, 1.000000000000000000, 0.9510565162951535312, 1.000000000000000000, 0.9510565162951535312, 1.000000000000000000, 0.9510565162951535312, 1.000000000000000000, 0.9510565162951535312, 1.000000000000000000, 0.9510565162951535312, 1.000000000000000000, 0.9510565162951535312, 1.000000000000000000, 0.9510565162951535312, 1.000000000000000000, 0.9510565162951535312, 1.000000000000000000, 0.9510565162951535312, 1.000000000000000000, 0.9510565162951535312, 1.000000000000000000, 0.9510565162951535312, 1.000000000000000000, 0.9510565162951535312, 1.000000000000000000, 0.9510565162951535312, 1.000000000000000000, 0.9510565162951535312, 1.000000000000000000, 0.9510565162951535312, 1.000000000000000000, 0.9510565162951535312, 1.000000000000000000, 0.9510565162951535312, 1.000000000000000000, 0.9510565162951535312, 1.000000000000000000, 0.9510565162951535312, 1.000000000000000000, 0.9510565162951535312, 1.000000000000000000, 0.9510565162951535312, 1.000000000000000000, 0.9510565162951535312, 1.000000000000000000, 0.9510565162951535312, 1.000000000000000000, 0.9510565162951535312, 1.000000000000000000, 0.9510565162951535312, 1.000000000000000000, 0.9510565162951535312, 1.000000000000000000, 0.9510565162951535312, 1.000000000000000000, 0.9510565162951535312, 1.000000000000000000, 0.9510565162951535312, 1.000000000000000000, 0.9510565162951535312, 1.000000000000000000, 0.9510565162951535312, 1.000000000000000000, 0.9510565162951535312, 1.000000000000000000, 0.9510565162951535312, 1.000000000000000000, 0.9510565162951535312, 1.000000000000000000, 0.9510565162951535312, 1.000000000000000000, 0.9510565162951535312, 1.000000000000000000, 0.9510565162951535312, 1.000000000000000000, 0.9510565162951535312, 1.000000000000000000, 0.9510565162951535312, 1.000000000000000000, 0.9510565162951535312, 1.000000000000000000, 0.9510565162951535312, 1.000000000000000000, 0.9510565162951535312, 1.000000000000000000, 0.9510565162951535312, 1.000000000000000000, 0.9510565162951535312, 1.000000000000000000, 0.9510565162951535312, 1.000000000000000000, 0.9510565162951535312, 1.000000000000000000, 0.9510565162951535312, 1.000000000000000000, 0.9510565162951535312, 1.000000000000000000, 0.9510565162951535312, 1.000000000000000000) ) ) 
 REPRESENTATION_ITEM ( '' )  SURFACE ( )  );
#17027 = CARTESIAN_POINT ( 'NONE',  ( 123.5871333237427905, 50.00000000108524034, -11.99502265407588730 ) ) ;
#17028 = CARTESIAN_POINT ( 'NONE',  ( 94.99999999999995737, 1.387778780781445676E-14, 5.999999999999998224 ) ) ;
#17029 = CARTESIAN_POINT ( 'NONE',  ( 98.23223304703363112, 124.8999999999999915, -1.767766952966370209 ) ) ;
#17030 = CARTESIAN_POINT ( 'NONE',  ( -13.14518615778179544, 39.75976562608393294, 0.000000000000000000 ) ) ;
#17031 = CARTESIAN_POINT ( 'NONE',  ( 99.99999999999998579, 90.00000000000000000, 4.999999999999983125 ) ) ;
#17032 = CARTESIAN_POINT ( 'NONE',  ( 97.50000000000000000, 125.0092387953251034, 0.1913417161825344548 ) ) ;
#17033 = CARTESIAN_POINT ( 'NONE',  ( 102.0669872999999939, 123.6000000010924680, -0.8561741729129507261 ) ) ;
#17034 = CARTESIAN_POINT ( 'NONE',  ( 102.0669872999999797, 124.3500000010924822, -9.794112055954760458E-15 ) ) ;
#17035 = CIRCLE ( 'NONE', #8400, 19.22649730810373470 ) ;
#17036 =( NAMED_UNIT ( * ) PLANE_ANGLE_UNIT ( ) SI_UNIT ( $, .RADIAN. ) );
#17037 = CARTESIAN_POINT ( 'NONE',  ( 103.1528011352953342, -3.152801135295355106, 10.81250000136559208 ) ) ;
#17038 = CARTESIAN_POINT ( 'NONE',  ( 99.99999999999998579, 128.0000000000000000, -5.204170427930421283E-15 ) ) ;
#17039 = ORIENTED_EDGE ( 'NONE', *, *, #10185, .F. ) ;
#17040 = CARTESIAN_POINT ( 'NONE',  ( 102.4999999999999858, 123.9000000021849530, -9.847140817659276890E-15 ) ) ;
#17041 = CARTESIAN_POINT ( 'NONE',  ( 96.84719886470459471, 3.152801135295383084, 11.31250000136559208 ) ) ;
#17042 = CARTESIAN_POINT ( 'NONE',  ( 2.414731522848535132E-15, 32.02070312608393010, 13.14518615778179544 ) ) ;
#17043 = CARTESIAN_POINT ( 'NONE',  ( 5.444914386472297529, 39.51171875108392584, -13.14518615778179900 ) ) ;
#17044 = CARTESIAN_POINT ( 'NONE',  ( 0.000000000000000000, -7.395377635281828788, 0.000000000000000000 ) ) ;
#17045 = CARTESIAN_POINT ( 'NONE',  ( 95.54126587499996504, 79.43750000136559208, -1.387778780781445676E-14 ) ) ;
#17046 = CARTESIAN_POINT ( 'NONE',  ( 51.85481384221820633, 40.00781250108393294, 5.444914386472304635 ) ) ;
#17047 = CARTESIAN_POINT ( 'NONE',  ( 91.91746824999998466, 112.6261737610028320, -45.47500000273119980 ) ) ;
#17048 = CARTESIAN_POINT ( 'NONE',  ( 65.00000000000000000, -7.395377635281828788, -7.517135062566165128E-15 ) ) ;
#17049 = CARTESIAN_POINT ( 'NONE',  ( 98.53841926354351699, 122.8500000010924680, -1.461580736456474794 ) ) ;
#17050 = LINE ( 'NONE', #1693, #4963 ) ;
#17051 = CARTESIAN_POINT ( 'NONE',  ( 97.83688103937535629, 116.6573956140660897, -54.89999999453763735 ) ) ;
#17052 = CARTESIAN_POINT ( 'NONE',  ( 139.5988444088204403, 40.70234374999999716, -9.598844408820458085 ) ) ;
#17053 = VERTEX_POINT ( 'NONE', #15845 ) ;
#17054 = DIRECTION ( 'NONE',  ( -0.000000000000000000, -0.000000000000000000, -1.000000000000000000 ) ) ;
#17055 = CARTESIAN_POINT ( 'NONE',  ( -5.444914386472299306, 39.31328125108394289, 13.14518615778179722 ) ) ;
#17056 = FACE_OUTER_BOUND ( 'NONE', #4683, .T. ) ;
#17057 = CARTESIAN_POINT ( 'NONE',  ( 143.1451861577818079, 39.36289062608393152, -1.609821015232357215E-15 ) ) ;
#17058 = CARTESIAN_POINT ( 'NONE',  ( 59.37712712842213136, 36.98164062716787015, -13.57481594606304753 ) ) ;
#17059 = AXIS2_PLACEMENT_3D ( 'NONE', #4173, #6033, #17125 ) ;
#17060 = CARTESIAN_POINT ( 'NONE',  ( 104.9952793366501709, 103.1245878333314323, -52.92499999726882010 ) ) ;
#17061 = CARTESIAN_POINT ( 'NONE',  ( 13.57481594606304931, 34.30273437716787299, 5.622872871577869525 ) ) ;
#17062 = EDGE_LOOP ( 'NONE', ( #12672, #5839, #4989, #16243 ) ) ;
#17063 = CARTESIAN_POINT ( 'NONE',  ( 99.99999999999995737, -4.999999999999990230, 4.249999999999998224 ) ) ;
#17064 = ORIENTED_EDGE ( 'NONE', *, *, #7584, .F. ) ;
#17065 = CARTESIAN_POINT ( 'NONE',  ( 195.0000000000000000, 38.37070312608393152, 13.14518615778179544 ) ) ;
#17066 = CIRCLE ( 'NONE', #1183, 24.13397459621556962 ) ;
#17067 = CARTESIAN_POINT ( 'NONE',  ( -13.57481594606304398, 34.00507812716787726, 5.622872871577880183 ) ) ;
#17068 = CARTESIAN_POINT ( 'NONE',  ( 135.4449143864723339, 37.92421875108393436, -13.14518615778179722 ) ) ;
#17069 = CARTESIAN_POINT ( 'NONE',  ( 55.81982418635200816, 55.00000000000000000, 9.999999999999984013 ) ) ;
#17070 = CARTESIAN_POINT ( 'NONE',  ( 97.50000000000000000, 125.0000000000000000, -9.540979117872439019E-15 ) ) ;
#17071 = FACE_OUTER_BOUND ( 'NONE', #7492, .T. ) ;
#17072 = LINE ( 'NONE', #10517, #21185 ) ;
#17073 = CARTESIAN_POINT ( 'NONE',  ( 102.4999999999999858, 123.0000000000000000, -9.847140817659276890E-15 ) ) ;
#17074 = CARTESIAN_POINT ( 'NONE',  ( 200.6228728715778686, 38.86679687499999858, 13.57481594606304576 ) ) ;
#17075 = CARTESIAN_POINT ( 'NONE',  ( 59.37712712842218110, 39.26367187500000000, -13.57481594606310260 ) ) ;
#17076 = CARTESIAN_POINT ( 'NONE',  ( 95.54126587499995082, -1.846868145590724986, 2.750000001365592084 ) ) ;
#17077 = CARTESIAN_POINT ( 'NONE',  ( 59.55508561352770158, 38.81718750108393579, -13.14518615778179900 ) ) ;
#17078 = EDGE_CURVE ( 'NONE', #8637, #17432, #22282, .T. ) ;
#17079 =( BOUNDED_CURVE ( )  B_SPLINE_CURVE ( 2, ( #12172, #14460, #16471, #23177, #14318, #12036, #27458, #3510, #25830 ),
 .UNSPECIFIED., .F., .F. ) 
 B_SPLINE_CURVE_WITH_KNOTS ( ( 3, 2, 2, 2, 3 ),
 ( 0.4375000000000003331, 0.4479166666666669627, 0.4583333333333335369, 0.4687500000000001665, 0.4791666666666667962 ),
 .UNSPECIFIED. ) 
 CURVE ( )  GEOMETRIC_REPRESENTATION_ITEM ( )  RATIONAL_B_SPLINE_CURVE ( ( 0.9999999999999975575, 0.9238795325112891810, 1.000000000000000000, 0.9238795325112867385, 1.000000000000000000, 0.9238795325112867385, 1.000000000000000000, 0.9238795325112859613, 1.000000000000000888 ) ) 
 REPRESENTATION_ITEM ( '' )  );
#17080 = AXIS2_PLACEMENT_3D ( 'NONE', #1371, #27861, #25710 ) ;
#17081 = CARTESIAN_POINT ( 'NONE',  ( 95.54126587499996504, 1.846868145590750077, 6.375000001365592084 ) ) ;
#17082 = CARTESIAN_POINT ( 'NONE',  ( 104.3262379212492590, 115.9545556584642867, -45.20000000546238539 ) ) ;
#17083 = CARTESIAN_POINT ( 'NONE',  ( 98.15313185440925281, 94.62499999863439371, -4.458734124999994997 ) ) ;
#17084 = CARTESIAN_POINT ( 'NONE',  ( 97.93301270000000613, 124.6500000010924651, -9.540979117872439019E-15 ) ) ;
#17085 = CARTESIAN_POINT ( 'NONE',  ( -5.622872871577873077, 38.46992187499999716, -13.57481594606304753 ) ) ;
#17086 = CARTESIAN_POINT ( 'NONE',  ( 130.0000000000000000, 39.75976562608394005, -13.14518615778179544 ) ) ;
#17087 = ORIENTED_EDGE ( 'NONE', *, *, #22101, .F. ) ;
#17088 = CARTESIAN_POINT ( 'NONE',  ( 95.54126587499995082, 81.62500000136560629, -1.846868145590750077 ) ) ;
#17089 = AXIS2_PLACEMENT_3D ( 'NONE', #15396, #23827, #4307 ) ;
#17090 = LINE ( 'NONE', #12388, #12015 ) ;
#17091 = ORIENTED_EDGE ( 'NONE', *, *, #12266, .F. ) ;
#17092 = CARTESIAN_POINT ( 'NONE',  ( 0.000000000000000000, 23.00000000000000000, -25.00000000000001066 ) ) ;
#17093 = CARTESIAN_POINT ( 'NONE',  ( 55.70494972787295751, 33.50898437608393010, -9.295050272127046043 ) ) ;
#17094 = ORIENTED_EDGE ( 'NONE', *, *, #17152, .T. ) ;
#17095 = LINE ( 'NONE', #17239, #26338 ) ;
#17096 = CARTESIAN_POINT ( 'NONE',  ( 96.84719886470459471, 3.152801135295383084, 1.562500001365592972 ) ) ;
#17097 = VERTEX_POINT ( 'NONE', #9294 ) ;
#17098 = CARTESIAN_POINT ( 'NONE',  ( 13.14518615778179544, 35.59257812608393579, -1.609821015232357215E-15 ) ) ;
#17099 = CARTESIAN_POINT ( 'NONE',  ( -9.295050272127046043, 38.27148437608393294, -9.295050272127046043 ) ) ;
#17100 = CARTESIAN_POINT ( 'NONE',  ( 200.6228728715778686, 38.46992187716787015, -13.57481594606304753 ) ) ;
#17101 = CARTESIAN_POINT ( 'NONE',  ( -13.14518615778179189, 36.63437500108393863, 5.444914386472304635 ) ) ;
#17102 = CARTESIAN_POINT ( 'NONE',  ( 97.50000000000000000, 124.3000000021849587, -9.540979117872439019E-15 ) ) ;
#17103 = CARTESIAN_POINT ( 'NONE',  ( 203.7693896720689963, 50.37710889401661518, 14.99999999999732836 ) ) ;
#17104 = CARTESIAN_POINT ( 'NONE',  ( 143.1451861577818363, 38.81718750108393579, -5.444914386472297529 ) ) ;
#17105 = CARTESIAN_POINT ( 'NONE',  ( 2.414731522848535132E-15, 37.77539062608393294, 13.14518615778179544 ) ) ;
#17106 = EDGE_LOOP ( 'NONE', ( #11011, #24331, #23902, #8692 ) ) ;
#17107 = CARTESIAN_POINT ( 'NONE',  ( 143.1451861577818079, 33.75703125108393010, 5.444914386472293977 ) ) ;
#17108 = CARTESIAN_POINT ( 'NONE',  ( 51.42518405393695957, 37.87460937499999147, 5.622872871577880183 ) ) ;
#17109 = AXIS2_PLACEMENT_3D ( 'NONE', #25899, #2389, #13462 ) ;
#17110 = CARTESIAN_POINT ( 'NONE',  ( 13.57481594606304931, 38.27148437716787299, 5.622872871577868636 ) ) ;
#17111 = CARTESIAN_POINT ( 'NONE',  ( 98.15313185440925281, 4.458734125000016313, 1.250000001365592750 ) ) ;
#17112 = CARTESIAN_POINT ( 'NONE',  ( 105.6631189606246295, 114.1144967660473242, -46.80000000000001137 ) ) ;
#17113 = CARTESIAN_POINT ( 'NONE',  ( 101.8468681455906903, -4.458734124999987891, 3.750000001365591640 ) ) ;
#17114 = CARTESIAN_POINT ( 'NONE',  ( 104.9999999999999716, 2.071067811865491937, 3.687500002731185056 ) ) ;
#17115 = CARTESIAN_POINT ( 'NONE',  ( 95.54126587499996504, -1.846868145590724986, 0.7500000013655925279 ) ) ;
#17116 =( BOUNDED_CURVE ( )  B_SPLINE_CURVE ( 2, ( #1086, #7471, #3633, #9892, #27577 ),
 .UNSPECIFIED., .F., .F. ) 
 B_SPLINE_CURVE_WITH_KNOTS ( ( 3, 2, 3 ),
 ( 0.000000000000000000, 0.01041666666666679446, 0.02083333333333358892 ),
 .UNSPECIFIED. ) 
 CURVE ( )  GEOMETRIC_REPRESENTATION_ITEM ( )  RATIONAL_B_SPLINE_CURVE ( ( 1.000000000000000000, 0.9238795325112867385, 1.000000000000000000, 0.9238795325112848511, 1.000000000000001776 ) ) 
 REPRESENTATION_ITEM ( '' )  );
#17117 = DIRECTION ( 'NONE',  ( -0.000000000000000000, -1.000000000000000000, -0.000000000000000000 ) ) ;
#17118 = CARTESIAN_POINT ( 'NONE',  ( 97.50236033167490746, 117.6869444889999841, -46.02499999726882152 ) ) ;
#17119 = CARTESIAN_POINT ( 'NONE',  ( -9.295050272127046043, 38.27148437608393294, -9.295050272127046043 ) ) ;
#17120 = CARTESIAN_POINT ( 'NONE',  ( 93.46109445667489979, 114.7507929638356785, -46.07499999726881867 ) ) ;
#17121 = ORIENTED_EDGE ( 'NONE', *, *, #11906, .F. ) ;
#17122 = ADVANCED_FACE ( 'NONE', ( #24268 ), #51, .F. ) ;
#17123 = CARTESIAN_POINT ( 'NONE',  ( -5.444914386472299306, 32.96328125108393436, 13.14518615778179722 ) ) ;
#17124 = AXIS2_PLACEMENT_3D ( 'NONE', #10000, #24848, #1059 ) ;
#17125 = DIRECTION ( 'NONE',  ( 0.000000000000000000, 0.000000000000000000, -1.000000000000000000 ) ) ;
#17126 = CARTESIAN_POINT ( 'NONE',  ( 98.81505309850513186, 123.0000000000000426, 1.864324913875618162 ) ) ;
#17127 = CARTESIAN_POINT ( 'NONE',  ( -9.598844408820454532, 40.30546874999999574, 9.598844408820459861 ) ) ;
#17128 = CARTESIAN_POINT ( 'NONE',  ( 3.878385297391210518, 32.03609435653363136, -13.57481594606304576 ) ) ;
#17129 = CARTESIAN_POINT ( 'NONE',  ( 185.7049497278729575, 39.85898437608393152, 9.295050272127047819 ) ) ;
#17130 = CIRCLE ( 'NONE', #28075, 13.57481594606304576 ) ;
#17131 = ORIENTED_EDGE ( 'NONE', *, *, #2461, .F. ) ;
#17132 = FACE_OUTER_BOUND ( 'NONE', #23562, .T. ) ;
#17133 = CARTESIAN_POINT ( 'NONE',  ( 95.67376207875072680, 104.0454443415356991, -54.70000000000000995 ) ) ;
#17134 = AXIS2_PLACEMENT_3D ( 'NONE', #12828, #173, #17546 ) ;
#17135 = CARTESIAN_POINT ( 'NONE',  ( 99.99999999999995737, 4.458734125000016313, 14.43750000136559208 ) ) ;
#17136 = ORIENTED_EDGE ( 'NONE', *, *, #11224, .T. ) ;
#17137 = CARTESIAN_POINT ( 'NONE',  ( 95.67376207875072680, 115.9545556584642867, -50.30000000000000426 ) ) ;
#17138 = CARTESIAN_POINT ( 'NONE',  ( 104.9999999999999716, 1.449011120738813565E-14, 5.500000000000000000 ) ) ;
#17139 = CARTESIAN_POINT ( 'NONE',  ( 99.99999999999998579, 123.3500000010924680, 2.066987299999980099 ) ) ;
#17140 = CARTESIAN_POINT ( 'NONE',  ( 124.3771271284221314, 34.89804687716787868, 13.57481594606304753 ) ) ;
#17141 = VECTOR ( 'NONE', #25097, 1000.000000000000000 ) ;
#17142 = CARTESIAN_POINT ( 'NONE',  ( 99.99999999999995737, 81.37500000273119838, 4.999999999999990230 ) ) ;
#17143 = CARTESIAN_POINT ( 'NONE',  ( 5.622872871577870413, 37.57695312499999574, -13.57481594606304753 ) ) ;
#17144 = CARTESIAN_POINT ( 'NONE',  ( 185.7049497278729575, 35.09648437608393579, -9.295050272127046043 ) ) ;
#17145 = VERTEX_POINT ( 'NONE', #2757 ) ;
#17146 = ORIENTED_EDGE ( 'NONE', *, *, #22375, .F. ) ;
#17147 = VERTEX_POINT ( 'NONE', #20140 ) ;
#17148 = CARTESIAN_POINT ( 'NONE',  ( 13.14518615778179544, 38.76757812608393294, -1.609821015232357215E-15 ) ) ;
#17149 = DIRECTION ( 'NONE',  ( -0.8660254037844407060, 0.4999999999999963363, 0.000000000000000000 ) ) ;
#17150 = EDGE_CURVE ( 'NONE', #21981, #15490, #620, .T. ) ;
#17151 = CARTESIAN_POINT ( 'NONE',  ( 13.57481594606304753, 38.27148437500000711, -5.622872871577873966 ) ) ;
#17152 = EDGE_CURVE ( 'NONE', #22143, #26327, #11420, .T. ) ;
#17153 = CARTESIAN_POINT ( 'NONE',  ( 96.84719886470459471, 81.31250000136559208, -3.152801135295383084 ) ) ;
#17154 = CARTESIAN_POINT ( 'NONE',  ( 181.8548138422182205, 38.91640625108393436, -5.444914386472297529 ) ) ;
#17155 = CARTESIAN_POINT ( 'NONE',  ( 100.0000000000000000, 110.0000000000000000, -55.00000000000000711 ) ) ;
#17156 = CARTESIAN_POINT ( 'NONE',  ( 102.3556624333333076, 122.9166666670308246, -9.829464563757769835E-15 ) ) ;
#17157 = CARTESIAN_POINT ( 'NONE',  ( 99.99999999999998579, 128.0000000000000000, 2.500000000000003553 ) ) ;
#17158 = CARTESIAN_POINT ( 'NONE',  ( 204.2950502721270425, 39.66054687608393436, -9.295050272127046043 ) ) ;
#17159 = CARTESIAN_POINT ( 'NONE',  ( 99.99999999999997158, 118.4984768113314004, -48.12499999726881583 ) ) ;
#17160 = EDGE_CURVE ( 'NONE', #12494, #2842, #24085, .T. ) ;
#17161 = B_SPLINE_CURVE_WITH_KNOTS ( 'NONE', 3,
 ( #6443, #7103, #6965, #1904, #4848, #17126, #8297, #15114, #23834, #19412, #19135, #2711, #14979, #9253, #6303, #572, #24505, #10706 ),
 .UNSPECIFIED., .F., .F.,
 ( 4, 2, 2, 2, 2, 2, 2, 2, 4 ),
 ( 0.000000000000000000, 0.0005608035638250541540, 0.001121607127650108308, 0.001682410691475162787, 0.002243214255300217484, 0.002804017819125271746, 0.003364821382950326442, 0.003925624946775381138, 0.004486428510600435834 ),
 .UNSPECIFIED. ) ;
#17162 = ORIENTED_EDGE ( 'NONE', *, *, #2338, .T. ) ;
#17163 =( BOUNDED_CURVE ( )  B_SPLINE_CURVE ( 2, ( #27862, #8322, #6193, #14863, #12162, #10164, #14587, #12027, #23307 ),
 .UNSPECIFIED., .F., .F. ) 
 B_SPLINE_CURVE_WITH_KNOTS ( ( 3, 2, 2, 2, 3 ),
 ( 0.2500000000000002220, 0.2750000000000002442, 0.3000000000000002665, 0.3250000000000002887, 0.3500000000000003109 ),
 .UNSPECIFIED. ) 
 CURVE ( )  GEOMETRIC_REPRESENTATION_ITEM ( )  RATIONAL_B_SPLINE_CURVE ( ( 0.9999999999999993339, 0.9238795325112874046, 1.000000000000000000, 0.9238795325112867385, 1.000000000000000000, 0.9238795325112867385, 1.000000000000000000, 0.9238795325112857393, 1.000000000000001110 ) ) 
 REPRESENTATION_ITEM ( '' )  );
#17164 = CARTESIAN_POINT ( 'NONE',  ( -5.622872871577873077, 35.29492187500000000, -13.57481594606304753 ) ) ;
#17165 = CARTESIAN_POINT ( 'NONE',  ( -8.049105076161786076E-16, 36.38632812608393152, -13.14518615778179544 ) ) ;
#17166 = CARTESIAN_POINT ( 'NONE',  ( 94.99999999999995737, 2.071067811865491048, 2.062500002731185500 ) ) ;
#17167 = CARTESIAN_POINT ( 'NONE',  ( 130.0000000000000000, 35.39414062608393863, 13.14518615778179544 ) ) ;
#17168 = AXIS2_PLACEMENT_3D ( 'NONE', #25014, #1083, #23296 ) ;
#17169 = CARTESIAN_POINT ( 'NONE',  ( 59.55508561352770158, 38.02343750108394005, -13.14518615778179900 ) ) ;
#17170 = EDGE_CURVE ( 'NONE', #4508, #17588, #9689, .T. ) ;
#17171 = CARTESIAN_POINT ( 'NONE',  ( 181.8548138422181921, 39.21406250108392300, 5.444914386472304635 ) ) ;
#17172 = DIRECTION ( 'NONE',  ( 0.000000000000000000, 1.000000000000000000, 0.000000000000000000 ) ) ;
#17173 = CARTESIAN_POINT ( 'NONE',  ( -5.444914386472299306, 34.35234375108392868, 13.14518615778179722 ) ) ;
#17174 = CARTESIAN_POINT ( 'NONE',  ( 123.9140557840132573, 54.65299103241509471, -15.00000000000000000 ) ) ;
#17175 = CARTESIAN_POINT ( 'NONE',  ( 124.3771271284221172, 40.35507812499999147, 13.57481594606302444 ) ) ;
#17176 = CARTESIAN_POINT ( 'NONE',  ( 2.414731522848535132E-15, 39.16445312608392726, 13.14518615778179544 ) ) ;
#17177 = CARTESIAN_POINT ( 'NONE',  ( 94.99999999999995737, 1.387778780781445676E-14, 11.00000000000000000 ) ) ;
#17178 = CYLINDRICAL_SURFACE ( 'NONE', #5971, 5.000000000000004441 ) ;
#17179 = CARTESIAN_POINT ( 'NONE',  ( -13.57481594606304576, 37.03124999999999289, 0.000000000000000000 ) ) ;
#17180 = CARTESIAN_POINT ( 'NONE',  ( 95.54126587499995082, 1.846868145590750077, 7.375000001365592084 ) ) ;
#17181 = DIRECTION ( 'NONE',  ( 1.000000000000000000, 0.000000000000000000, 0.000000000000000000 ) ) ;
#17182 = ORIENTED_EDGE ( 'NONE', *, *, #23604, .T. ) ;
#17183 = CARTESIAN_POINT ( 'NONE',  ( 104.3262379212492590, 104.0454443415356991, -53.29999999999999716 ) ) ;
#17184 = CARTESIAN_POINT ( 'NONE',  ( 95.54126587499995082, -1.846868145590724986, 12.50000000136559208 ) ) ;
#17185 = CARTESIAN_POINT ( 'NONE',  ( 130.4460412567749188, 49.99999999978043519, 13.57776691409199898 ) ) ;
#17186 = CARTESIAN_POINT ( 'NONE',  ( 13.14518615778179544, 37.77539062608393294, -1.609821015232357215E-15 ) ) ;
#17187 = CARTESIAN_POINT ( 'NONE',  ( 112.9999999999999858, 102.0000000000000000, -43.00000000000000000 ) ) ;
#17188 = CARTESIAN_POINT ( 'NONE',  ( 99.99999999999995737, 79.93750000136559208, 4.458734124999988779 ) ) ;
#17189 = CARTESIAN_POINT ( 'NONE',  ( 59.55508561352770158, 37.42812500108394147, -13.14518615778179900 ) ) ;
#17190 = CARTESIAN_POINT ( 'NONE',  ( 102.4976396683250925, 102.3130555110000159, -50.52500000273119696 ) ) ;
#17191 = CARTESIAN_POINT ( 'NONE',  ( -13.14518615778179722, 39.71015625108393010, -5.444914386472297529 ) ) ;
#17192 = PLANE ( 'NONE',  #2570 ) ;
#17193 = LINE ( 'NONE', #6370, #25883 ) ;
#17194 = CARTESIAN_POINT ( 'NONE',  ( 105.6631189606246295, 105.8855032339526758, -53.69999999453763451 ) ) ;
#17195 = CARTESIAN_POINT ( 'NONE',  ( 124.3771271284221314, 40.35507812499998437, 13.57481594606304753 ) ) ;
#17196 = EDGE_CURVE ( 'NONE', #11161, #22131, #27019, .T. ) ;
#17197 = ORIENTED_EDGE ( 'NONE', *, *, #10510, .F. ) ;
#17198 = DIRECTION ( 'NONE',  ( -0.000000000000000000, -1.000000000000000000, -0.000000000000000000 ) ) ;
#17199 = CARTESIAN_POINT ( 'NONE',  ( -9.295050272127044266, 38.46992187608393721, 9.295050272127047819 ) ) ;
#17200 = CARTESIAN_POINT ( 'NONE',  ( 13.57481594606304576, 39.90859375216787441, -1.662435489736055892E-15 ) ) ;
#17201 =( BOUNDED_CURVE ( )  B_SPLINE_CURVE ( 2, ( #3537, #16903, #21337, #25600, #10621, #6086, #14752, #1405, #10064 ),
 .UNSPECIFIED., .F., .F. ) 
 B_SPLINE_CURVE_WITH_KNOTS ( ( 3, 2, 2, 2, 3 ),
 ( 0.03571428571428574700, 0.04464285714285718548, 0.05357142857142861703, 0.06250000000000005551, 0.07142857142857149400 ),
 .UNSPECIFIED. ) 
 CURVE ( )  GEOMETRIC_REPRESENTATION_ITEM ( )  RATIONAL_B_SPLINE_CURVE ( ( 0.9999999999999996669, 0.9238795325112870716, 1.000000000000000000, 0.9238795325112867385, 1.000000000000000000, 0.9238795325112867385, 1.000000000000000000, 0.9238795325112861834, 1.000000000000000666 ) ) 
 REPRESENTATION_ITEM ( '' )  );
#17202 = CARTESIAN_POINT ( 'NONE',  ( 135.4449143864723055, 36.03906250108394005, 13.14518615778179189 ) ) ;
#17203 = CARTESIAN_POINT ( 'NONE',  ( 51.42518405393695957, 36.28710937716787299, -5.622872871577873077 ) ) ;
#17204 = CARTESIAN_POINT ( 'NONE',  ( 10.56308295036056677, 36.00000000000000711, 8.196709705856857653 ) ) ;
#17205 = CARTESIAN_POINT ( 'NONE',  ( -9.598844408820458085, 37.03125000216787299, -9.598844408820458085 ) ) ;
#17206 = VECTOR ( 'NONE', #16642, 1000.000000000000000 ) ;
#17207 = CARTESIAN_POINT ( 'NONE',  ( 104.9999999999999716, 1.449011120738813565E-14, 5.500000000000000000 ) ) ;
#17208 = CARTESIAN_POINT ( 'NONE',  ( 102.0710678118654329, 5.000000000000018652, 1.687499999999999778 ) ) ;
#17209 = CARTESIAN_POINT ( 'NONE',  ( 185.4011555911795597, 33.16171874999999858, 9.598844408820459861 ) ) ;
#17210 = CARTESIAN_POINT ( 'NONE',  ( 204.2950502721270425, 38.66835937608393436, -9.295050272127046043 ) ) ;
#17211 = CARTESIAN_POINT ( 'NONE',  ( 65.00000000000000000, 38.42031249999999432, -13.57481594606304576 ) ) ;
#17212 = CARTESIAN_POINT ( 'NONE',  ( 5.622872871577878406, 34.20351562716788152, 13.57481594606304398 ) ) ;
#17213 = EDGE_LOOP ( 'NONE', ( #4329, #4032, #16411, #27091 ) ) ;
#17214 = CARTESIAN_POINT ( 'NONE',  ( 5.622872871577694553, 35.69179687499999432, 13.57481594606322695 ) ) ;
#17215 = CARTESIAN_POINT ( 'NONE',  ( 126.1345856245867907, 54.10683252460150072, 14.99999999999996980 ) ) ;
#17216 = CARTESIAN_POINT ( 'NONE',  ( 51.42518405393695957, 37.08085937499999574, 5.622872871577880183 ) ) ;
#17217 = CARTESIAN_POINT ( 'NONE',  ( -9.295050272127046043, 36.68398437608393436, -9.295050272127046043 ) ) ;
#17218 = CARTESIAN_POINT ( 'NONE',  ( 13.14518615778179900, 37.82500000108392868, -5.444914386472297529 ) ) ;
#17219 = CARTESIAN_POINT ( 'NONE',  ( 181.4251840539369596, 37.77539062499999289, -5.622872871577873077 ) ) ;
#17220 = CARTESIAN_POINT ( 'NONE',  ( 65.00000000000000000, -7.395377635281828788, -13.57481594606305109 ) ) ;
#17221 = CARTESIAN_POINT ( 'NONE',  ( 95.54126587499996504, 1.387778780781445676E-14, 1.687500001365591418 ) ) ;
#17222 = CARTESIAN_POINT ( 'NONE',  ( 70.44491438647230552, 37.92421875108392726, -13.14518615778179900 ) ) ;
#17223 = CARTESIAN_POINT ( 'NONE',  ( 104.4587341249999639, 1.442382525525748735E-14, 0.9375000013655925279 ) ) ;
#17224 = CARTESIAN_POINT ( 'NONE',  ( 102.1631189606246295, 103.3426043859339103, -43.90000000546237402 ) ) ;
#17225 = CARTESIAN_POINT ( 'NONE',  ( 98.15313185440925281, 93.62499999863440792, -4.458734124999994997 ) ) ;
#17226 = CARTESIAN_POINT ( 'NONE',  ( -3.136173621347420060, 36.00000000000000711, 12.79489613812762450 ) ) ;
#17227 = CARTESIAN_POINT ( 'NONE',  ( 5.622872871577871301, 39.16445312499999432, -13.57481594606304753 ) ) ;
#17228 = CARTESIAN_POINT ( 'NONE',  ( 124.5550856135277087, 39.31328125108394289, 13.14518615778179722 ) ) ;
#17229 = AXIS2_PLACEMENT_3D ( 'NONE', #5789, #8050, #20897 ) ;
#17230 = AXIS2_PLACEMENT_3D ( 'NONE', #16313, #3769, #14160 ) ;
#17231 = VERTEX_POINT ( 'NONE', #17534 ) ;
#17232 = CARTESIAN_POINT ( 'NONE',  ( 97.92893218813451028, 83.18750000000001421, 4.999999999999989342 ) ) ;
#17233 = AXIS2_PLACEMENT_3D ( 'NONE', #13300, #19599, #20173 ) ;
#17234 = CARTESIAN_POINT ( 'NONE',  ( 99.99999999999998579, 95.06249999863440792, 4.458734124999981674 ) ) ;
#17235 = ORIENTED_EDGE ( 'NONE', *, *, #13476, .F. ) ;
#17236 = DIRECTION ( 'NONE',  ( 0.000000000000000000, 0.000000000000000000, -1.000000000000000000 ) ) ;
#17237 = CARTESIAN_POINT ( 'NONE',  ( 74.29505027212704249, 33.31054687608394005, -9.295050272127046043 ) ) ;
#17238 = VERTEX_POINT ( 'NONE', #15238 ) ;
#17239 = CARTESIAN_POINT ( 'NONE',  ( 114.9999999999999858, 100.0000000000000000, -15.00000000000000711 ) ) ;
#17240 = CARTESIAN_POINT ( 'NONE',  ( 99.99999999999995737, -4.458734124999988779, 0.9375000013655925279 ) ) ;
#17241 = EDGE_CURVE ( 'NONE', #5424, #7349, #588, .T. ) ;
#17242 = EDGE_LOOP ( 'NONE', ( #18606, #11476, #59, #22591 ) ) ;
#17243 = CARTESIAN_POINT ( 'NONE',  ( -13.14518615778179722, 35.93984375108393436, -5.444914386472297529 ) ) ;
#17244 = CARTESIAN_POINT ( 'NONE',  ( 9.295050272127047819, 39.46210937608393721, 9.295050272127046043 ) ) ;
#17245 = UNCERTAINTY_MEASURE_WITH_UNIT (LENGTH_MEASURE( 1.000000000000000082E-05 ), #16604, 'distance_accuracy_value', 'NONE');
#17246 = EDGE_CURVE ( 'NONE', #3560, #4816, #21967, .T. ) ;
#17247 = CARTESIAN_POINT ( 'NONE',  ( 208.5748159460630688, 39.11484375216787157, -1.662435489736055892E-15 ) ) ;
#17248 = CARTESIAN_POINT ( 'NONE',  ( 9.295050272127047819, 37.67617187608393436, 9.295050272127046043 ) ) ;
#17249 = CARTESIAN_POINT ( 'NONE',  ( 92.99999999999998579, 110.0000000000000000, -52.49999999453763877 ) ) ;
#17250 = CARTESIAN_POINT ( 'NONE',  ( 196.8921833570923923, 53.66387243068088964, 14.99999999999994671 ) ) ;
#17251 = CARTESIAN_POINT ( 'NONE',  ( 116.8548138422182205, 38.42031250108393436, 5.444914386472304635 ) ) ;
#17252 = CARTESIAN_POINT ( 'NONE',  ( 13.14518615778179900, 37.22968750108393721, -5.444914386472297529 ) ) ;
#17253 =( GEOMETRIC_REPRESENTATION_CONTEXT ( 3 ) GLOBAL_UNCERTAINTY_ASSIGNED_CONTEXT ( ( #19814 ) ) GLOBAL_UNIT_ASSIGNED_CONTEXT ( ( #13163, #17036, #10478 ) ) REPRESENTATION_CONTEXT ( 'NONE', 'WORKASPACE' ) );
#17254 = CARTESIAN_POINT ( 'NONE',  ( 135.4449143864723055, 35.54296875108393294, -13.14518615778179900 ) ) ;
#17255 = CARTESIAN_POINT ( 'NONE',  ( 70.62287287157786864, 38.37070312499999147, -13.57481594606304753 ) ) ;
#17256 = DIRECTION ( 'NONE',  ( -0.000000000000000000, -1.000000000000000000, -0.000000000000000000 ) ) ;
#17257 = AXIS2_PLACEMENT_3D ( 'NONE', #6850, #10696, #4584 ) ;
#17258 = CARTESIAN_POINT ( 'NONE',  ( 101.8468681455906903, -4.458734124999987891, 1.750000001365591862 ) ) ;
#17259 = CARTESIAN_POINT ( 'NONE',  ( 196.1371678245420753, 35.99999999999999289, 13.09590655363592582 ) ) ;
#17260 = CARTESIAN_POINT ( 'NONE',  ( 95.54126587499996504, 1.387778780781445676E-14, 3.437500001365592972 ) ) ;
#17261 = CARTESIAN_POINT ( 'NONE',  ( 95.00472066334982912, 116.8754121666685393, -51.42500000273118843 ) ) ;
#17262 = CARTESIAN_POINT ( 'NONE',  ( 9.598844408820459861, 39.01562500216787299, 9.598844408820456309 ) ) ;
#17263 = DIRECTION ( 'NONE',  ( 0.000000000000000000, 1.000000000000000000, 0.000000000000000000 ) ) ;
#17264 = CARTESIAN_POINT ( 'NONE',  ( -13.14518615778179544, 32.61601562608393579, 0.000000000000000000 ) ) ;
#17265 = CARTESIAN_POINT ( 'NONE',  ( 5.444914386472297529, 38.91640625108393436, -13.14518615778179900 ) ) ;
#17266 = CARTESIAN_POINT ( 'NONE',  ( 104.9952793366501709, 103.1245878333314323, -51.17499999726881299 ) ) ;
#17267 = ORIENTED_EDGE ( 'NONE', *, *, #28137, .T. ) ;
#17268 = CARTESIAN_POINT ( 'NONE',  ( 97.93301270000000613, 123.9500000010924765, -9.540979117872439019E-15 ) ) ;
#17269 = CARTESIAN_POINT ( 'NONE',  ( 99.99999999999995737, 79.87500000273119838, -5.000000000000018652 ) ) ;
#17270 = DIRECTION ( 'NONE',  ( 0.000000000000000000, -1.000000000000000000, 0.000000000000000000 ) ) ;
#17271 = CARTESIAN_POINT ( 'NONE',  ( 195.0000000000000000, 39.16445312608392726, 13.14518615778179544 ) ) ;
#17272 = ORIENTED_EDGE ( 'NONE', *, *, #27289, .T. ) ;
#17273 = CARTESIAN_POINT ( 'NONE',  ( 99.99999999999998579, 90.00000000000000000, -4.999999999999996447 ) ) ;
#17274 = VECTOR ( 'NONE', #1182, 1000.000000000000000 ) ;
#17275 = CARTESIAN_POINT ( 'NONE',  ( 99.99999999999995737, 1.387778780781445676E-14, 34.79898987322334136 ) ) ;
#17276 = CARTESIAN_POINT ( 'NONE',  ( 139.5988444088204687, 39.71015624999999716, 9.598844408820456309 ) ) ;
#17277 = ORIENTED_EDGE ( 'NONE', *, *, #11512, .T. ) ;
#17278 = CARTESIAN_POINT ( 'NONE',  ( 102.1631189606246295, 103.3426043859339103, -53.40000000000001279 ) ) ;
#17279 = CARTESIAN_POINT ( 'NONE',  ( 5.444914386472302859, 38.42031250108393436, 13.14518615778179189 ) ) ;
#17280 = CARTESIAN_POINT ( 'NONE',  ( 97.93301269999999192, 123.2000000010924765, 0.8561741729129329626 ) ) ;
#17281 = VECTOR ( 'NONE', #1624, 1000.000000000000000 ) ;
#17282 = CARTESIAN_POINT ( 'NONE',  ( 135.4449143864723055, 40.30546875108393579, -13.14518615778179900 ) ) ;
#17283 = DIRECTION ( 'NONE',  ( 0.000000000000000000, 1.000000000000000000, 0.000000000000000000 ) ) ;
#17284 =( BOUNDED_CURVE ( )  B_SPLINE_CURVE ( 2, ( #11219, #23929, #416, #4408, #8958, #9242, #13062, #24070, #26646 ),
 .UNSPECIFIED., .F., .T. ) 
 B_SPLINE_CURVE_WITH_KNOTS ( ( 3, 2, 2, 2, 3 ),
 ( 0.1875000000000001388, 0.1979166666666667407, 0.2083333333333333703, 0.2187499999999999722, 0.2291666666666665741 ),
 .UNSPECIFIED. ) 
 CURVE ( )  GEOMETRIC_REPRESENTATION_ITEM ( )  RATIONAL_B_SPLINE_CURVE ( ( 0.9999999999999990008, 0.9238795325112877377, 1.000000000000000000, 0.9238795325112867385, 1.000000000000000000, 0.9238795325112867385, 1.000000000000000000, 0.9238795325112872936, 0.9999999999999994449 ) ) 
 REPRESENTATION_ITEM ( '' )  );
#17285 = CARTESIAN_POINT ( 'NONE',  ( 78.14518615778179367, 39.56132812608393579, -1.609821015232357215E-15 ) ) ;
#17286 = CARTESIAN_POINT ( 'NONE',  ( -8.312177448680279460E-16, 37.62656249999999858, -13.57481594606304576 ) ) ;
#17287 = CARTESIAN_POINT ( 'NONE',  ( 208.1451861577817795, 34.84843750108393579, -5.444914386472297529 ) ) ;
#17288 = ORIENTED_EDGE ( 'NONE', *, *, #21750, .T. ) ;
#17289 = ORIENTED_EDGE ( 'NONE', *, *, #20138, .F. ) ;
#17290 = CARTESIAN_POINT ( 'NONE',  ( 13.14518615778179900, 37.92421875108392726, 5.444914386472293977 ) ) ;
#17291 = CARTESIAN_POINT ( 'NONE',  ( 103.1528011352953342, -3.152801135295355106, 11.06250000136559208 ) ) ;
#17292 = CARTESIAN_POINT ( 'NONE',  ( 51.85481384221820633, 39.75976562608393294, 0.000000000000000000 ) ) ;
#17293 = CARTESIAN_POINT ( 'NONE',  ( 103.1528011352953342, 80.81250000136559208, 3.152801135295355106 ) ) ;
#17294 = CARTESIAN_POINT ( 'NONE',  ( 200.4449143864723055, 38.71796875108393721, -13.14518615778179722 ) ) ;
#17295 = DIRECTION ( 'NONE',  ( 1.000000000000000000, 0.000000000000000000, 0.000000000000000000 ) ) ;
#17296 = LINE ( 'NONE', #8326, #11371 ) ;
#17297 = CARTESIAN_POINT ( 'NONE',  ( 94.99999999999995737, 1.387778780781445676E-14, 12.00000000000000000 ) ) ;
#17298 = CARTESIAN_POINT ( 'NONE',  ( 102.1631189606246295, 103.3426043859339103, -49.40000000000000568 ) ) ;
#17299 = CARTESIAN_POINT ( 'NONE',  ( 102.4976396683250783, 117.6869444889999841, -50.22499999726882436 ) ) ;
#17300 = EDGE_LOOP ( 'NONE', ( #5078, #678, #19154 ) ) ;
#17301 = EDGE_CURVE ( 'NONE', #21288, #12843, #2071, .T. ) ;
#17302 = MECHANICAL_DESIGN_GEOMETRIC_PRESENTATION_REPRESENTATION (  '', ( #18239 ), #6385 ) ;
#17303 = CARTESIAN_POINT ( 'NONE',  ( 9.598844408820459861, 36.53515624999999289, 9.598844408820456309 ) ) ;
#17304 = CARTESIAN_POINT ( 'NONE',  ( -5.444914386472299306, 36.73359375108393010, 13.14518615778179722 ) ) ;
#17305 = CARTESIAN_POINT ( 'NONE',  ( 103.5355339059327093, -3.535533905932726206, 2.500000002731185500 ) ) ;
#17306 = CARTESIAN_POINT ( 'NONE',  ( 124.5550856135277087, 36.13828125108393863, 13.14518615778179722 ) ) ;
#17307 = CARTESIAN_POINT ( 'NONE',  ( 65.00000000000000000, 32.41757812608393863, -13.14518615778179544 ) ) ;
#17308 = CARTESIAN_POINT ( 'NONE',  ( 195.0000000000000000, 38.17226562608394147, -13.14518615778179544 ) ) ;
#17309 = EDGE_LOOP ( 'NONE', ( #13080, #19892, #17182, #7395, #11435, #12314, #15630, #6720 ) ) ;
#17310 = DIRECTION ( 'NONE',  ( 0.000000000000000000, -1.000000000000000000, 0.000000000000000000 ) ) ;
#17311 = CARTESIAN_POINT ( 'NONE',  ( -13.14518615778179544, 31.82226562608393650, 0.000000000000000000 ) ) ;
#17312 = CARTESIAN_POINT ( 'NONE',  ( 138.4023157812348472, 54.99999999485618929, -15.00000000000000000 ) ) ;
#17313 = EDGE_CURVE ( 'NONE', #10602, #8880, #27919, .T. ) ;
#17314 = CARTESIAN_POINT ( 'NONE',  ( 190.2199608011490852, 35.99999999999998579, 12.25280873422859784 ) ) ;
#17315 = CARTESIAN_POINT ( 'NONE',  ( 13.14518615778179900, 33.26093750108393721, -5.444914386472297529 ) ) ;
#17316 = CARTESIAN_POINT ( 'NONE',  ( 91.91746824999998466, 112.6261737610028320, -53.22500000273119269 ) ) ;
#17317 = VECTOR ( 'NONE', #1891, 1000.000000000000000 ) ;
#17318 = EDGE_CURVE ( 'NONE', #27401, #2214, #3000, .T. ) ;
#17319 = CARTESIAN_POINT ( 'NONE',  ( -13.14518615778179544, 35.79101562608393294, 0.000000000000000000 ) ) ;
#17320 = CARTESIAN_POINT ( 'NONE',  ( -18.00000000000000355, 80.00000000000000000, 13.00000000000000178 ) ) ;
#17321 = CARTESIAN_POINT ( 'NONE',  ( 101.0355339059327378, 122.4500000021849502, -2.499999999999997780 ) ) ;
#17322 = EDGE_CURVE ( 'NONE', #7547, #17145, #25088, .T. ) ;
#17323 = CARTESIAN_POINT ( 'NONE',  ( 55.81982418635200105, 50.00000000000001421, 14.99999999999998934 ) ) ;
#17324 = CIRCLE ( 'NONE', #47, 23.26794919243112858 ) ;
#17325 = CARTESIAN_POINT ( 'NONE',  ( 0.000000000000000000, 36.00000000000000000, -13.57481594606304576 ) ) ;
#17326 = VERTEX_POINT ( 'NONE', #18104 ) ;
#17327 = CARTESIAN_POINT ( 'NONE',  ( 98.15313185440925281, -4.458734124999987891, 9.625000001365593860 ) ) ;
#17328 = CARTESIAN_POINT ( 'NONE',  ( 97.50000000000000000, 122.6500000021849530, -1.035533905932742416 ) ) ;
#17329 = CARTESIAN_POINT ( 'NONE',  ( 95.54126587499995082, 1.846868145590750077, 12.37500000136559208 ) ) ;
#17330 = FACE_OUTER_BOUND ( 'NONE', #2500, .T. ) ;
#17331 = EDGE_CURVE ( 'NONE', #17145, #13309, #20681, .T. ) ;
#17332 = CARTESIAN_POINT ( 'NONE',  ( 13.14518615778179900, 40.20625000108393010, -5.444914386472297529 ) ) ;
#17333 = LINE ( 'NONE', #19897, #8566 ) ;
#17334 = CARTESIAN_POINT ( 'NONE',  ( 96.84719886470459471, 81.81250000136559208, 3.152801135295355994 ) ) ;
#17335 = CARTESIAN_POINT ( 'NONE',  ( 74.29505027212704249, 34.89804687608393863, -9.295050272127046043 ) ) ;
#17336 =( BOUNDED_SURFACE ( )  B_SPLINE_SURFACE ( 3, 2, ( 
 ( #4511, #15606, #6496 ),
 ( #22039, #4370, #13168 ),
 ( #4228, #24309, #12887 ),
 ( #17607, #21617, #26314 ),
 ( #15172, #2093, #2515 ),
 ( #10761, #8919, #28171 ),
 ( #23891, #11177, #15461 ),
 ( #19895, #4795, #13026 ),
 ( #15318, #13454, #21907 ),
 ( #17185, #21763, #2240 ),
 ( #2381, #24032, #11039 ),
 ( #19749, #232, #6775 ),
 ( #24176, #1095, #22890 ),
 ( #5080, #5221, #24740 ),
 ( #11601, #13602, #13886 ),
 ( #9762, #24884, #2931 ),
 ( #15749, #13742, #3355 ),
 ( #11463, #811, #26604 ),
 ( #20042, #7050, #666 ),
 ( #521, #22325, #5363 ) ),
 .UNSPECIFIED., .F., .F., .F. ) 
 B_SPLINE_SURFACE_WITH_KNOTS ( ( 4, 2, 2, 2, 2, 2, 2, 2, 2, 4 ),
 ( 3, 3 ),
 ( 0.009073803551359473779, 0.01139250602759182829, 0.01371120850382418453, 0.01602991098005654078, 0.01834861345628889528, 0.01950796469440507080, 0.02066731593252124979, 0.02298601840875360430, 0.02530472088498595881, 0.02762342336121831332 ),
 ( 0.000000000000000000, 1.000000000000000000 ),
 .UNSPECIFIED. ) 
 GEOMETRIC_REPRESENTATION_ITEM ( )  RATIONAL_B_SPLINE_SURFACE ( (
 ( 1.000000000000000000, 0.7071067811865476838, 1.000000000000000000),
 ( 1.000000000000000000, 0.7344871497827925033, 1.000000000000000000),
 ( 1.000000000000000000, 0.7612510203320145274, 1.000000000000000000),
 ( 1.000000000000000000, 0.8116663633842718939, 1.000000000000000000),
 ( 1.000000000000000000, 0.8353358059749915743, 1.000000000000000000),
 ( 1.000000000000000000, 0.8764699612587960598, 1.000000000000000000),
 ( 1.000000000000000000, 0.8939017358719169026, 1.000000000000000000),
 ( 1.000000000000000000, 0.9185314935647126422, 1.000000000000000000),
 ( 1.000000000000000000, 0.9256439951240776898, 1.000000000000000000),
 ( 1.000000000000000000, 0.9261623622475867457, 1.000000000000000000),
 ( 1.000000000000000000, 0.9246301385979069920, 1.000000000000000000),
 ( 1.000000000000000000, 0.9183304321347807164, 1.000000000000000000),
 ( 1.000000000000000000, 0.9135987334167550156, 1.000000000000000000),
 ( 1.000000000000000000, 0.8954110486041423345, 1.000000000000000000),
 ( 1.000000000000000000, 0.8779877431162668167, 1.000000000000000000),
 ( 1.000000000000000000, 0.8366182664710850592, 1.000000000000000000),
 ( 1.000000000000000000, 0.8126941604011834741, 1.000000000000000000),
 ( 1.000000000000000000, 0.7617527316309427032, 1.000000000000000000),
 ( 1.000000000000000000, 0.7347103785789421693, 1.000000000000000000),
 ( 1.000000000000000000, 0.7071067811865464625, 1.000000000000000000) ) ) 
 REPRESENTATION_ITEM ( '' )  SURFACE ( )  );
#17337 = CARTESIAN_POINT ( 'NONE',  ( 97.50236033167492167, 117.6869444889999841, -49.52500000273119696 ) ) ;
#17338 = CARTESIAN_POINT ( 'NONE',  ( 104.9999999999999716, 80.68750000273119838, -2.071067811865491937 ) ) ;
#17339 = CARTESIAN_POINT ( 'NONE',  ( 94.33688103937535629, 105.8855032339526758, -56.29999999453763593 ) ) ;
#17340 = CARTESIAN_POINT ( 'NONE',  ( 143.5748159460630688, 39.01562500000000000, -1.662435489736055892E-15 ) ) ;
#17341 = AXIS2_PLACEMENT_3D ( 'NONE', #42, #23982, #1911 ) ;
#17342 = ORIENTED_EDGE ( 'NONE', *, *, #15737, .T. ) ;
#17343 = CARTESIAN_POINT ( 'NONE',  ( 99.99999999999997158, 102.6397644303321215, -55.99999999453763877 ) ) ;
#17344 = CARTESIAN_POINT ( 'NONE',  ( -13.14518615778179544, 35.98945312608393721, 0.000000000000000000 ) ) ;
#17345 = CARTESIAN_POINT ( 'NONE',  ( 2.493653234604083739E-15, 38.91640625216786731, 13.57481594606304576 ) ) ;
#17346 = CARTESIAN_POINT ( 'NONE',  ( 124.5550856135277087, 36.43593750108392726, -13.14518615778179900 ) ) ;
#17347 = CARTESIAN_POINT ( 'NONE',  ( 70.62287287157788285, 32.61601562716786873, 13.57481594606304576 ) ) ;
#17348 = ADVANCED_FACE ( 'NONE', ( #9964 ), #18253, .T. ) ;
#17349 = CARTESIAN_POINT ( 'NONE',  ( 13.24545034676895305, 36.00000000000001421, 2.307131236159923215 ) ) ;
#17350 = CARTESIAN_POINT ( 'NONE',  ( 13.57481594606304931, 35.89023437716787868, 5.622872871577869525 ) ) ;
#17351 = CARTESIAN_POINT ( 'NONE',  ( 94.99999999999995737, -2.071067811865466624, 4.062499999999998224 ) ) ;
#17352 = CARTESIAN_POINT ( 'NONE',  ( -20.00000000000000355, 55.00000000000000000, -14.99999999999999822 ) ) ;
#17353 = EDGE_CURVE ( 'NONE', #3142, #1596, #1164, .T. ) ;
#17354 = CARTESIAN_POINT ( 'NONE',  ( 204.2950502721270425, 37.08085937608393579, -9.295050272127046043 ) ) ;
#17355 = CARTESIAN_POINT ( 'NONE',  ( 70.62287287157791127, 38.86679687500001279, 13.57481594606301023 ) ) ;
#17356 = EDGE_CURVE ( 'NONE', #13106, #5755, #24669, .T. ) ;
#17357 = SURFACE_SIDE_STYLE ('',( #21647 ) ) ;
#17358 = CARTESIAN_POINT ( 'NONE',  ( 195.0000000000000000, 38.12265625216787157, 13.57481594606304576 ) ) ;
#17359 = CARTESIAN_POINT ( 'NONE',  ( 1.662435489736055892E-15, 40.99999999999999289, 13.57481594606304576 ) ) ;
#17360 = CARTESIAN_POINT ( 'NONE',  ( 122.3760580380745324, 55.00000000000000711, 14.99999999999997158 ) ) ;
#17361 = CARTESIAN_POINT ( 'NONE',  ( 9.598844408820459861, 35.74140624999999716, 9.598844408820456309 ) ) ;
#17362 = CARTESIAN_POINT ( 'NONE',  ( 94.99999999999995737, 1.387778780781445676E-14, 12.12500000273118594 ) ) ;
#17363 = CARTESIAN_POINT ( 'NONE',  ( -13.14518615778179900, 35.93984375108393436, -5.444914386472297529 ) ) ;
#17364 = CARTESIAN_POINT ( 'NONE',  ( -13.14518615778179544, 39.75976562608393294, 0.000000000000000000 ) ) ;
#17365 = CARTESIAN_POINT ( 'NONE',  ( 181.4251840539369596, 33.06249999999999289, 0.000000000000000000 ) ) ;
#17366 = CARTESIAN_POINT ( 'NONE',  ( 104.9952793366501709, 116.8754121666685393, -46.07500000273119412 ) ) ;
#17367 = CARTESIAN_POINT ( 'NONE',  ( 107.0000000000000000, 110.0000000000000000, -51.49999999453763877 ) ) ;
#17368 = CARTESIAN_POINT ( 'NONE',  ( 59.55508561352770158, 34.35234375108392868, 13.14518615778179722 ) ) ;
#17369 = CARTESIAN_POINT ( 'NONE',  ( 101.8468681455907046, 4.458734125000016313, 2.125000001365591640 ) ) ;
#17370 = CARTESIAN_POINT ( 'NONE',  ( -5.622872871577920151, 35.69179687716787441, 13.57481594606300135 ) ) ;
#17371 = CARTESIAN_POINT ( 'NONE',  ( 99.99999999999998579, 92.06249999863440792, 4.458734124999981674 ) ) ;
#17372 = CARTESIAN_POINT ( 'NONE',  ( 103.5355339059327093, 3.535533905932755072, 4.624999999999999112 ) ) ;
#17373 = CARTESIAN_POINT ( 'NONE',  ( 9.598844408820459861, 35.74140624999999716, 9.598844408820456309 ) ) ;
#17374 = DIRECTION ( 'NONE',  ( -2.385244779468110248E-16, 0.000000000000000000, -1.000000000000000000 ) ) ;
#17375 = ORIENTED_EDGE ( 'NONE', *, *, #5970, .T. ) ;
#17376 = CARTESIAN_POINT ( 'NONE',  ( 102.0710678118654329, 83.31250000000000000, 4.999999999999989342 ) ) ;
#17377 = CARTESIAN_POINT ( 'NONE',  ( 103.1528011352953484, 92.43749999863440792, -3.152801135295366208 ) ) ;
#17378 = CARTESIAN_POINT ( 'NONE',  ( 13.57481594606304753, 34.30273437500000000, -5.622872871577873966 ) ) ;
#17379 = ORIENTED_EDGE ( 'NONE', *, *, #23264, .F. ) ;
#17380 = CARTESIAN_POINT ( 'NONE',  ( 93.00000000000000000, 107.7255621263696526, -46.90000000000001279 ) ) ;
#17381 = CARTESIAN_POINT ( 'NONE',  ( 78.14518615778179367, 34.79882812608394005, -1.609821015232357215E-15 ) ) ;
#17382 = ORIENTED_EDGE ( 'NONE', *, *, #971, .T. ) ;
#17383 = CARTESIAN_POINT ( 'NONE',  ( 107.0000000000000000, 110.0000000000000000, -145.0000000000000284 ) ) ;
#17384 = CARTESIAN_POINT ( 'NONE',  ( 104.4587341249999781, -1.846868145590721655, 4.125000001365592084 ) ) ;
#17385 = EDGE_CURVE ( 'NONE', #16078, #19393, #2759, .T. ) ;
#17386 = ORIENTED_EDGE ( 'NONE', *, *, #6000, .F. ) ;
#17387 = DIRECTION ( 'NONE',  ( 0.000000000000000000, 0.000000000000000000, -1.000000000000000000 ) ) ;
#17388 = CARTESIAN_POINT ( 'NONE',  ( -13.14518615778179900, 39.90859375108394147, -5.444914386472297529 ) ) ;
#17389 = CARTESIAN_POINT ( 'NONE',  ( 200.6228728715778686, 37.67617187716787441, -13.57481594606304753 ) ) ;
#17390 = CARTESIAN_POINT ( 'NONE',  ( -13.14518615778179189, 37.42812500108393436, 5.444914386472304635 ) ) ;
#17391 = DIRECTION ( 'NONE',  ( -1.000000000000000000, -0.000000000000000000, 2.385244779468110248E-16 ) ) ;
#17392 = CARTESIAN_POINT ( 'NONE',  ( 203.2596115289017291, 50.00000000056336091, 10.79618466885029093 ) ) ;
#17393 = EDGE_CURVE ( 'NONE', #26730, #15219, #11493, .T. ) ;
#17394 = CARTESIAN_POINT ( 'NONE',  ( 116.9040934463640156, 35.99999999999999289, 1.137167824541468031 ) ) ;
#17395 = ORIENTED_EDGE ( 'NONE', *, *, #1476, .F. ) ;
#17396 = CARTESIAN_POINT ( 'NONE',  ( -13.14518615778179900, 39.11484375108394573, -5.444914386472297529 ) ) ;
#17397 = CARTESIAN_POINT ( 'NONE',  ( 130.0000000000000000, 35.98945312608393010, 13.14518615778179544 ) ) ;
#17398 = CARTESIAN_POINT ( 'NONE',  ( 51.42518405393695957, 33.85624999999999574, 0.000000000000000000 ) ) ;
#17399 = CARTESIAN_POINT ( 'NONE',  ( 104.4587341249999781, 1.846868145590750299, 9.250000001365593860 ) ) ;
#17400 = CYLINDRICAL_SURFACE ( 'NONE', #18534, 7.000000000000006217 ) ;
#17401 = CARTESIAN_POINT ( 'NONE',  ( 104.4587341249999781, -1.846868145590721655, 1.875000001365591862 ) ) ;
#17402 = CARTESIAN_POINT ( 'NONE',  ( 91.91746824999998466, 107.3738262389971538, -51.02500000273119696 ) ) ;
#17403 = LINE ( 'NONE', #12962, #19997 ) ;
#17404 = DIRECTION ( 'NONE',  ( 0.000000000000000000, -1.000000000000000000, 0.000000000000000000 ) ) ;
#17405 = CARTESIAN_POINT ( 'NONE',  ( 108.0825317499999869, 107.3738262389971680, -48.72499999726881725 ) ) ;
#17406 = CARTESIAN_POINT ( 'NONE',  ( -13.14518615778179189, 36.03906250108394005, 5.444914386472304635 ) ) ;
#17407 = AXIS2_PLACEMENT_3D ( 'NONE', #14519, #23234, #8385 ) ;
#17408 = CARTESIAN_POINT ( 'NONE',  ( 93.46109445667489979, 114.7507929638356785, -48.07499999726882578 ) ) ;
#17409 = ORIENTED_EDGE ( 'NONE', *, *, #246, .F. ) ;
#17410 = DIRECTION ( 'NONE',  ( 0.000000000000000000, 0.000000000000000000, 1.000000000000000000 ) ) ;
#17411 = B_SPLINE_CURVE_WITH_KNOTS ( 'NONE', 3,
 ( #275, #24352, #9381, #2838, #11222, #856, #18228, #13504, #24647, #15653, #4983, #15506, #4550, #26502, #17650, #19793, #4843, #9246, #20371, #22224, #22084, #7097, #4695, #18078, #7381, #11363, #2561, #13211, #24498, #21945, #9528, #19940, #9105, #2423, #7237, #17938, #15795, #26649, #13650, #26937, #22507, #11506, #8962, #26792, #15928, #26358, #6816, #6958, #24216, #419, #17799, #5553, #3126, #16365 ),
 .UNSPECIFIED., .F., .F.,
 ( 4, 2, 2, 2, 2, 2, 2, 2, 2, 2, 2, 2, 2, 2, 2, 2, 2, 2, 2, 2, 2, 2, 2, 2, 2, 2, 4 ),
 ( 0.7500000000000000000, 0.8046875000000001110, 0.8320312500000005551, 0.8593750000000011102, 0.8867187500000015543, 0.9140625000000019984, 0.9414062500000025535, 0.9687500000000029976, 1.023437500000001332, 1.050781250000000444, 1.078124999999999778, 1.105468749999998890, 1.132812499999998002, 1.187499999999996447, 1.242187499999994893, 1.269531249999994005, 1.296874999999993339, 1.324218749999992450, 1.351562499999991562, 1.378906249999990674, 1.406249999999989786, 1.460937499999990452, 1.488281249999992006, 1.515624999999993783, 1.542968749999995115, 1.570312499999996891, 1.625000000000000000 ),
 .UNSPECIFIED. ) ;
#17412 = CARTESIAN_POINT ( 'NONE',  ( 130.0000000000000000, 36.93203125216787441, -13.57481594606304576 ) ) ;
#17413 = CYLINDRICAL_SURFACE ( 'NONE', #11670, 4.999999999999989342 ) ;
#17414 = CARTESIAN_POINT ( 'NONE',  ( 200.4449143864723055, 40.00781250108393294, 13.14518615778179189 ) ) ;
#17415 = ORIENTED_EDGE ( 'NONE', *, *, #9152, .F. ) ;
#17416 = CARTESIAN_POINT ( 'NONE',  ( 70.44491438647229131, 36.53515625108394715, -13.14518615778179722 ) ) ;
#17417 = FACE_OUTER_BOUND ( 'NONE', #2997, .T. ) ;
#17418 = DIRECTION ( 'NONE',  ( -0.8660254037844404840, -0.000000000000000000, -0.4999999999999967804 ) ) ;
#17419 = EDGE_LOOP ( 'NONE', ( #22812, #17908 ) ) ;
#17420 = CARTESIAN_POINT ( 'NONE',  ( 105.6631189606246295, 105.8855032339526758, -49.20000000000000995 ) ) ;
#17421 = CARTESIAN_POINT ( 'NONE',  ( -5.444914386472297529, 39.61093750108393152, -13.14518615778179900 ) ) ;
#17422 = CARTESIAN_POINT ( 'NONE',  ( 99.99999999999998579, 124.1500000010924651, 2.066987299999980099 ) ) ;
#17423 = AXIS2_PLACEMENT_3D ( 'NONE', #14724, #25575, #7907 ) ;
#17424 = CARTESIAN_POINT ( 'NONE',  ( 135.4449143864723055, 39.21406250108392300, 13.14518615778179189 ) ) ;
#17425 = CARTESIAN_POINT ( 'NONE',  ( -13.14518615778179722, 40.70234375108392300, -5.444914386472297529 ) ) ;
#17426 = CARTESIAN_POINT ( 'NONE',  ( 103.5355339059327235, 94.99999999726881583, -3.535533905932738197 ) ) ;
#17427 = CARTESIAN_POINT ( 'NONE',  ( 59.55508561352770158, 40.10703125108393152, 13.14518615778179722 ) ) ;
#17428 = LINE ( 'NONE', #26126, #15514 ) ;
#17429 = CARTESIAN_POINT ( 'NONE',  ( 181.8548138422182205, 35.19570312608393436, 0.000000000000000000 ) ) ;
#17430 = ORIENTED_EDGE ( 'NONE', *, *, #16124, .F. ) ;
#17431 = EDGE_LOOP ( 'NONE', ( #1066, #27370, #12449, #4069 ) ) ;
#17432 = VERTEX_POINT ( 'NONE', #11528 ) ;
#17433 = CARTESIAN_POINT ( 'NONE',  ( 13.14518615778179544, 39.56132812608393579, -1.609821015232357215E-15 ) ) ;
#17434 = CARTESIAN_POINT ( 'NONE',  ( 103.1528011352953342, -3.152801135295355106, 12.06250000136559208 ) ) ;
#17435 = CARTESIAN_POINT ( 'NONE',  ( 51.85481384221820633, 39.71015625108393010, -5.444914386472297529 ) ) ;
#17436 = CARTESIAN_POINT ( 'NONE',  ( 95.54126587499996504, 82.43750000136559208, -1.387778780781445676E-14 ) ) ;
#17437 = CARTESIAN_POINT ( 'NONE',  ( 181.8548138422182205, 39.71015625108393010, -5.444914386472297529 ) ) ;
#17438 = CARTESIAN_POINT ( 'NONE',  ( 5.444914386472302859, 39.41250000108393436, 13.14518615778179189 ) ) ;
#17439 = ADVANCED_FACE ( 'NONE', ( #7552 ), #1402, .T. ) ;
#17440 = CARTESIAN_POINT ( 'NONE',  ( -13.57481594606304576, 39.51171875216787299, 0.000000000000000000 ) ) ;
#17441 = LINE ( 'NONE', #17157, #21220 ) ;
#17442 = CARTESIAN_POINT ( 'NONE',  ( 106.5389055433250860, 105.2492070361643215, -52.82499999726881867 ) ) ;
#17443 = ORIENTED_EDGE ( 'NONE', *, *, #23954, .T. ) ;
#17444 = VECTOR ( 'NONE', #21225, 1000.000000000000000 ) ;
#17445 = CARTESIAN_POINT ( 'NONE',  ( -5.622872871577873077, 36.38632812499999858, 13.57481594606304753 ) ) ;
#17446 = CARTESIAN_POINT ( 'NONE',  ( -9.295050272127044266, 36.68398437608392726, 9.295050272127047819 ) ) ;
#17447 = CARTESIAN_POINT ( 'NONE',  ( 102.0710678118654329, 5.000000000000018652, 2.812500002731185944 ) ) ;
#17448 = CARTESIAN_POINT ( 'NONE',  ( 116.8548138422182205, 36.78320312608393294, 0.000000000000000000 ) ) ;
#17449 = CARTESIAN_POINT ( 'NONE',  ( 78.14518615778179367, 34.55078125108393294, 5.444914386472293977 ) ) ;
#17450 = CARTESIAN_POINT ( 'NONE',  ( 185.7049497278729575, 36.08867187608393579, 9.295050272127047819 ) ) ;
#17451 = DIRECTION ( 'NONE',  ( -0.000000000000000000, -0.000000000000000000, -1.000000000000000000 ) ) ;
#17452 =( BOUNDED_CURVE ( )  B_SPLINE_CURVE ( 2, ( #12783, #6389, #1980, #10649, #4253, #13052, #8664, #17355, #21788 ),
 .UNSPECIFIED., .F., .F. ) 
 B_SPLINE_CURVE_WITH_KNOTS ( ( 3, 2, 2, 2, 3 ),
 ( 0.1875000000000001388, 0.1979166666666667407, 0.2083333333333333703, 0.2187499999999999722, 0.2291666666666665741 ),
 .UNSPECIFIED. ) 
 CURVE ( )  GEOMETRIC_REPRESENTATION_ITEM ( )  RATIONAL_B_SPLINE_CURVE ( ( 0.9999999999999990008, 0.9238795325112877377, 1.000000000000000000, 0.9238795325112867385, 1.000000000000000000, 0.9238795325112867385, 1.000000000000000000, 0.9238795325112872936, 0.9999999999999994449 ) ) 
 REPRESENTATION_ITEM ( '' )  );
#17453 = CARTESIAN_POINT ( 'NONE',  ( 104.9999999999999574, 2.071067811865501263, 9.687500002731182391 ) ) ;
#17454 = CARTESIAN_POINT ( 'NONE',  ( 116.4251840539369454, 40.25585937716787299, -5.622872871577873077 ) ) ;
#17455 = DIRECTION ( 'NONE',  ( 0.000000000000000000, 1.000000000000000000, 0.000000000000000000 ) ) ;
#17456 = CARTESIAN_POINT ( 'NONE',  ( 5.444914386472302859, 36.03906250108394005, 13.14518615778179189 ) ) ;
#17457 = DIRECTION ( 'NONE',  ( 0.000000000000000000, 0.000000000000000000, 1.000000000000000000 ) ) ;
#17458 = CARTESIAN_POINT ( 'NONE',  ( 101.0355339059327378, 123.7500000021849615, 2.499999999999977796 ) ) ;
#17459 = CARTESIAN_POINT ( 'NONE',  ( -8.312177448680279460E-16, 36.13828125216787157, -13.57481594606304576 ) ) ;
#17460 = ORIENTED_EDGE ( 'NONE', *, *, #17313, .T. ) ;
#17461 = CARTESIAN_POINT ( 'NONE',  ( 101.8468681455906903, 4.458734125000016313, 7.125000001365591196 ) ) ;
#17462 = ORIENTED_EDGE ( 'NONE', *, *, #10203, .F. ) ;
#17463 = CARTESIAN_POINT ( 'NONE',  ( 100.8561741729129153, 124.3000000010924708, -2.066987299999999195 ) ) ;
#17464 = CARTESIAN_POINT ( 'NONE',  ( 104.4587341249999781, -1.846868145590721655, 12.87500000136559208 ) ) ;
#17465 = DIRECTION ( 'NONE',  ( 5.782411586589357392E-17, -0.000000000000000000, 1.000000000000000000 ) ) ;
#17466 = CARTESIAN_POINT ( 'NONE',  ( -8.049105076161786076E-16, 39.56132812608393579, -13.14518615778179544 ) ) ;
#17467 = FACE_OUTER_BOUND ( 'NONE', #635, .T. ) ;
#17468 = CARTESIAN_POINT ( 'NONE',  ( 101.8468681455906903, 82.00000000136560629, 4.458734124999987891 ) ) ;
#17469 = CARTESIAN_POINT ( 'NONE',  ( 78.14518615778179367, 34.00507812608393721, -1.609821015232357215E-15 ) ) ;
#17470 = CARTESIAN_POINT ( 'NONE',  ( 99.99999999999998579, 118.4984768113314004, -49.62500000273118417 ) ) ;
#17471 = CARTESIAN_POINT ( 'NONE',  ( 9.295050272127046043, 38.66835937608393436, -9.295050272127046043 ) ) ;
#17472 = EDGE_CURVE ( 'NONE', #12585, #17231, #15148, .T. ) ;
#17473 = DIRECTION ( 'NONE',  ( 0.000000000000000000, -1.000000000000000000, 0.000000000000000000 ) ) ;
#17474 = DIRECTION ( 'NONE',  ( -0.000000000000000000, -1.000000000000000000, -0.000000000000000000 ) ) ;
#17475 = CARTESIAN_POINT ( 'NONE',  ( 106.9999999999999716, 112.2744378736303759, -49.90000000000000568 ) ) ;
#17476 = CARTESIAN_POINT ( 'NONE',  ( 124.3771271284221314, 38.46992187499999716, -13.57481594606304753 ) ) ;
#17477 = MANIFOLD_SOLID_BREP ( 'Thread1', #3980 ) ;
#17478 = ORIENTED_EDGE ( 'NONE', *, *, #15375, .T. ) ;
#17479 = CARTESIAN_POINT ( 'NONE',  ( 104.9999999999999716, 1.449011120738813565E-14, 8.499999999999998224 ) ) ;
#17480 = EDGE_CURVE ( 'NONE', #8513, #12423, #14416, .T. ) ;
#17481 = CARTESIAN_POINT ( 'NONE',  ( -5.444914386472299306, 35.34453125108393579, 13.14518615778179722 ) ) ;
#17482 = CARTESIAN_POINT ( 'NONE',  ( 13.57481594606304931, 37.47773437716787726, 5.622872871577869525 ) ) ;
#17483 = CARTESIAN_POINT ( 'NONE',  ( 120.7049497278729575, 36.68398437608392726, 9.295050272127047819 ) ) ;
#17484 = CARTESIAN_POINT ( 'NONE',  ( 78.57481594606305464, 33.55859375216787299, -1.662435489736055892E-15 ) ) ;
#17485 = ORIENTED_EDGE ( 'NONE', *, *, #3729, .F. ) ;
#17486 = FACE_OUTER_BOUND ( 'NONE', #493, .T. ) ;
#17487 = CARTESIAN_POINT ( 'NONE',  ( 9.598844408820456309, 32.86406250216787583, -9.598844408820458085 ) ) ;
#17488 = CARTESIAN_POINT ( 'NONE',  ( 96.46446609406721961, -3.535533905932727539, 4.124999999999998224 ) ) ;
#17489 = EDGE_CURVE ( 'NONE', #22555, #16261, #18089, .T. ) ;
#17490 = CARTESIAN_POINT ( 'NONE',  ( 97.50236033167490746, 117.6869444889999841, -46.27499999726882152 ) ) ;
#17491 = CONICAL_SURFACE ( 'NONE', #8851, 25.00000000000001066, 0.9599310885968833640 ) ;
#17492 = CARTESIAN_POINT ( 'NONE',  ( 200.4449143864723055, 33.65781250108393152, 13.14518615778179189 ) ) ;
#17493 = CARTESIAN_POINT ( 'NONE',  ( 2.493653234604083739E-15, 34.15390625216787157, 13.57481594606304576 ) ) ;
#17494 = PRESENTATION_STYLE_ASSIGNMENT (( #22071 ) ) ;
#17495 = ORIENTED_EDGE ( 'NONE', *, *, #16104, .F. ) ;
#17496 =( BOUNDED_CURVE ( )  B_SPLINE_CURVE ( 2, ( #8680, #17370, #15213, #11082, #16074, #20086, #5120, #11647, #13356 ),
 .UNSPECIFIED., .F., .F. ) 
 B_SPLINE_CURVE_WITH_KNOTS ( ( 3, 2, 2, 2, 3 ),
 ( 0.4791666666666667962, 0.4895833333333333703, 0.5000000000000000000, 0.5104166666666665186, 0.5208333333333332593 ),
 .UNSPECIFIED. ) 
 CURVE ( )  GEOMETRIC_REPRESENTATION_ITEM ( )  RATIONAL_B_SPLINE_CURVE ( ( 0.9999999999999992228, 0.9238795325112875156, 1.000000000000000000, 0.9238795325112867385, 1.000000000000000000, 0.9238795325112867385, 1.000000000000000000, 0.9238795325112875156, 0.9999999999999992228 ) ) 
 REPRESENTATION_ITEM ( '' )  );
#17497 = CARTESIAN_POINT ( 'NONE',  ( 94.99999999999995737, 84.12500000273119838, -1.387778780781445676E-14 ) ) ;
#17498 = DIRECTION ( 'NONE',  ( 0.000000000000000000, 0.000000000000000000, -1.000000000000000000 ) ) ;
#17499 = CARTESIAN_POINT ( 'NONE',  ( -8.312177448680279460E-16, 37.62656249999999858, -13.57481594606304576 ) ) ;
#17500 = CARTESIAN_POINT ( 'NONE',  ( 143.5748159460630688, 38.22187499999999716, -1.662435489736055892E-15 ) ) ;
#17501 = CARTESIAN_POINT ( 'NONE',  ( -5.444914386472297529, 38.22187500108393010, -13.14518615778179900 ) ) ;
#17502 = CARTESIAN_POINT ( 'NONE',  ( -5.444914386472299306, 35.93984375108392726, 13.14518615778179722 ) ) ;
#17503 = CARTESIAN_POINT ( 'NONE',  ( 208.5748159460630120, 34.99726562500000426, 5.622872871577869525 ) ) ;
#17504 = CARTESIAN_POINT ( 'NONE',  ( 97.50236033167492167, 117.6869444889999841, -45.77500000273119696 ) ) ;
#17505 = CARTESIAN_POINT ( 'NONE',  ( 101.1086910246750250, 117.0000000187143314, -45.05125428434656243 ) ) ;
#17506 = CARTESIAN_POINT ( 'NONE',  ( 74.29505027212704249, 35.29492187608393294, 9.295050272127046043 ) ) ;
#17507 = CARTESIAN_POINT ( 'NONE',  ( 98.15313185440923860, -4.458734124999987891, 2.625000001365592084 ) ) ;
#17508 = CARTESIAN_POINT ( 'NONE',  ( 107.0000000000000142, 112.2744378736303332, -45.40000000546235981 ) ) ;
#17509 = CARTESIAN_POINT ( 'NONE',  ( 101.8468681455907330, 95.12499999863439371, 4.458734124999979898 ) ) ;
#17510 = EDGE_CURVE ( 'NONE', #21036, #11286, #1708, .T. ) ;
#17511 = LINE ( 'NONE', #17652, #20280 ) ;
#17512 = CARTESIAN_POINT ( 'NONE',  ( -5.622872871577873077, 35.29492187500000000, -13.57481594606304753 ) ) ;
#17513 = CARTESIAN_POINT ( 'NONE',  ( 139.2950502721270425, 36.48554687608393721, -9.295050272127046043 ) ) ;
#17514 = ORIENTED_EDGE ( 'NONE', *, *, #6175, .T. ) ;
#17515 = CARTESIAN_POINT ( 'NONE',  ( 96.84719886470459471, 79.81250000136559208, 3.152801135295355994 ) ) ;
#17516 = AXIS2_PLACEMENT_3D ( 'NONE', #17778, #26481, #4389 ) ;
#17517 = CARTESIAN_POINT ( 'NONE',  ( 97.92893218813451028, 81.93750000273118417, -5.000000000000018652 ) ) ;
#17518 = CARTESIAN_POINT ( 'NONE',  ( 101.8468681455907330, 94.12499999863439371, 4.458734124999979898 ) ) ;
#17519 = CARTESIAN_POINT ( 'NONE',  ( 61.57977918782911786, 35.99999999999998579, -13.02105590829194348 ) ) ;
#17520 = ADVANCED_FACE ( 'NONE', ( #17635 ), #26344, .F. ) ;
#17521 = CARTESIAN_POINT ( 'NONE',  ( 94.33688103937535629, 105.8855032339526758, -48.80000000000001137 ) ) ;
#17522 = CARTESIAN_POINT ( 'NONE',  ( 65.00000000000000000, 35.39414062608393863, 13.14518615778179544 ) ) ;
#17523 =( REPRESENTATION_RELATIONSHIP ('NONE','NONE', #2411, #19878 ) REPRESENTATION_RELATIONSHIP_WITH_TRANSFORMATION ( #22967 )SHAPE_REPRESENTATION_RELATIONSHIP( ) );
#17524 = ORIENTED_EDGE ( 'NONE', *, *, #15055, .F. ) ;
#17525 = CARTESIAN_POINT ( 'NONE',  ( 5.622872871577870413, 32.91367187716787157, -13.57481594606304753 ) ) ;
#17526 = CARTESIAN_POINT ( 'NONE',  ( 103.1528011352953342, -3.152801135295355106, 4.062500001365592084 ) ) ;
#17527 = ORIENTED_EDGE ( 'NONE', *, *, #3170, .T. ) ;
#17528 = CARTESIAN_POINT ( 'NONE',  ( -13.14518615778179544, 35.19570312608393436, 0.000000000000000000 ) ) ;
#17529 = CARTESIAN_POINT ( 'NONE',  ( -9.295050272127044266, 38.46992187608393721, 9.295050272127047819 ) ) ;
#17530 = UNCERTAINTY_MEASURE_WITH_UNIT (LENGTH_MEASURE( 1.000000000000000082E-05 ), #13440, 'distance_accuracy_value', 'NONE');
#17531 = CARTESIAN_POINT ( 'NONE',  ( 208.5748159460630120, 34.40195312716787157, -5.622872871577873077 ) ) ;
#17532 = CARTESIAN_POINT ( 'NONE',  ( -13.14518615778179544, 34.99726562608393721, 0.000000000000000000 ) ) ;
#17533 = CARTESIAN_POINT ( 'NONE',  ( 5.622872871577946796, 36.58476562716786873, 13.57481594606297115 ) ) ;
#17534 = CARTESIAN_POINT ( 'NONE',  ( 131.1371678245417627, 36.00000000000000000, 13.09590655363595602 ) ) ;
#17535 = CARTESIAN_POINT ( 'NONE',  ( 5.444914386472302859, 37.82500000108392868, 13.14518615778179189 ) ) ;
#17536 = CARTESIAN_POINT ( 'NONE',  ( 124.5550856135277087, 34.84843750108393579, -13.14518615778179900 ) ) ;
#17537 = CARTESIAN_POINT ( 'NONE',  ( 78.57481594606304043, 35.09648437499998863, -5.622872871577873077 ) ) ;
#17538 = DIRECTION ( 'NONE',  ( -0.000000000000000000, 1.000000000000000000, -0.000000000000000000 ) ) ;
#17539 = CARTESIAN_POINT ( 'NONE',  ( 96.84719886470459471, 3.152801135295383084, 10.56250000136559208 ) ) ;
#17540 = CARTESIAN_POINT ( 'NONE',  ( 208.0420085811496733, 36.00000000000001421, -3.640726557254588158 ) ) ;
#17541 = CARTESIAN_POINT ( 'NONE',  ( 104.4587341249999781, -1.846868145590721655, 12.87500000136559208 ) ) ;
#17542 = CARTESIAN_POINT ( 'NONE',  ( 91.91746824999998466, 112.6261737610028320, -49.22500000273119269 ) ) ;
#17543 = DIRECTION ( 'NONE',  ( 0.000000000000000000, 0.000000000000000000, 1.000000000000000000 ) ) ;
#17544 = VECTOR ( 'NONE', #20541, 1000.000000000000000 ) ;
#17545 = AXIS2_PLACEMENT_3D ( 'NONE', #23483, #25342, #6097 ) ;
#17546 = DIRECTION ( 'NONE',  ( 0.000000000000000000, 0.000000000000000000, -1.000000000000000000 ) ) ;
#17547 = CARTESIAN_POINT ( 'NONE',  ( 91.91746824999998466, 110.0000000000000000, -51.62499999726882294 ) ) ;
#17548 = CARTESIAN_POINT ( 'NONE',  ( 9.295050272127047819, 35.49335937608393721, 9.295050272127046043 ) ) ;
#17549 = CARTESIAN_POINT ( 'NONE',  ( 108.0825317500000011, 110.0000000000000000, -50.87499999726882294 ) ) ;
#17550 = VERTEX_POINT ( 'NONE', #11349 ) ;
#17551 = CARTESIAN_POINT ( 'NONE',  ( 99.20899822134843760, 123.0000000000000000, -1.909647267044714436 ) ) ;
#17552 = LINE ( 'NONE', #6717, #8416 ) ;
#17553 = DIRECTION ( 'NONE',  ( -0.000000000000000000, 1.000000000000000000, -0.000000000000000000 ) ) ;
#17554 = EDGE_CURVE ( 'NONE', #27581, #2056, #24630, .T. ) ;
#17555 = CARTESIAN_POINT ( 'NONE',  ( 189.5550856135277229, 40.40468750108393436, -13.14518615778179900 ) ) ;
#17556 = EDGE_LOOP ( 'NONE', ( #24719, #13357, #25885, #27277, #7641, #4046 ) ) ;
#17557 = CARTESIAN_POINT ( 'NONE',  ( 78.14518615778180788, 36.33671875108393579, 5.444914386472293977 ) ) ;
#17558 = DIRECTION ( 'NONE',  ( -1.000000000000000000, 0.000000000000000000, 0.000000000000000000 ) ) ;
#17559 = CARTESIAN_POINT ( 'NONE',  ( 65.84210759546466818, 53.50112910130383881, -15.00000000000000000 ) ) ;
#17560 = EDGE_LOOP ( 'NONE', ( #17162, #13834, #19246, #2994 ) ) ;
#17561 = CARTESIAN_POINT ( 'NONE',  ( 95.67376207875072680, 104.0454443415356991, -53.70000000000000284 ) ) ;
#17562 = CARTESIAN_POINT ( 'NONE',  ( 13.14518615778179900, 40.20625000108393010, -5.444914386472297529 ) ) ;
#17563 = CARTESIAN_POINT ( 'NONE',  ( 99.14382582708707048, 124.6000000010924822, -2.066987299999999195 ) ) ;
#17564 = CARTESIAN_POINT ( 'NONE',  ( 139.5988444088204403, 32.07031250216787299, -9.598844408820458085 ) ) ;
#17565 = DIRECTION ( 'NONE',  ( 0.000000000000000000, 0.000000000000000000, 1.000000000000000000 ) ) ;
#17566 = CARTESIAN_POINT ( 'NONE',  ( 104.9999999999999716, 94.93749999726880162, -2.071067811865478170 ) ) ;
#17567 = CARTESIAN_POINT ( 'NONE',  ( 59.55508561352770158, 36.93203125108394147, 13.14518615778179722 ) ) ;
#17568 = CARTESIAN_POINT ( 'NONE',  ( 99.99999999999995737, 80.00000000000000000, -5.000000000000018652 ) ) ;
#17569 = CARTESIAN_POINT ( 'NONE',  ( 200.4449143864723055, 35.44375000108393436, 13.14518615778179189 ) ) ;
#17570 = ORIENTED_EDGE ( 'NONE', *, *, #11777, .F. ) ;
#17571 = VERTEX_POINT ( 'NONE', #18355 ) ;
#17572 = CARTESIAN_POINT ( 'NONE',  ( -9.295050272127046043, 39.85898437608393152, -9.295050272127046043 ) ) ;
#17573 = DIRECTION ( 'NONE',  ( 1.000000000000000000, 0.000000000000000000, 0.000000000000000000 ) ) ;
#17574 = CARTESIAN_POINT ( 'NONE',  ( 95.54126587499996504, 1.846868145590750077, 9.625000001365593860 ) ) ;
#17575 = AXIS2_PLACEMENT_3D ( 'NONE', #4014, #19115, #4155 ) ;
#17576 = CARTESIAN_POINT ( 'NONE',  ( 5.622872871577786924, 38.07304687499999574, 13.57481594606313813 ) ) ;
#17577 = CARTESIAN_POINT ( 'NONE',  ( 104.4587341249999781, 79.87500000136560629, 1.846868145590721655 ) ) ;
#17578 = CARTESIAN_POINT ( 'NONE',  ( 181.8548138422182205, 38.22187500108393721, 5.444914386472304635 ) ) ;
#17579 = CARTESIAN_POINT ( 'NONE',  ( -9.295050272127044266, 39.26367187608393294, 9.295050272127047819 ) ) ;
#17580 = CARTESIAN_POINT ( 'NONE',  ( 2.493653234604083739E-15, 39.71015625216787015, 13.57481594606304576 ) ) ;
#17581 = AXIS2_PLACEMENT_3D ( 'NONE', #16862, #10436, #18859 ) ;
#17582 = CARTESIAN_POINT ( 'NONE',  ( 96.46446609406721961, -3.535533905932727539, 12.12500000000000000 ) ) ;
#17583 = CYLINDRICAL_SURFACE ( 'NONE', #6361, 13.57481594606304398 ) ;
#17584 = CARTESIAN_POINT ( 'NONE',  ( 99.99999999999997158, 101.5015231886685854, -53.12499999726883004 ) ) ;
#17585 = ORIENTED_EDGE ( 'NONE', *, *, #2308, .F. ) ;
#17586 = CARTESIAN_POINT ( 'NONE',  ( -5.622872871577873077, 37.97382812499999716, 13.57481594606304753 ) ) ;
#17587 = CARTESIAN_POINT ( 'NONE',  ( -13.14518615778179544, 35.79101562608393294, 0.000000000000000000 ) ) ;
#17588 = VERTEX_POINT ( 'NONE', #26921 ) ;
#17589 = CARTESIAN_POINT ( 'NONE',  ( 143.1451861577818079, 37.18007812608393436, -1.609821015232357215E-15 ) ) ;
#17590 = CARTESIAN_POINT ( 'NONE',  ( 55.70494972787295751, 33.50898437608393010, 9.295050272127047819 ) ) ;
#17591 = CARTESIAN_POINT ( 'NONE',  ( 208.1451861577817795, 36.33671875108394289, 5.444914386472293977 ) ) ;
#17592 = VERTEX_POINT ( 'NONE', #9232 ) ;
#17593 = CARTESIAN_POINT ( 'NONE',  ( 99.99999999999998579, 95.12499999726881583, -4.999999999999997335 ) ) ;
#17594 = CARTESIAN_POINT ( 'NONE',  ( 9.295050272127046043, 33.90585937608393152, -9.295050272127046043 ) ) ;
#17595 = CARTESIAN_POINT ( 'NONE',  ( 131.1387681171055419, 50.00000000043814907, -13.56816686242498271 ) ) ;
#17596 = CARTESIAN_POINT ( 'NONE',  ( 13.57481594606304576, 39.01562500000000000, -1.662435489736055892E-15 ) ) ;
#17597 = CARTESIAN_POINT ( 'NONE',  ( 124.3771271284221314, 40.15664062716787441, -13.57481594606304753 ) ) ;
#17598 = CARTESIAN_POINT ( 'NONE',  ( 0.000000000000000000, 30.99999999999999645, 0.000000000000000000 ) ) ;
#17599 = ADVANCED_FACE ( 'NONE', ( #14201 ), #7223, .F. ) ;
#17600 = CARTESIAN_POINT ( 'NONE',  ( 99.99999999999995737, 1.387778780781445676E-14, 15.00000000000000000 ) ) ;
#17601 = CARTESIAN_POINT ( 'NONE',  ( 102.4999999999999716, 123.8500000021849416, 1.035533905932722876 ) ) ;
#17602 = CARTESIAN_POINT ( 'NONE',  ( -13.57481594606304753, 36.28710937716787299, -5.622872871577872189 ) ) ;
#17603 =( LENGTH_UNIT ( ) NAMED_UNIT ( * ) SI_UNIT ( .MILLI., .METRE. ) );
#17604 = CARTESIAN_POINT ( 'NONE',  ( 103.1528011352953342, 3.152801135295383084, 9.062500001365592084 ) ) ;
#17605 = CARTESIAN_POINT ( 'NONE',  ( 98.23223304703363112, 123.4000000021849530, -1.767766952966370209 ) ) ;
#17606 = CARTESIAN_POINT ( 'NONE',  ( 98.15313185440925281, -4.458734124999987891, 12.62500000136559208 ) ) ;
#17607 = CARTESIAN_POINT ( 'NONE',  ( 122.8845096081448816, 49.99999999945637796, 11.58166858713987324 ) ) ;
#17608 = CARTESIAN_POINT ( 'NONE',  ( 9.295050272127047819, 40.05742187608392868, 9.295050272127046043 ) ) ;
#17609 = DIRECTION ( 'NONE',  ( -1.000000000000000000, 0.000000000000000000, 0.000000000000000000 ) ) ;
#17610 = CARTESIAN_POINT ( 'NONE',  ( 103.1528011352953342, 82.06250000136559208, 3.152801135295355106 ) ) ;
#17611 = CARTESIAN_POINT ( 'NONE',  ( 70.44491438647230552, 34.65000000108393863, 13.14518615778179189 ) ) ;
#17612 = CARTESIAN_POINT ( 'NONE',  ( 108.0825317500000153, 110.0000000000000000, -44.37500000273119838 ) ) ;
#17613 = CARTESIAN_POINT ( 'NONE',  ( 13.14518615778179722, 39.31328125108392868, 5.444914386472293977 ) ) ;
#17614 = AXIS2_PLACEMENT_3D ( 'NONE', #27780, #12639, #15057 ) ;
#17615 = DIRECTION ( 'NONE',  ( -0.000000000000000000, -1.000000000000000000, -0.000000000000000000 ) ) ;
#17616 = CYLINDRICAL_SURFACE ( 'NONE', #13577, 13.57481594606304398 ) ;
#17617 = CARTESIAN_POINT ( 'NONE',  ( 130.0000000000000000, 40.80156249999999574, -13.57481594606304576 ) ) ;
#17618 = CARTESIAN_POINT ( 'NONE',  ( 120.4011555911795455, 36.33671874999999574, 9.598844408820459861 ) ) ;
#17619 = MANIFOLD_SOLID_BREP ( 'Thread3', #23114 ) ;
#17620 = ORIENTED_EDGE ( 'NONE', *, *, #14982, .T. ) ;
#17621 = LINE ( 'NONE', #8931, #7727 ) ;
#17622 = CARTESIAN_POINT ( 'NONE',  ( 13.14518615778179900, 35.64218750108393152, -5.444914386472297529 ) ) ;
#17623 = CARTESIAN_POINT ( 'NONE',  ( 5.622872871577871301, 36.08867187716787583, -13.57481594606304753 ) ) ;
#17624 =( BOUNDED_CURVE ( )  B_SPLINE_CURVE ( 2, ( #2368, #18424, #20424, #22849, #21896, #18283, #9722, #26989, #24697 ),
 .UNSPECIFIED., .F., .F. ) 
 B_SPLINE_CURVE_WITH_KNOTS ( ( 3, 2, 2, 2, 3 ),
 ( 0.5833333333333337034, 0.6250000000000002220, 0.6666666666666667407, 0.7083333333333332593, 0.7499999999999997780 ),
 .UNSPECIFIED. ) 
 CURVE ( )  GEOMETRIC_REPRESENTATION_ITEM ( )  RATIONAL_B_SPLINE_CURVE ( ( 0.9999999999999994449, 0.9238795325112872936, 1.000000000000000000, 0.9238795325112867385, 1.000000000000000000, 0.9238795325112867385, 1.000000000000000000, 0.9238795325112871826, 0.9999999999999995559 ) ) 
 REPRESENTATION_ITEM ( '' )  );
#17625 = CARTESIAN_POINT ( 'NONE',  ( 139.2950502721270425, 37.08085937608393579, -9.295050272127046043 ) ) ;
#17626 = CARTESIAN_POINT ( 'NONE',  ( 55.40115559117954547, 34.65000000216787868, -9.598844408820458085 ) ) ;
#17627 = CARTESIAN_POINT ( 'NONE',  ( 9.031440422455050410, 35.99999999999997868, 9.765766397118351705 ) ) ;
#17628 = CARTESIAN_POINT ( 'NONE',  ( -8.049105076161786076E-16, 40.35507812608393152, -13.14518615778179544 ) ) ;
#17629 = CARTESIAN_POINT ( 'NONE',  ( 102.0710678118654329, -4.999999999999989342, 1.312499999999999556 ) ) ;
#17630 = CARTESIAN_POINT ( 'NONE',  ( 95.00472066334981491, 103.1245878333314465, -49.57499999726881157 ) ) ;
#17631 = CARTESIAN_POINT ( 'NONE',  ( 185.7049497278729575, 34.89804687608393152, -9.295050272127046043 ) ) ;
#17632 = VECTOR ( 'NONE', #10547, 1000.000000000000227 ) ;
#17633 = VECTOR ( 'NONE', #11981, 1000.000000000000000 ) ;
#17634 = DIRECTION ( 'NONE',  ( 0.000000000000000000, 0.000000000000000000, -1.000000000000000000 ) ) ;
#17635 = FACE_OUTER_BOUND ( 'NONE', #9150, .T. ) ;
#17637 = VERTEX_POINT ( 'NONE', #15912 ) ;
#17636 = CARTESIAN_POINT ( 'NONE',  ( 185.4011555911795597, 40.30546874999999574, 9.598844408820459861 ) ) ;
#17638 = ADVANCED_FACE ( 'NONE', ( #4971 ), #12568, .T. ) ;
#17639 = LINE ( 'NONE', #25919, #9507 ) ;
#17640 = CARTESIAN_POINT ( 'NONE',  ( 126.8834079195342355, 53.90895096933309105, 14.99999999999996803 ) ) ;
#17641 = CARTESIAN_POINT ( 'NONE',  ( -13.57481594606304753, 36.18789062499999432, -5.622872871577873077 ) ) ;
#17642 = CARTESIAN_POINT ( 'NONE',  ( -0.9955612250524552564, 35.99999999999999289, -13.45766439703027118 ) ) ;
#17643 = CARTESIAN_POINT ( 'NONE',  ( 5.444914386472297529, 37.32890625108393579, -13.14518615778179900 ) ) ;
#17644 = CARTESIAN_POINT ( 'NONE',  ( 5.444914386472297529, 36.33671875108394289, -13.14518615778179900 ) ) ;
#17645 = CARTESIAN_POINT ( 'NONE',  ( 181.4251840539369596, 34.60039062499999574, -5.622872871577873077 ) ) ;
#17646 = CARTESIAN_POINT ( 'NONE',  ( 97.50236033167492167, 102.3130555110000159, -46.97500000273119269 ) ) ;
#17647 = CARTESIAN_POINT ( 'NONE',  ( 143.5748159460630688, 36.63437499999999858, -1.662435489736055892E-15 ) ) ;
#17648 = CARTESIAN_POINT ( 'NONE',  ( 78.14518615778179367, 35.34453125108392868, 5.444914386472293977 ) ) ;
#17649 = CARTESIAN_POINT ( 'NONE',  ( 95.54126587499996504, -1.846868145590724986, 2.500000001365592084 ) ) ;
#17650 = CARTESIAN_POINT ( 'NONE',  ( 100.6274934504576777, 123.0000000000000000, -2.424672454047630321 ) ) ;
#17651 = ORIENTED_EDGE ( 'NONE', *, *, #7090, .T. ) ;
#17652 = CARTESIAN_POINT ( 'NONE',  ( 219.9999999999999716, 55.00000000000000000, 14.99999999999994316 ) ) ;
#17653 = CARTESIAN_POINT ( 'NONE',  ( 13.57481594606304576, 35.84062499999999574, -1.662435489736055892E-15 ) ) ;
#17654 = CARTESIAN_POINT ( 'NONE',  ( 120.7049497278729575, 37.67617187608393436, 9.295050272127047819 ) ) ;
#17655 = VERTEX_POINT ( 'NONE', #16766 ) ;
#17656 = ORIENTED_EDGE ( 'NONE', *, *, #22631, .F. ) ;
#17657 = CARTESIAN_POINT ( 'NONE',  ( 97.92893218813451028, 84.81250000000001421, -5.000000000000018652 ) ) ;
#17658 = CARTESIAN_POINT ( 'NONE',  ( 104.9999999999999574, 83.56250000273119838, 2.071067811865462627 ) ) ;
#17659 = CARTESIAN_POINT ( 'NONE',  ( 96.46446609406726225, 90.37500000000000000, -3.535533905932738197 ) ) ;
#17660 = CARTESIAN_POINT ( 'NONE',  ( 58.52943630333427194, 36.00000000000001421, -11.78199955157067436 ) ) ;
#17661 = CIRCLE ( 'NONE', #20872, 5.000000000000004441 ) ;
#17662 = ADVANCED_FACE ( 'NONE', ( #25467 ), #5945, .T. ) ;
#17663 = CARTESIAN_POINT ( 'NONE',  ( 99.99999999999997158, 102.6397644303321215, -48.50000000000000711 ) ) ;
#17664 = CARTESIAN_POINT ( 'NONE',  ( 78.14518615778179367, 32.46718750108393436, -5.444914386472297529 ) ) ;
#17665 = ORIENTED_EDGE ( 'NONE', *, *, #21004, .T. ) ;
#17666 = PLANE ( 'NONE',  #14030 ) ;
#17667 = CARTESIAN_POINT ( 'NONE',  ( 96.84719886470459471, -3.152801135295355994, 4.812500001365592084 ) ) ;
#17668 = ORIENTED_EDGE ( 'NONE', *, *, #6201, .F. ) ;
#17669 = CARTESIAN_POINT ( 'NONE',  ( 13.14518615778179544, 32.41757812608393863, -1.609821015232357215E-15 ) ) ;
#17670 =( BOUNDED_CURVE ( )  B_SPLINE_CURVE ( 2, ( #24183, #8786, #6642, #24042, #19758, #4518, #13176, #21915, #11049 ),
 .UNSPECIFIED., .F., .F. ) 
 B_SPLINE_CURVE_WITH_KNOTS ( ( 3, 2, 2, 2, 3 ),
 ( 0.4791666666666667962, 0.4895833333333333703, 0.5000000000000000000, 0.5104166666666665186, 0.5208333333333332593 ),
 .UNSPECIFIED. ) 
 CURVE ( )  GEOMETRIC_REPRESENTATION_ITEM ( )  RATIONAL_B_SPLINE_CURVE ( ( 0.9999999999999992228, 0.9238795325112875156, 1.000000000000000000, 0.9238795325112867385, 1.000000000000000000, 0.9238795325112867385, 1.000000000000000000, 0.9238795325112875156, 0.9999999999999992228 ) ) 
 REPRESENTATION_ITEM ( '' )  );
#17671 = CARTESIAN_POINT ( 'NONE',  ( 9.295050272127046043, 40.45429687608393721, -9.295050272127046043 ) ) ;
#17672 = CARTESIAN_POINT ( 'NONE',  ( 204.5988444088204403, 35.24531250216787726, -9.598844408820458085 ) ) ;
#17673 = EDGE_LOOP ( 'NONE', ( #22700, #24450, #26264 ) ) ;
#17674 = EDGE_CURVE ( 'NONE', #22175, #26480, #23330, .T. ) ;
#17675 = CARTESIAN_POINT ( 'NONE',  ( 13.14518615778179722, 37.72578125108393010, 5.444914386472293977 ) ) ;
#17676 = CARTESIAN_POINT ( 'NONE',  ( 204.5988444088204403, 36.03906250216787299, -9.598844408820458085 ) ) ;
#17677 = DIRECTION ( 'NONE',  ( 0.000000000000000000, 0.000000000000000000, 1.000000000000000000 ) ) ;
#17678 = VERTEX_POINT ( 'NONE', #21189 ) ;
#17679 = CARTESIAN_POINT ( 'NONE',  ( -5.444914386472297529, 36.63437500108393152, -13.14518615778179900 ) ) ;
#17680 = EDGE_CURVE ( 'NONE', #5755, #7831, #3704, .T. ) ;
#17681 = CARTESIAN_POINT ( 'NONE',  ( 124.5550856135277087, 34.35234375108392868, 13.14518615778179722 ) ) ;
#17682 = CARTESIAN_POINT ( 'NONE',  ( 70.62287287157788285, 34.89804687499999147, 13.57481594606304576 ) ) ;
#17683 = CARTESIAN_POINT ( 'NONE',  ( -5.622872871577873966, 34.79882812499999289, 13.57481594606304753 ) ) ;
#17684 = EDGE_CURVE ( 'NONE', #25472, #25494, #4221, .T. ) ;
#17685 = CIRCLE ( 'NONE', #20889, 7.000000000000006217 ) ;
#17686 = AXIS2_PLACEMENT_3D ( 'NONE', #27303, #12430, #16866 ) ;
#17687 = CARTESIAN_POINT ( 'NONE',  ( 96.84719886470459471, -3.152801135295355994, 11.81250000136559208 ) ) ;
#17688 = CYLINDRICAL_SURFACE ( 'NONE', #13033, 5.000000000000000000 ) ;
#17689 = CARTESIAN_POINT ( 'NONE',  ( 103.1528011352953342, 3.152801135295383084, 14.06250000136559208 ) ) ;
#17690 = CARTESIAN_POINT ( 'NONE',  ( 104.9952793366501851, 103.1245878333314323, -44.42500000273119554 ) ) ;
#17691 = AXIS2_PLACEMENT_3D ( 'NONE', #16062, #2690, #24770 ) ;
#17692 = LINE ( 'NONE', #19827, #7249 ) ;
#17693 = DIRECTION ( 'NONE',  ( -1.000000000000000000, 0.000000000000000000, 0.000000000000000000 ) ) ;
#17694 = CARTESIAN_POINT ( 'NONE',  ( 99.99999999999997158, 101.5015231886685712, -51.12499999726882294 ) ) ;
#17695 = CARTESIAN_POINT ( 'NONE',  ( 13.14518615778179544, 37.18007812608393436, -1.609821015232357215E-15 ) ) ;
#17696 = EDGE_CURVE ( 'NONE', #2410, #8127, #11377, .T. ) ;
#17697 = CARTESIAN_POINT ( 'NONE',  ( 97.83688103937537051, 103.3426043859339103, -48.09999999453764019 ) ) ;
#17698 = ORIENTED_EDGE ( 'NONE', *, *, #19426, .F. ) ;
#17699 = CARTESIAN_POINT ( 'NONE',  ( 101.4615807364564546, 123.4500000010924765, 1.461580736456455476 ) ) ;
#17700 = CARTESIAN_POINT ( 'NONE',  ( 99.14382582708708469, 123.1000000010924822, 2.066987299999979655 ) ) ;
#17701 = CARTESIAN_POINT ( 'NONE',  ( 99.37536711629694253, 123.0000000000000426, -2.000913270215707307 ) ) ;
#17702 = CARTESIAN_POINT ( 'NONE',  ( 208.1451861577818079, 37.77539062608393294, -1.609821015232357215E-15 ) ) ;
#17703 = ORIENTED_EDGE ( 'NONE', *, *, #8444, .F. ) ;
#17704 = CARTESIAN_POINT ( 'NONE',  ( 141.1048480505471332, 36.02027164848243501, -8.092840767093784748 ) ) ;
#17705 = CARTESIAN_POINT ( 'NONE',  ( 204.1801758136479918, 55.00000000000000000, -15.00000000000000000 ) ) ;
#17706 = CARTESIAN_POINT ( 'NONE',  ( 101.8468681455906903, -4.458734124999987891, 13.00000000136559386 ) ) ;
#17707 = EDGE_LOOP ( 'NONE', ( #10109, #5737, #25276, #15600, #16272, #20292, #14618, #13975, #19072, #22405, #27045, #13972, #2176, #26889, #6737, #5004, #13272 ) ) ;
#17708 = CARTESIAN_POINT ( 'NONE',  ( 91.91746824999999887, 110.0000000000000000, -51.37500000273119127 ) ) ;
#17709 = CARTESIAN_POINT ( 'NONE',  ( 13.14518615778179544, 40.15664062608393436, -1.609821015232357215E-15 ) ) ;
#17710 = COLOUR_RGB ( '', 0.40784314, 0.44705882, 0.49803922) ;
#17711 = CARTESIAN_POINT ( 'NONE',  ( 97.50000000000000000, 124.2500000000000000, 1.035533905932725096 ) ) ;
#17712 = AXIS2_PLACEMENT_3D ( 'NONE', #26103, #15104, #4447 ) ;
#17713 = CARTESIAN_POINT ( 'NONE',  ( 143.5748159460630404, 32.71523437716787441, 5.622872871577869525 ) ) ;
#17714 = CARTESIAN_POINT ( 'NONE',  ( -13.14518615778179189, 40.00781250108393294, 5.444914386472304635 ) ) ;
#17715 = CARTESIAN_POINT ( 'NONE',  ( 104.9999999999999858, 92.87499999726881583, -6.938893903907228378E-15 ) ) ;
#17716 = CARTESIAN_POINT ( 'NONE',  ( 65.00000000000000000, 38.56914062608393579, 13.14518615778179544 ) ) ;
#17717 = CARTESIAN_POINT ( 'NONE',  ( 61.36350375319361916, 51.46815297079188412, -14.99999999999999822 ) ) ;
#17718 = EDGE_CURVE ( 'NONE', #21855, #21025, #15491, .T. ) ;
#17719 = CARTESIAN_POINT ( 'NONE',  ( 208.5748159460630120, 40.65273437499998721, -5.622872871577873077 ) ) ;
#17720 = CARTESIAN_POINT ( 'NONE',  ( 114.9999999999999858, 100.0000000000000000, -15.00000000000000711 ) ) ;
#17721 = ORIENTED_EDGE ( 'NONE', *, *, #24980, .F. ) ;
#17722 = ORIENTED_EDGE ( 'NONE', *, *, #4953, .T. ) ;
#17723 = CARTESIAN_POINT ( 'NONE',  ( -9.295050272127046043, 39.06523437608392868, -9.295050272127046043 ) ) ;
#17724 = CARTESIAN_POINT ( 'NONE',  ( 103.1528011352953342, 3.152801135295383084, 9.312500001365593860 ) ) ;
#17725 = CARTESIAN_POINT ( 'NONE',  ( 101.7677669529663547, 124.7000000000000028, -1.767766952966370209 ) ) ;
#17726 = CARTESIAN_POINT ( 'NONE',  ( 55.40115559117954547, 36.43593750216787441, 9.598844408820459861 ) ) ;
#17727 = CARTESIAN_POINT ( 'NONE',  ( 181.8548138422182205, 38.17226562608393436, 0.000000000000000000 ) ) ;
#17728 = CARTESIAN_POINT ( 'NONE',  ( -9.295050272127046043, 38.27148437608393294, -9.295050272127046043 ) ) ;
#17729 = CARTESIAN_POINT ( 'NONE',  ( 0.000000000000000000, 36.00000000000000000, -13.57481594606304576 ) ) ;
#17730 = VECTOR ( 'NONE', #9711, 1000.000000000000000 ) ;
#17731 = CARTESIAN_POINT ( 'NONE',  ( 200.4449143864723055, 40.20625000108394431, 13.14518615778179189 ) ) ;
#17732 = CARTESIAN_POINT ( 'NONE',  ( 95.00472066334982912, 116.8754121666685393, -46.17499999726882720 ) ) ;
#17733 = ORIENTED_EDGE ( 'NONE', *, *, #7016, .F. ) ;
#17734 = CARTESIAN_POINT ( 'NONE',  ( 5.622872871577871301, 35.98945312499999716, -13.57481594606304753 ) ) ;
#17735 = CARTESIAN_POINT ( 'NONE',  ( 5.444914386472302859, 38.42031250108393436, 13.14518615778179189 ) ) ;
#17736 = ORIENTED_EDGE ( 'NONE', *, *, #3875, .F. ) ;
#17737 = CARTESIAN_POINT ( 'NONE',  ( 116.8548138422182205, 33.60820312608393579, 0.000000000000000000 ) ) ;
#17738 = CARTESIAN_POINT ( 'NONE',  ( 70.44491438647230552, 33.95546875108393436, -13.14518615778179900 ) ) ;
#17739 = CIRCLE ( 'NONE', #4093, 5.000000000000004441 ) ;
#17740 = CARTESIAN_POINT ( 'NONE',  ( 185.7049497278729575, 38.27148437608393294, -9.295050272127046043 ) ) ;
#17741 = ORIENTED_EDGE ( 'NONE', *, *, #8291, .T. ) ;
#17742 = FACE_OUTER_BOUND ( 'NONE', #22478, .T. ) ;
#17743 = CARTESIAN_POINT ( 'NONE',  ( -9.295050272127044266, 31.92148437608393508, 9.295050272127047819 ) ) ;
#17744 = CARTESIAN_POINT ( 'NONE',  ( 104.9999999999999716, 1.449011120738813565E-14, 1.625000002731184834 ) ) ;
#17745 = LINE ( 'NONE', #15307, #10393 ) ;
#17746 = CARTESIAN_POINT ( 'NONE',  ( 97.50000000000000000, 125.0000000000000000, -9.540979117872439019E-15 ) ) ;
#17747 = FACE_OUTER_BOUND ( 'NONE', #23804, .T. ) ;
#17748 = CARTESIAN_POINT ( 'NONE',  ( 97.50000000000000000, 124.3092387975100621, 0.1913417161825344548 ) ) ;
#17749 = CARTESIAN_POINT ( 'NONE',  ( 60.42840836746411526, 51.44262710532056815, 14.99999999999998046 ) ) ;
#17750 = CIRCLE ( 'NONE', #8657, 13.57481594606304576 ) ;
#17751 = ORIENTED_EDGE ( 'NONE', *, *, #24711, .T. ) ;
#17752 =( NAMED_UNIT ( * ) SI_UNIT ( $, .STERADIAN. ) SOLID_ANGLE_UNIT ( ) );
#17753 = VERTEX_POINT ( 'NONE', #4362 ) ;
#17754 = CARTESIAN_POINT ( 'NONE',  ( 103.1528011352953342, 3.152801135295383084, 10.06250000136559208 ) ) ;
#17755 = ORIENTED_EDGE ( 'NONE', *, *, #6379, .F. ) ;
#17756 = CARTESIAN_POINT ( 'NONE',  ( 100.8561741729129295, 124.0000000010925021, 2.066987299999979211 ) ) ;
#17757 = CARTESIAN_POINT ( 'NONE',  ( 99.99999999999995737, 4.458734125000016313, 8.187500001365592084 ) ) ;
#17758 = CARTESIAN_POINT ( 'NONE',  ( 65.00000000000000000, 37.72578125216787726, -13.57481594606304576 ) ) ;
#17759 = CARTESIAN_POINT ( 'NONE',  ( 13.14518615778179900, 36.13828125108393863, 5.444914386472293977 ) ) ;
#17760 = DIRECTION ( 'NONE',  ( 0.000000000000000000, 0.000000000000000000, 1.000000000000000000 ) ) ;
#17761 = CARTESIAN_POINT ( 'NONE',  ( 95.54126587499996504, 82.68750000136560629, -1.387778780781445676E-14 ) ) ;
#17762 = CARTESIAN_POINT ( 'NONE',  ( 51.85481384221820633, 36.78320312608393294, 0.000000000000000000 ) ) ;
#17763 = CARTESIAN_POINT ( 'NONE',  ( 106.5389055433251002, 114.7507929638356785, -51.92500000273119554 ) ) ;
#17764 = CARTESIAN_POINT ( 'NONE',  ( 13.14518615778179722, 36.23750000108393010, -5.444914386472297529 ) ) ;
#17765 = CARTESIAN_POINT ( 'NONE',  ( 99.99999999999995737, 80.87500000273119838, -5.000000000000018652 ) ) ;
#17766 = DIRECTION ( 'NONE',  ( 0.000000000000000000, 0.000000000000000000, 1.000000000000000000 ) ) ;
#17767 = CARTESIAN_POINT ( 'NONE',  ( 97.83688103937535629, 116.6573956140660897, -49.40000000000001279 ) ) ;
#17768 = CARTESIAN_POINT ( 'NONE',  ( 139.5988444088204687, 38.12265624999999858, 9.598844408820456309 ) ) ;
#17769 = ORIENTED_EDGE ( 'NONE', *, *, #25654, .F. ) ;
#17770 = CARTESIAN_POINT ( 'NONE',  ( 9.598844408820459861, 33.36015624999999574, 9.598844408820456309 ) ) ;
#17771 = CARTESIAN_POINT ( 'NONE',  ( 5.444914386472302859, 36.23750000108393721, 13.14518615778179189 ) ) ;
#17772 = CARTESIAN_POINT ( 'NONE',  ( -9.598844408820458085, 37.03125000216787299, -9.598844408820458085 ) ) ;
#17773 = CARTESIAN_POINT ( 'NONE',  ( 97.92893218813451028, 5.000000000000018652, 8.937500002731184168 ) ) ;
#17774 = CARTESIAN_POINT ( 'NONE',  ( 130.0000000000000000, 33.60820312608392868, 13.14518615778179544 ) ) ;
#17775 = CARTESIAN_POINT ( 'NONE',  ( 55.40115559117954547, 33.06250000216787299, -9.598844408820458085 ) ) ;
#17776 = CIRCLE ( 'NONE', #19581, 11.50000000000001776 ) ;
#17777 = VERTEX_POINT ( 'NONE', #11033 ) ;
#17778 = CARTESIAN_POINT ( 'NONE',  ( 99.99999999999995737, 85.00000000000000000, -1.387778780781445676E-14 ) ) ;
#17779 = CARTESIAN_POINT ( 'NONE',  ( 9.598844408820456309, 33.65781250216787157, -9.598844408820458085 ) ) ;
#17780 = DIRECTION ( 'NONE',  ( 3.469446951953614682E-16, 0.000000000000000000, 1.000000000000000000 ) ) ;
#17781 = CARTESIAN_POINT ( 'NONE',  ( 106.5389055433250860, 114.7507929638356785, -46.67499999726882720 ) ) ;
#17782 = CARTESIAN_POINT ( 'NONE',  ( 13.57481594606304753, 38.37070312716786447, -5.622872871577873077 ) ) ;
#17783 = CARTESIAN_POINT ( 'NONE',  ( 181.8548138422181921, 34.15390625108393863, -5.444914386472297529 ) ) ;
#17784 = PLANE ( 'NONE',  #15634 ) ;
#17785 = FILL_AREA_STYLE ('',( #11208 ) ) ;
#17786 = DIRECTION ( 'NONE',  ( 0.000000000000000000, 0.000000000000000000, 1.000000000000000000 ) ) ;
#17787 = DIRECTION ( 'NONE',  ( 1.000000000000000000, 0.000000000000000000, -5.782411586589357392E-17 ) ) ;
#17788 = CARTESIAN_POINT ( 'NONE',  ( 131.8875287258764217, 53.66306546785491349, 14.99999999999996447 ) ) ;
#17789 = CARTESIAN_POINT ( 'NONE',  ( 13.57481594606304576, 35.84062499999999574, -1.662435489736055892E-15 ) ) ;
#17790 =( BOUNDED_CURVE ( )  B_SPLINE_CURVE ( 2, ( #28173, #4513, #13170, #21909, #25262, #9733, #4798, #23137, #18714 ),
 .UNSPECIFIED., .F., .F. ) 
 B_SPLINE_CURVE_WITH_KNOTS ( ( 3, 2, 2, 2, 3 ),
 ( 0.8541666666666662966, 0.8645833333333331483, 0.8750000000000000000, 0.8854166666666667407, 0.8958333333333335924 ),
 .UNSPECIFIED. ) 
 CURVE ( )  GEOMETRIC_REPRESENTATION_ITEM ( )  RATIONAL_B_SPLINE_CURVE ( ( 1.000000000000002442, 0.9238795325112842960, 1.000000000000000000, 0.9238795325112867385, 1.000000000000000000, 0.9238795325112867385, 1.000000000000000000, 0.9238795325112850731, 1.000000000000001554 ) ) 
 REPRESENTATION_ITEM ( '' )  );
#17791 = CARTESIAN_POINT ( 'NONE',  ( 107.0000000000000000, 110.0000000000000000, -46.00000000000001421 ) ) ;
#17792 = CARTESIAN_POINT ( 'NONE',  ( 13.14518615778179900, 37.92421875108392726, 5.444914386472293977 ) ) ;
#17793 = CARTESIAN_POINT ( 'NONE',  ( 9.295050272127046043, 36.28710937608393294, -9.295050272127046043 ) ) ;
#17794 = CARTESIAN_POINT ( 'NONE',  ( 195.0000000000000000, 36.03906250000000000, -13.57481594606304576 ) ) ;
#17795 = CARTESIAN_POINT ( 'NONE',  ( 106.5389055433251002, 114.7507929638356785, -46.17500000273119554 ) ) ;
#17796 = CARTESIAN_POINT ( 'NONE',  ( 105.6631189606246295, 114.1144967660473242, -45.30000000546237970 ) ) ;
#17797 = CARTESIAN_POINT ( 'NONE',  ( 78.14518615778179367, 36.18789062608393436, -1.609821015232357215E-15 ) ) ;
#17798 = CARTESIAN_POINT ( 'NONE',  ( 101.8468681455907046, -4.458734124999987891, 1.750000001365591862 ) ) ;
#17799 = CARTESIAN_POINT ( 'NONE',  ( 100.9398115314949393, 123.0000000000000000, 2.320989078743034284 ) ) ;
#17800 = CARTESIAN_POINT ( 'NONE',  ( 99.99999999999998579, 93.62499999726881583, 4.999999999999984013 ) ) ;
#17801 = CARTESIAN_POINT ( 'NONE',  ( 13.57481594606304931, 37.37851562499999858, 5.622872871577869525 ) ) ;
#17802 = CARTESIAN_POINT ( 'NONE',  ( 124.5550856135277087, 38.51953125108393294, 13.14518615778179722 ) ) ;
#17803 = EDGE_LOOP ( 'NONE', ( #10678, #25718, #17382, #22862 ) ) ;
#17804 = CARTESIAN_POINT ( 'NONE',  ( 101.8468681455906903, 80.37500000136562051, -4.458734125000016313 ) ) ;
#17805 = EDGE_CURVE ( 'NONE', #9543, #15488, #18434, .T. ) ;
#17806 = CARTESIAN_POINT ( 'NONE',  ( 195.0000000000000000, -7.395377635281828788, -2.255140518769849538E-14 ) ) ;
#17807 = CARTESIAN_POINT ( 'NONE',  ( 94.99999999999995737, 81.18750000273119838, 2.071067811865466624 ) ) ;
#17808 = CARTESIAN_POINT ( 'NONE',  ( 104.4587341249999923, 94.37499999863440792, -1.846868145590737198 ) ) ;
#17809 = CARTESIAN_POINT ( 'NONE',  ( 98.15313185440925281, 95.24999999863437949, 4.458734124999979898 ) ) ;
#17810 = CARTESIAN_POINT ( 'NONE',  ( 92.99999999999998579, 110.0000000000000000, -47.00000000000001421 ) ) ;
#17811 = CARTESIAN_POINT ( 'NONE',  ( 55.70494972787295751, 31.92148437608393508, -9.295050272127046043 ) ) ;
#17812 = EDGE_LOOP ( 'NONE', ( #12485, #16092, #12936, #18654, #5531, #20027, #27363, #24548, #11760, #15117, #9824, #5865, #14953, #1620 ) ) ;
#17813 = CARTESIAN_POINT ( 'NONE',  ( 84.99999999999998579, 95.00000000000000000, 12.99999999999999467 ) ) ;
#17814 = CARTESIAN_POINT ( 'NONE',  ( 95.54126587499996504, 1.387778780781445676E-14, 0.6875000013655923059 ) ) ;
#17815 = ORIENTED_EDGE ( 'NONE', *, *, #20062, .T. ) ;
#17816 = CARTESIAN_POINT ( 'NONE',  ( -8.049105076161786076E-16, 35.79101562608394005, -13.14518615778179544 ) ) ;
#17817 = CARTESIAN_POINT ( 'NONE',  ( 200.6228728715778686, 35.29492187716788720, -13.57481594606304753 ) ) ;
#17818 = CARTESIAN_POINT ( 'NONE',  ( 13.14518615778179544, 33.80664062608393294, -1.609821015232357215E-15 ) ) ;
#17819 = DIRECTION ( 'NONE',  ( -0.000000000000000000, -0.000000000000000000, -1.000000000000000000 ) ) ;
#17820 = CARTESIAN_POINT ( 'NONE',  ( 139.2950502721270425, 36.28710937608393294, 9.295050272127046043 ) ) ;
#17821 = ORIENTED_EDGE ( 'NONE', *, *, #23765, .F. ) ;
#17822 = CARTESIAN_POINT ( 'NONE',  ( 13.14518615778179900, 34.05468750108394005, -5.444914386472297529 ) ) ;
#17823 = CARTESIAN_POINT ( 'NONE',  ( 95.67376207875072680, 104.0454443415356991, -50.20000000546238539 ) ) ;
#17824 = CARTESIAN_POINT ( 'NONE',  ( 74.59884440882045453, 34.35234374999999574, -9.598844408820458085 ) ) ;
#17825 = CARTESIAN_POINT ( 'NONE',  ( 102.0669872999999939, 124.3000000010924566, 0.8561741729129311862 ) ) ;
#17826 = CARTESIAN_POINT ( 'NONE',  ( 96.84719886470459471, -3.152801135295355994, 10.81250000136559208 ) ) ;
#17827 = DIRECTION ( 'NONE',  ( 0.000000000000000000, 0.000000000000000000, -1.000000000000000000 ) ) ;
#17828 = ADVANCED_FACE ( 'NONE', ( #15312 ), #21346, .T. ) ;
#17829 = CARTESIAN_POINT ( 'NONE',  ( 95.54126587499995082, 1.846868145590750077, 1.375000001365592972 ) ) ;
#17830 = CARTESIAN_POINT ( 'NONE',  ( 99.99999999999998579, 101.5015231886685854, -48.62500000273119838 ) ) ;
#17831 = CYLINDRICAL_SURFACE ( 'NONE', #2263, 11.57481594606304398 ) ;
#17832 = DIRECTION ( 'NONE',  ( 0.000000000000000000, 0.000000000000000000, 1.000000000000000000 ) ) ;
#17833 = CARTESIAN_POINT ( 'NONE',  ( 104.9952793366501567, 116.8754121666685393, -50.32499999726882578 ) ) ;
#17834 = CARTESIAN_POINT ( 'NONE',  ( -8.049105076161786076E-16, 34.99726562608393721, -13.14518615778179544 ) ) ;
#17835 = CARTESIAN_POINT ( 'NONE',  ( 93.00000000000000000, 112.2744378736303332, -48.59999999453763309 ) ) ;
#17836 = ORIENTED_EDGE ( 'NONE', *, *, #14737, .F. ) ;
#17837 = CARTESIAN_POINT ( 'NONE',  ( 97.93301270000000613, 124.7500000010924737, -9.540979117872439019E-15 ) ) ;
#17839 = EDGE_CURVE ( 'NONE', #15078, #15088, #10781, .T. ) ;
#17838 = CARTESIAN_POINT ( 'NONE',  ( 102.0669873000000081, 123.4000000010924794, -0.8561741729129508371 ) ) ;
#17840 = CARTESIAN_POINT ( 'NONE',  ( 0.000000000000000000, 40.99999999999999289, 0.000000000000000000 ) ) ;
#17841 = ADVANCED_FACE ( 'NONE', ( #804 ), #13319, .T. ) ;
#17842 =( BOUNDED_CURVE ( )  B_SPLINE_CURVE ( 2, ( #23020, #14302, #18737, #5916, #25017, #14165, #12432, #1779, #25288, #14582, #3634 ),
 .UNSPECIFIED., .F., .F. ) 
 B_SPLINE_CURVE_WITH_KNOTS ( ( 3, 2, 2, 2, 2, 3 ),
 ( 0.000000000000000000, 0.02000000000000000042, 0.04000000000000000083, 0.05999999999999999778, 0.08000000000000000167, 0.1000000000000000194 ),
 .UNSPECIFIED. ) 
 CURVE ( )  GEOMETRIC_REPRESENTATION_ITEM ( )  RATIONAL_B_SPLINE_CURVE ( ( 1.000000000000000000, 0.9510565162951535312, 1.000000000000000000, 0.9510565162951535312, 1.000000000000000000, 0.9510565162951535312, 1.000000000000000000, 0.9510565162951535312, 1.000000000000000000, 0.9510565162951535312, 1.000000000000000000 ) ) 
 REPRESENTATION_ITEM ( '' )  );
#17843 = CARTESIAN_POINT ( 'NONE',  ( 195.0000000000000000, 35.98945312608393010, 13.14518615778179544 ) ) ;
#17844 = ORIENTED_EDGE ( 'NONE', *, *, #23425, .F. ) ;
#17845 = DIRECTION ( 'NONE',  ( 0.000000000000000000, 0.000000000000000000, 1.000000000000000000 ) ) ;
#17846 = CARTESIAN_POINT ( 'NONE',  ( 104.4587341249999781, 1.846868145590750299, 11.25000000136559208 ) ) ;
#17847 = VERTEX_POINT ( 'NONE', #26930 ) ;
#17848 = CARTESIAN_POINT ( 'NONE',  ( 99.99999999999998579, 118.4984768113314004, -53.87500000273118417 ) ) ;
#17849 = CARTESIAN_POINT ( 'NONE',  ( 2.493653234604083739E-15, 33.36015625216786873, 13.57481594606304576 ) ) ;
#17850 = CARTESIAN_POINT ( 'NONE',  ( 98.23223304703363112, 123.2999999999999972, -1.767766952966370209 ) ) ;
#17851 = EDGE_CURVE ( 'NONE', #3596, #9781, #11325, .T. ) ;
#17852 = CARTESIAN_POINT ( 'NONE',  ( 143.1451861577818079, 40.10703125108393152, 5.444914386472293977 ) ) ;
#17853 = CARTESIAN_POINT ( 'NONE',  ( 13.14518615778179722, 39.51171875108393294, 5.444914386472293977 ) ) ;
#17854 = CARTESIAN_POINT ( 'NONE',  ( 95.00000000000000000, 95.31249999726880162, -2.071067811865479058 ) ) ;
#17855 = CARTESIAN_POINT ( 'NONE',  ( 51.85481384221820633, 38.37070312608393152, 0.000000000000000000 ) ) ;
#17856 = CARTESIAN_POINT ( 'NONE',  ( 61.19694562675306315, 54.09082899096448926, -14.99999999999999645 ) ) ;
#17857 = CARTESIAN_POINT ( 'NONE',  ( 97.50236033167492167, 117.6869444889999841, -51.77500000273119696 ) ) ;
#17858 = VECTOR ( 'NONE', #697, 1000.000000000000000 ) ;
#17859 = CARTESIAN_POINT ( 'NONE',  ( 185.7049497278729575, 32.71523437608393436, -9.295050272127046043 ) ) ;
#17860 = DIRECTION ( 'NONE',  ( 0.000000000000000000, 0.000000000000000000, 1.000000000000000000 ) ) ;
#17861 = ORIENTED_EDGE ( 'NONE', *, *, #12410, .F. ) ;
#17862 = CARTESIAN_POINT ( 'NONE',  ( 9.295050272127046043, 34.89804687608393863, -9.295050272127046043 ) ) ;
#17863 = CARTESIAN_POINT ( 'NONE',  ( 98.15313185440923860, 4.458734125000016313, 11.50000000136559208 ) ) ;
#17864 = CARTESIAN_POINT ( 'NONE',  ( 65.00000000000000000, 37.57695312608392868, 13.14518615778179544 ) ) ;
#17865 = EDGE_CURVE ( 'NONE', #9074, #26975, #7943, .T. ) ;
#17866 = CARTESIAN_POINT ( 'NONE',  ( 55.40115559117954547, 38.51953124999999289, -9.598844408820458085 ) ) ;
#17867 = CARTESIAN_POINT ( 'NONE',  ( 94.99999999999997158, -2.071067811865486608, 2.062499999999999556 ) ) ;
#17868 = ORIENTED_EDGE ( 'NONE', *, *, #17964, .F. ) ;
#17869 = CARTESIAN_POINT ( 'NONE',  ( 9.295050272127047819, 37.08085937608393579, 9.295050272127046043 ) ) ;
#17870 = ORIENTED_EDGE ( 'NONE', *, *, #6858, .F. ) ;
#17871 = CARTESIAN_POINT ( 'NONE',  ( 204.2950502721270425, 38.86679687608393863, -9.295050272127046043 ) ) ;
#17872 = CARTESIAN_POINT ( 'NONE',  ( 108.0825317499999869, 112.6261737610028320, -52.52499999726881441 ) ) ;
#17873 = VERTEX_POINT ( 'NONE', #10068 ) ;
#17874 = CARTESIAN_POINT ( 'NONE',  ( -9.598844408820454532, 33.95546874999999432, 9.598844408820459861 ) ) ;
#17875 = CARTESIAN_POINT ( 'NONE',  ( -13.14518615778179189, 34.25312500108393010, 5.444914386472304635 ) ) ;
#17876 = ORIENTED_EDGE ( 'NONE', *, *, #26252, .F. ) ;
#17877 = CARTESIAN_POINT ( 'NONE',  ( 124.5550856135277087, 32.16953125108393152, 13.14518615778179722 ) ) ;
#17878 = EDGE_CURVE ( 'NONE', #27159, #19876, #24255, .T. ) ;
#17879 = STYLED_ITEM ( 'NONE', ( #24298 ), #26591 ) ;
#17880 = CARTESIAN_POINT ( 'NONE',  ( 208.1451861577818079, 35.59257812608393579, -1.609821015232357215E-15 ) ) ;
#17881 = ORIENTED_EDGE ( 'NONE', *, *, #21122, .T. ) ;
#17882 = CARTESIAN_POINT ( 'NONE',  ( 94.99999999999995737, 1.387778780781445676E-14, 11.12500000273118594 ) ) ;
#17883 = SHAPE_REPRESENTATION ( 'connector', ( #26844 ), #20877 ) ;
#17884 = CARTESIAN_POINT ( 'NONE',  ( 13.14518615778179900, 33.06250000108393294, -5.444914386472297529 ) ) ;
#17885 = FACE_OUTER_BOUND ( 'NONE', #15520, .T. ) ;
#17886 = CARTESIAN_POINT ( 'NONE',  ( 70.62287287157788285, 40.45429687500001137, 13.57481594606306174 ) ) ;
#17887 = CARTESIAN_POINT ( 'NONE',  ( 108.0825317500000153, 110.0000000000000000, -52.12500000273119838 ) ) ;
#17888 = DIRECTION ( 'NONE',  ( 0.000000000000000000, 0.000000000000000000, 1.000000000000000000 ) ) ;
#17889 = CARTESIAN_POINT ( 'NONE',  ( 5.622872871578008080, 36.78320312499999289, -13.57481594606290898 ) ) ;
#17890 = CARTESIAN_POINT ( 'NONE',  ( 65.39699941464660071, 51.45716825712325715, 14.99999999999964118 ) ) ;
#17891 = ORIENTED_EDGE ( 'NONE', *, *, #19264, .F. ) ;
#17892 = CARTESIAN_POINT ( 'NONE',  ( 95.54126587499995082, 1.846868145590750077, 3.375000001365592972 ) ) ;
#17893 = ORIENTED_EDGE ( 'NONE', *, *, #6379, .T. ) ;
#17894 = CARTESIAN_POINT ( 'NONE',  ( 99.14382582708707048, 122.8000000010924708, -2.066987299999999195 ) ) ;
#17895 = CARTESIAN_POINT ( 'NONE',  ( 103.1528011352953342, -3.152801135295355106, 9.812500001365593860 ) ) ;
#17896 = CARTESIAN_POINT ( 'NONE',  ( 143.5748159460630688, 38.37070312716787157, -5.622872871577873966 ) ) ;
#17897 = CARTESIAN_POINT ( 'NONE',  ( -13.14518615778179900, 37.32890625108393579, -5.444914386472297529 ) ) ;
#17898 = DIRECTION ( 'NONE',  ( 0.000000000000000000, -0.000000000000000000, 1.000000000000000000 ) ) ;
#17899 = DIRECTION ( 'NONE',  ( 0.8660254037844418162, -0.4999999999999947264, 0.000000000000000000 ) ) ;
#17900 = CARTESIAN_POINT ( 'NONE',  ( 51.85481384221820633, 35.19570312608393436, 0.000000000000000000 ) ) ;
#17901 = CARTESIAN_POINT ( 'NONE',  ( 195.0000000000000000, 37.62656249999999858, -13.57481594606304576 ) ) ;
#17902 = CARTESIAN_POINT ( 'NONE',  ( 2.414731522848535132E-15, 38.37070312608393152, 13.14518615778179544 ) ) ;
#17903 = CARTESIAN_POINT ( 'NONE',  ( 13.57481594606304753, 35.19570312716787441, -5.622872871577873966 ) ) ;
#17904 = CARTESIAN_POINT ( 'NONE',  ( 7.089417272335208686, 49.99999999943681672, 11.59823041028890955 ) ) ;
#17905 = CARTESIAN_POINT ( 'NONE',  ( 104.3262379212492448, 115.9545556584642867, -55.19999999453763451 ) ) ;
#17906 = CARTESIAN_POINT ( 'NONE',  ( 135.6228728715778686, 37.57695312499998863, -13.57481594606304753 ) ) ;
#17907 = ORIENTED_EDGE ( 'NONE', *, *, #11234, .T. ) ;
#17908 = ORIENTED_EDGE ( 'NONE', *, *, #16579, .T. ) ;
#17909 = DIRECTION ( 'NONE',  ( -1.000000000000000000, 0.000000000000000000, 7.228014483236696740E-18 ) ) ;
#17910 = CARTESIAN_POINT ( 'NONE',  ( 9.295050272127047819, 37.87460937608393863, 9.295050272127046043 ) ) ;
#17911 = CARTESIAN_POINT ( 'NONE',  ( 2.493653234604083739E-15, 38.12265625216787157, 13.57481594606304576 ) ) ;
#17912 = CARTESIAN_POINT ( 'NONE',  ( 96.46446609406721961, -3.535533905932727539, 8.250000002731185944 ) ) ;
#17913 = CARTESIAN_POINT ( 'NONE',  ( 116.8548138422182205, 34.20351562608393436, 0.000000000000000000 ) ) ;
#17914 = CARTESIAN_POINT ( 'NONE',  ( 70.62287287157786864, 33.70742187716787441, -13.57481594606304753 ) ) ;
#17915 = CARTESIAN_POINT ( 'NONE',  ( 3.878385297391210518, 32.03609435653363136, -13.57481594606304576 ) ) ;
#17916 = CARTESIAN_POINT ( 'NONE',  ( 9.598844408820459861, 31.87187500216787228, 9.598844408820456309 ) ) ;
#17917 = CARTESIAN_POINT ( 'NONE',  ( 103.5355339059327093, 3.535533905932755072, 2.624999999999998668 ) ) ;
#17918 = AXIS2_PLACEMENT_3D ( 'NONE', #12462, #14198, #24908 ) ;
#17919 = CARTESIAN_POINT ( 'NONE',  ( 99.99999999999995737, 84.75000000000000000, -5.000000000000018652 ) ) ;
#17920 = CARTESIAN_POINT ( 'NONE',  ( 9.598844408820456309, 39.21406250216787015, -9.598844408820458085 ) ) ;
#17921 = CARTESIAN_POINT ( 'NONE',  ( 200.4449143864723055, 32.86406250108392868, 13.14518615778179189 ) ) ;
#17922 = CARTESIAN_POINT ( 'NONE',  ( -13.57481594606304576, 31.57421875216786944, 0.000000000000000000 ) ) ;
#17923 = CARTESIAN_POINT ( 'NONE',  ( 94.33688103937535629, 105.8855032339526758, -52.80000000000001137 ) ) ;
#17924 = CARTESIAN_POINT ( 'NONE',  ( 101.4615807364564546, 123.2500000010924879, 1.461580736456455476 ) ) ;
#17925 = CARTESIAN_POINT ( 'NONE',  ( 99.99999999999998579, 94.62499999726881583, 4.999999999999984013 ) ) ;
#17926 = CARTESIAN_POINT ( 'NONE',  ( 2.493653234604083739E-15, 35.64218749999999147, 13.57481594606304576 ) ) ;
#17927 = CARTESIAN_POINT ( 'NONE',  ( 92.45873412499997812, 110.0000000000000000, -55.31249999863442213 ) ) ;
#17928 = CARTESIAN_POINT ( 'NONE',  ( -5.622872871577873077, 36.88242187499999858, -13.57481594606304753 ) ) ;
#17929 = CARTESIAN_POINT ( 'NONE',  ( 139.1801758136479918, 50.00000000000000000, 9.999999999999976907 ) ) ;
#17930 = CARTESIAN_POINT ( 'NONE',  ( -5.444914386472299306, 32.96328125108393436, 13.14518615778179722 ) ) ;
#17931 = CARTESIAN_POINT ( 'NONE',  ( -13.14518615778179900, 34.94765625108392726, -5.444914386472297529 ) ) ;
#17932 = CARTESIAN_POINT ( 'NONE',  ( 208.5748159460630688, 33.45937499999999432, -1.662435489736055892E-15 ) ) ;
#17933 = CARTESIAN_POINT ( 'NONE',  ( -9.598844408820454532, 37.22968750216787726, 9.598844408820459861 ) ) ;
#17934 = CARTESIAN_POINT ( 'NONE',  ( 130.0000000000000000, -7.395377635281828788, -13.57481594606305997 ) ) ;
#17935 = CARTESIAN_POINT ( 'NONE',  ( 102.1631189606246295, 116.6573956140660897, -45.10000000546238397 ) ) ;
#17936 = CARTESIAN_POINT ( 'NONE',  ( 78.14518615778179367, 34.65000000108393152, -5.444914386472297529 ) ) ;
#17937 = CARTESIAN_POINT ( 'NONE',  ( 95.00000000000000000, 90.56249999999998579, 2.071067811865463959 ) ) ;
#17938 = CARTESIAN_POINT ( 'NONE',  ( 97.83149761400481736, 122.9999999999999716, 1.253061062422446970 ) ) ;
#17939 = ORIENTED_EDGE ( 'NONE', *, *, #6071, .T. ) ;
#17940 = CARTESIAN_POINT ( 'NONE',  ( 101.4615807364564546, 124.0500000010924850, 1.461580736456455476 ) ) ;
#17941 = CARTESIAN_POINT ( 'NONE',  ( 13.57481594606304576, 34.25312499999999716, -1.662435489736055892E-15 ) ) ;
#17942 = CARTESIAN_POINT ( 'NONE',  ( 143.1451861577818079, 37.13046875108393863, 5.444914386472293977 ) ) ;
#17943 = ORIENTED_EDGE ( 'NONE', *, *, #23943, .F. ) ;
#17944 = CARTESIAN_POINT ( 'NONE',  ( 99.99999999999995737, 82.25000000000000000, 4.999999999999990230 ) ) ;
#17945 = DIRECTION ( 'NONE',  ( 0.000000000000000000, 0.000000000000000000, 1.000000000000000000 ) ) ;
#17946 = CARTESIAN_POINT ( 'NONE',  ( 104.9999999999999574, 82.68750000273121259, -2.071067811865491937 ) ) ;
#17947 = CARTESIAN_POINT ( 'NONE',  ( 96.46446609406726225, 93.37500000000000000, -3.535533905932738197 ) ) ;
#17948 = CARTESIAN_POINT ( 'NONE',  ( 99.99999999999998579, 95.31249999863440792, 4.458734124999981674 ) ) ;
#17949 = AXIS2_PLACEMENT_3D ( 'NONE', #24257, #9147, #8581 ) ;
#17950 = CARTESIAN_POINT ( 'NONE',  ( 97.83688103937537051, 103.3426043859339103, -48.60000000000000853 ) ) ;
#17951 = CARTESIAN_POINT ( 'NONE',  ( 55.70494972787295751, 32.91367187608393152, 9.295050272127047819 ) ) ;
#17952 = ORIENTED_EDGE ( 'NONE', *, *, #20584, .T. ) ;
#17953 = CARTESIAN_POINT ( 'NONE',  ( 96.46446609406726225, 95.49999999726881583, 3.535533905932723986 ) ) ;
#17954 = CARTESIAN_POINT ( 'NONE',  ( 94.99999999999995737, 1.387778780781445676E-14, 15.00000000000000000 ) ) ;
#17955 = ORIENTED_EDGE ( 'NONE', *, *, #5487, .T. ) ;
#17956 = CARTESIAN_POINT ( 'NONE',  ( -5.444914386472297529, 35.04687500108393294, -13.14518615778179900 ) ) ;
#17957 = CARTESIAN_POINT ( 'NONE',  ( 185.4011555911795597, 34.05468750216788010, 9.598844408820459861 ) ) ;
#17958 =( BOUNDED_CURVE ( )  B_SPLINE_CURVE ( 2, ( #20346, #18053, #20063, #13623, #26769, #5098, #16342, #25041, #2950 ),
 .UNSPECIFIED., .F., .T. ) 
 B_SPLINE_CURVE_WITH_KNOTS ( ( 3, 2, 2, 2, 3 ),
 ( 0.3125000000000002220, 0.3229166666666668517, 0.3333333333333334259, 0.3437500000000000555, 0.3541666666666666852 ),
 .UNSPECIFIED. ) 
 CURVE ( )  GEOMETRIC_REPRESENTATION_ITEM ( )  RATIONAL_B_SPLINE_CURVE ( ( 0.9999999999999983347, 0.9238795325112884038, 1.000000000000000000, 0.9238795325112867385, 1.000000000000000000, 0.9238795325112867385, 1.000000000000000000, 0.9238795325112867385, 1.000000000000000000 ) ) 
 REPRESENTATION_ITEM ( '' )  );
#17959 = ORIENTED_EDGE ( 'NONE', *, *, #8973, .T. ) ;
#17960 = CARTESIAN_POINT ( 'NONE',  ( -9.295050272127046043, 31.72304687608393081, -9.295050272127046043 ) ) ;
#17961 = CARTESIAN_POINT ( 'NONE',  ( 74.18017581364799184, 55.00000000000000000, -9.999999999999998224 ) ) ;
#17962 = CARTESIAN_POINT ( 'NONE',  ( 120.7049497278729575, 37.47773437608393010, -9.295050272127046043 ) ) ;
#17963 = CARTESIAN_POINT ( 'NONE',  ( -8.049105076161786076E-16, 35.79101562608394005, -13.14518615778179544 ) ) ;
#17964 = EDGE_CURVE ( 'NONE', #10805, #9259, #27191, .T. ) ;
#17965 = CARTESIAN_POINT ( 'NONE',  ( 100.0000000000000000, 110.0000000000000000, -55.00000000000000711 ) ) ;
#17966 = CARTESIAN_POINT ( 'NONE',  ( 51.42518405393695957, 32.21914062500000142, -5.622872871577873077 ) ) ;
#17967 = CARTESIAN_POINT ( 'NONE',  ( 99.99999999999998579, 92.25000000000000000, -4.999999999999997335 ) ) ;
#17968 = CARTESIAN_POINT ( 'NONE',  ( 123.6617092076501905, 35.99999999999997868, 11.53992004315006703 ) ) ;
#17969 = CARTESIAN_POINT ( 'NONE',  ( 98.15313185440925281, 4.458734125000016313, 12.50000000136559208 ) ) ;
#17970 = FACE_OUTER_BOUND ( 'NONE', #19733, .T. ) ;
#17971 = AXIS2_PLACEMENT_3D ( 'NONE', #15769, #9500, #22344 ) ;
#17972 = CARTESIAN_POINT ( 'NONE',  ( 101.8468681455906903, -4.458734124999987891, 0.7500000013655925279 ) ) ;
#17973 = CARTESIAN_POINT ( 'NONE',  ( 108.0825317500000153, 110.0000000000000000, -46.12500000273119838 ) ) ;
#17974 = CARTESIAN_POINT ( 'NONE',  ( 103.1528011352953484, 91.68749999863440792, -3.152801135295366208 ) ) ;
#17975 = CARTESIAN_POINT ( 'NONE',  ( 96.46446609406721961, 3.535533905932755072, 3.875000000000000000 ) ) ;
#17976 = CARTESIAN_POINT ( 'NONE',  ( 93.46109445667489979, 114.7507929638356785, -51.82499999726881867 ) ) ;
#17977 = CARTESIAN_POINT ( 'NONE',  ( 9.295050272127046043, 36.48554687608393721, -9.295050272127046043 ) ) ;
#17978 = ORIENTED_EDGE ( 'NONE', *, *, #2542, .T. ) ;
#17979 = DIRECTION ( 'NONE',  ( -0.000000000000000000, -1.000000000000000000, -0.000000000000000000 ) ) ;
#17980 = CARTESIAN_POINT ( 'NONE',  ( 95.00000000000000000, 91.43750000000000000, -2.071067811865479058 ) ) ;
#17981 = CARTESIAN_POINT ( 'NONE',  ( 200.4449143864723055, 34.45156250108393436, 13.14518615778179189 ) ) ;
#17982 = ORIENTED_EDGE ( 'NONE', *, *, #7051, .T. ) ;
#17983 = CARTESIAN_POINT ( 'NONE',  ( 99.99999999999995737, 85.00000000000000000, -1.387778780781445676E-14 ) ) ;
#17984 = CARTESIAN_POINT ( 'NONE',  ( 95.54126587499995082, 1.846868145590750077, 12.62500000136559208 ) ) ;
#17985 = EDGE_LOOP ( 'NONE', ( #8825, #12697, #6833, #25215 ) ) ;
#17986 = CARTESIAN_POINT ( 'NONE',  ( 91.91746824999998466, 112.6261737610028320, -53.47500000273119980 ) ) ;
#17987 = CIRCLE ( 'NONE', #27129, 5.000000000000000000 ) ;
#17988 = CARTESIAN_POINT ( 'NONE',  ( 9.295050272127046043, 37.08085937608393579, -9.295050272127046043 ) ) ;
#17989 = DIRECTION ( 'NONE',  ( -1.000000000000000000, 0.000000000000000000, 0.000000000000000000 ) ) ;
#17990 = CARTESIAN_POINT ( 'NONE',  ( 135.4449143864723055, 36.83281250108392868, 13.14518615778179189 ) ) ;
#17991 = CARTESIAN_POINT ( 'NONE',  ( -8.049105076161786076E-16, 40.55351562608393579, -13.14518615778179544 ) ) ;
#17992 = CARTESIAN_POINT ( 'NONE',  ( 13.14518615778179900, 35.44375000108393436, -5.444914386472297529 ) ) ;
#17993 = CARTESIAN_POINT ( 'NONE',  ( 97.92893218813452449, 95.18749999726880162, -4.999999999999997335 ) ) ;
#17994 = VECTOR ( 'NONE', #23519, 1000.000000000000000 ) ;
#17995 = CARTESIAN_POINT ( 'NONE',  ( 65.00000000000000000, 36.98164062608393721, 13.14518615778179544 ) ) ;
#17996 = CARTESIAN_POINT ( 'NONE',  ( 67.16995658311145689, 49.99999999883969082, -13.43548448457778477 ) ) ;
#17997 = VERTEX_POINT ( 'NONE', #13312 ) ;
#17998 = CARTESIAN_POINT ( 'NONE',  ( 104.9952793366501709, 103.1245878333314465, -52.67500000273119554 ) ) ;
#17999 = CARTESIAN_POINT ( 'NONE',  ( 195.0000000000000000, 32.61601562608393579, -13.14518615778179544 ) ) ;
#18000 = EDGE_CURVE ( 'NONE', #6173, #7474, #95, .T. ) ;
#18001 = VERTEX_POINT ( 'NONE', #26461 ) ;
#18002 = CARTESIAN_POINT ( 'NONE',  ( 9.295050272127046043, 36.48554687608393721, -9.295050272127046043 ) ) ;
#18003 = CARTESIAN_POINT ( 'NONE',  ( 96.84719886470459471, 3.152801135295383084, 6.562500001365592084 ) ) ;
#18004 = CARTESIAN_POINT ( 'NONE',  ( 51.85481384221820633, 37.32890625108393579, -5.444914386472297529 ) ) ;
#18005 = DIRECTION ( 'NONE',  ( -1.000000000000000000, 0.000000000000000000, 0.000000000000000000 ) ) ;
#18006 = CARTESIAN_POINT ( 'NONE',  ( 200.4449143864723055, 36.33671875108393579, -13.14518615778179722 ) ) ;
#18007 = CARTESIAN_POINT ( 'NONE',  ( -13.14518615778179189, 33.65781250108393152, 5.444914386472304635 ) ) ;
#18008 =( BOUNDED_CURVE ( )  B_SPLINE_CURVE ( 2, ( #10215, #7679, #16515, #5695, #23078, #12210, #20937, #1421, #16788 ),
 .UNSPECIFIED., .F., .F. ) 
 B_SPLINE_CURVE_WITH_KNOTS ( ( 3, 2, 2, 2, 3 ),
 ( 0.2708333333333330928, 0.2812499999999998890, 0.2916666666666666852, 0.3020833333333334259, 0.3125000000000002220 ),
 .UNSPECIFIED. ) 
 CURVE ( )  GEOMETRIC_REPRESENTATION_ITEM ( )  RATIONAL_B_SPLINE_CURVE ( ( 1.000000000000001554, 0.9238795325112850731, 1.000000000000000000, 0.9238795325112867385, 1.000000000000000000, 0.9238795325112867385, 1.000000000000000000, 0.9238795325112850731, 1.000000000000001554 ) ) 
 REPRESENTATION_ITEM ( '' )  );
#18009 = CARTESIAN_POINT ( 'NONE',  ( 99.99999999999998579, 124.7999999999999972, -2.499999999999997780 ) ) ;
#18010 = CARTESIAN_POINT ( 'NONE',  ( 181.8548138422182205, 37.62656250108393152, 5.444914386472304635 ) ) ;
#18011 = CARTESIAN_POINT ( 'NONE',  ( 95.00472066334982912, 116.8754121666685393, -48.17499999726882010 ) ) ;
#18012 = ORIENTED_EDGE ( 'NONE', *, *, #2573, .T. ) ;
#18013 = CARTESIAN_POINT ( 'NONE',  ( -8.312177448680279460E-16, 34.45156249999999432, -13.57481594606304576 ) ) ;
#18014 = CARTESIAN_POINT ( 'NONE',  ( 13.14518615778179900, 33.06250000108393294, -5.444914386472297529 ) ) ;
#18015 = ORIENTED_EDGE ( 'NONE', *, *, #9550, .F. ) ;
#18016 = CARTESIAN_POINT ( 'NONE',  ( 124.5550856135277087, 34.25312500108393010, -13.14518615778179900 ) ) ;
#18017 = CARTESIAN_POINT ( 'NONE',  ( 1.662435489736055892E-15, 30.99999999999999645, 13.57481594606304576 ) ) ;
#18018 = CARTESIAN_POINT ( 'NONE',  ( 181.8548138422181921, 32.86406250108393579, 5.444914386472304635 ) ) ;
#18019 = EDGE_LOOP ( 'NONE', ( #12086, #21410 ) ) ;
#18020 = CARTESIAN_POINT ( 'NONE',  ( 102.0710678118654329, 5.000000000000018652, 10.81250000273118417 ) ) ;
#18021 = CARTESIAN_POINT ( 'NONE',  ( -0.9830651850993568086, 49.99999999948985874, -13.54930971656723493 ) ) ;
#18022 = CARTESIAN_POINT ( 'NONE',  ( 97.50236033167492167, 117.6869444889999841, -47.52500000273119696 ) ) ;
#18023 = DIRECTION ( 'NONE',  ( 0.000000000000000000, 1.000000000000000000, 0.000000000000000000 ) ) ;
#18024 = ADVANCED_FACE ( 'NONE', ( #17330 ), #26167, .T. ) ;
#18025 = CARTESIAN_POINT ( 'NONE',  ( -5.622872871577964560, 33.80664062716787299, -13.57481594606295339 ) ) ;
#18026 = CARTESIAN_POINT ( 'NONE',  ( 73.76938967208273823, 50.37710889401973446, 15.00000000000719602 ) ) ;
#18027 = ORIENTED_EDGE ( 'NONE', *, *, #13351, .F. ) ;
#18028 = CARTESIAN_POINT ( 'NONE',  ( 103.1528011352953342, 3.152801135295383084, 6.062500001365592084 ) ) ;
#18029 = AXIS2_PLACEMENT_3D ( 'NONE', #21467, #26153, #25730 ) ;
#18030 = ORIENTED_EDGE ( 'NONE', *, *, #6530, .T. ) ;
#18031 = CARTESIAN_POINT ( 'NONE',  ( -8.312177448680279460E-16, 35.34453125216787583, -13.57481594606304576 ) ) ;
#18032 = CARTESIAN_POINT ( 'NONE',  ( 99.99999999999995737, -4.458734124999988779, 9.687500001365593860 ) ) ;
#18033 = CARTESIAN_POINT ( 'NONE',  ( 135.6228728715779255, 38.46992187716787726, -13.57481594606299247 ) ) ;
#18034 = EDGE_CURVE ( 'NONE', #7953, #2000, #10902, .T. ) ;
#18035 = CARTESIAN_POINT ( 'NONE',  ( 13.14518615778179544, 34.60039062608392868, -1.609821015232357215E-15 ) ) ;
#18036 = FACE_OUTER_BOUND ( 'NONE', #19797, .T. ) ;
#18037 = CARTESIAN_POINT ( 'NONE',  ( 70.62287287157776916, 37.67617187716787441, -13.57481594606313990 ) ) ;
#18038 = CARTESIAN_POINT ( 'NONE',  ( 99.99999999999998579, 93.06249999863440792, 4.458734124999981674 ) ) ;
#18039 = CARTESIAN_POINT ( 'NONE',  ( -13.14518615778179544, 37.37851562608393863, 0.000000000000000000 ) ) ;
#18040 =( BOUNDED_SURFACE ( )  B_SPLINE_SURFACE ( 1, 2, ( 
 ( #9821, #23085, #10086, #11808, #20672, #14092, #16379, #20531, #25357, #2988, #1156, #12218, #5567, #1013, #22952, #25214, #3279, #14230, #7828, #25079, #11948, #3559, #9955, #16239, #18798, #18528, #27505, #3414, #5276, #27233, #16521, #16088, #7688, #12082, #24936, #24794, #7394, #20945, #13942, #20806, #16660, #5838, #1286, #22523, #27369, #7961, #11662, #871, #5423, #18667, #5702, #20384, #9682, #14369, #9542, #22811, #18243, #26951, #22668, #18385, #27640, #15054, #4112, #1569, #21362, #21494, #17205, #21640, #25910, #6108, #6382, #10780, #19351, #28053, #14775, #23771, #8520, #23358, #12778, #10222, #14915, #26046, #3831, #4247, #19071, #12907, #2113, #18932, #25626, #17350, #14507, #19212, #23636, #12493, #19492, #12635, #8101, #28191, #27777, #23495, #1975, #21219, #3700, #8236, #16795, #1843, #10645, #3975, #1703, #23224, #16927, #10506, #10361, #8659, #12362, #21080, #25493, #27915, #5973, #8376, #14640, #17061, #25764, #6246, #13624, #15338, #4675, #26336, #401, #24053, #9361, #15192, #13337, #24478, #17779, #4529, #6937, #9224, #15482, #26482, #20064, #9083, #24196, #7075, #22202, #19771, #22345, #2541, #2816, #15632, #17487, #22064, #543, #114, #11201, #19917, #254, #8796, #19632, #4962, #26186, #24333, #686, #6652, #23910, #4819, #11484, #13479, #20200, #8938, #17916, #4390, #6795, #26627, #18054, #11341, #15770, #2679, #6516, #13047, #13190, #21782, #2262 ),
 ( #10923, #21926, #2402, #11060, #17628, #11768, #16197, #22486, #25175, #5099, #5525, #24903, #976, #26770, #22911, #5383, #27333, #11624, #1253, #18202, #9501, #18492, #14053, #18347, #22633, #16050, #3522, #27199, #833, #12181, #5664, #13905, #1115, #7793, #14328, #24760, #9643, #20347, #16479, #26912, #9914, #22774, #3240, #20768, #7651, #18630, #15904, #7213, #23047, #20909, #27052, #20632, #1391, #7503, #10053, #11908, #24622, #13763, #2951, #7357, #9783, #5240, #3102, #16343, #25042, #14191, #20492, #3373, #12043, #3663, #23739, #12597, #15018, #12871, #3937, #6074, #19176, #21323, #25590, #6211, #21601, #25728, #16756, #2079, #10468, #18764, #23595, #28018, #27467, #25313, #3796, #1803, #23460, #6343, #8061, #21464, #12740, #23323, #10323, #7924, #16892, #27879, #12325, #19317, #8340, #5803, #14741, #14880, #8201, #8484, #21045, #1941, #10181, #1529, #17025, #4078, #19029, #14605, #25456, #4214, #10610, #18891, #16622, #25875, #5937, #17173, #14469, #23187, #12456, #21181, #27601, #1663, #27741, #22167, #17594, #6763, #4780, #11163, #2645, #28156, #19458, #11307, #508, #21894, #4638, #9189, #11022, #20029, #2366, #15735, #24439, #17884, #8622, #13296, #78, #15303, #13155, #19735, #26301, #21748, #10747, #4497, #23875, #4926, #22024, #7036, #13589, #24161, #15446, #19879, #2502, #364, #26444, #22311, #17743, #8763, #17311, #9051, #26011, #15592, #26589, #6482, #15156 ) ),
 .UNSPECIFIED., .F., .F., .T. ) 
 B_SPLINE_SURFACE_WITH_KNOTS ( ( 2, 2 ),
 ( 3, 2, 2, 2, 2, 2, 2, 2, 2, 2, 2, 2, 2, 2, 2, 2, 2, 2, 2, 2, 2, 2, 2, 2, 2, 2, 2, 2, 2, 2, 2, 2, 2, 2, 2, 2, 2, 2, 2, 2, 2, 2, 2, 2, 2, 2, 2, 2, 2, 2, 2, 2, 2, 2, 2, 2, 2, 2, 2, 2, 2, 2, 2, 2, 2, 2, 2, 2, 2, 2, 2, 2, 2, 2, 2, 2, 2, 2, 2, 2, 2, 2, 2, 2, 2, 2, 2, 2, 2, 2, 2, 3 ),
 ( 0.000000000000000000, 1.000000000000000000 ),
 ( 0.000000000000000000, 0.01041666666666666609, 0.02083333333333333218, 0.03125000000000000000, 0.04166666666666666435, 0.05208333333333333565, 0.06250000000000000000, 0.07291666666666667129, 0.08333333333333332871, 0.09375000000000000000, 0.1041666666666666713, 0.1145833333333333287, 0.1250000000000000000, 0.1354166666666666574, 0.1458333333333333426, 0.1562500000000000000, 0.1666666666666666574, 0.1770833333333333426, 0.1875000000000000000, 0.1979166666666666574, 0.2083333333333333426, 0.2187500000000000000, 0.2291666666666666574, 0.2395833333333333426, 0.2500000000000000000, 0.2604166666666666852, 0.2708333333333333148, 0.2812500000000000000, 0.2916666666666666852, 0.3020833333333333148, 0.3125000000000000000, 0.3229166666666666852, 0.3333333333333333148, 0.3437500000000000000, 0.3541666666666666852, 0.3645833333333333148, 0.3750000000000000000, 0.3854166666666666852, 0.3958333333333333148, 0.4062500000000000000, 0.4166666666666666852, 0.4270833333333333148, 0.4375000000000000000, 0.4479166666666666852, 0.4583333333333333148, 0.4687500000000000000, 0.4791666666666666852, 0.4895833333333333148, 0.5000000000000000000, 0.5104166666666666297, 0.5208333333333333703, 0.5312500000000000000, 0.5416666666666666297, 0.5520833333333333703, 0.5625000000000000000, 0.5729166666666666297, 0.5833333333333333703, 0.5937500000000000000, 0.6041666666666666297, 0.6145833333333333703, 0.6250000000000000000, 0.6354166666666666297, 0.6458333333333333703, 0.6562500000000000000, 0.6666666666666666297, 0.6770833333333333703, 0.6875000000000000000, 0.6979166666666666297, 0.7083333333333333703, 0.7187500000000000000, 0.7291666666666666297, 0.7395833333333333703, 0.7500000000000000000, 0.7604166666666666297, 0.7708333333333333703, 0.7812500000000000000, 0.7916666666666666297, 0.8020833333333333703, 0.8125000000000000000, 0.8229166666666666297, 0.8333333333333333703, 0.8437500000000000000, 0.8541666666666666297, 0.8645833333333333703, 0.8750000000000000000, 0.8854166666666666297, 0.8958333333333333703, 0.9062500000000000000, 0.9166666666666666297, 0.9270833333333333703, 0.9375000000000000000, 0.9448586970929392370 ),
 .UNSPECIFIED. ) 
 GEOMETRIC_REPRESENTATION_ITEM ( )  RATIONAL_B_SPLINE_SURFACE ( (
 ( 1.000000000000000000, 0.9238795325112867385, 1.000000000000000000, 0.9238795325112867385, 1.000000000000000000, 0.9238795325112867385, 1.000000000000000000, 0.9238795325112867385, 1.000000000000000000, 0.9238795325112867385, 1.000000000000000000, 0.9238795325112867385, 1.000000000000000000, 0.9238795325112867385, 1.000000000000000000, 0.9238795325112867385, 1.000000000000000000, 0.9238795325112867385, 1.000000000000000000, 0.9238795325112867385, 1.000000000000000000, 0.9238795325112867385, 1.000000000000000000, 0.9238795325112867385, 1.000000000000000000, 0.9238795325112867385, 1.000000000000000000, 0.9238795325112867385, 1.000000000000000000, 0.9238795325112867385, 1.000000000000000000, 0.9238795325112867385, 1.000000000000000000, 0.9238795325112867385, 1.000000000000000000, 0.9238795325112867385, 1.000000000000000000, 0.9238795325112867385, 1.000000000000000000, 0.9238795325112867385, 1.000000000000000000, 0.9238795325112867385, 1.000000000000000000, 0.9238795325112867385, 1.000000000000000000, 0.9238795325112867385, 1.000000000000000000, 0.9238795325112867385, 1.000000000000000000, 0.9238795325112867385, 1.000000000000000000, 0.9238795325112867385, 1.000000000000000000, 0.9238795325112867385, 1.000000000000000000, 0.9238795325112867385, 1.000000000000000000, 0.9238795325112867385, 1.000000000000000000, 0.9238795325112867385, 1.000000000000000000, 0.9238795325112867385, 1.000000000000000000, 0.9238795325112867385, 1.000000000000000000, 0.9238795325112867385, 1.000000000000000000, 0.9238795325112867385, 1.000000000000000000, 0.9238795325112867385, 1.000000000000000000, 0.9238795325112867385, 1.000000000000000000, 0.9238795325112867385, 1.000000000000000000, 0.9238795325112867385, 1.000000000000000000, 0.9238795325112867385, 1.000000000000000000, 0.9238795325112867385, 1.000000000000000000, 0.9238795325112867385, 1.000000000000000000, 0.9238795325112867385, 1.000000000000000000, 0.9238795325112867385, 1.000000000000000000, 0.9238795325112867385, 1.000000000000000000, 0.9238795325112867385, 1.000000000000000000, 0.9238795325112867385, 1.000000000000000000, 0.9238795325112867385, 1.000000000000000000, 0.9238795325112867385, 1.000000000000000000, 0.9238795325112867385, 1.000000000000000000, 0.9238795325112867385, 1.000000000000000000, 0.9238795325112867385, 1.000000000000000000, 0.9238795325112867385, 1.000000000000000000, 0.9238795325112867385, 1.000000000000000000, 0.9238795325112867385, 1.000000000000000000, 0.9238795325112867385, 1.000000000000000000, 0.9238795325112867385, 1.000000000000000000, 0.9238795325112867385, 1.000000000000000000, 0.9238795325112867385, 1.000000000000000000, 0.9238795325112867385, 1.000000000000000000, 0.9238795325112867385, 1.000000000000000000, 0.9238795325112867385, 1.000000000000000000, 0.9238795325112867385, 1.000000000000000000, 0.9238795325112867385, 1.000000000000000000, 0.9238795325112867385, 1.000000000000000000, 0.9238795325112867385, 1.000000000000000000, 0.9238795325112867385, 1.000000000000000000, 0.9238795325112867385, 1.000000000000000000, 0.9238795325112867385, 1.000000000000000000, 0.9238795325112867385, 1.000000000000000000, 0.9238795325112867385, 1.000000000000000000, 0.9238795325112867385, 1.000000000000000000, 0.9238795325112867385, 1.000000000000000000, 0.9238795325112867385, 1.000000000000000000, 0.9238795325112867385, 1.000000000000000000, 0.9238795325112867385, 1.000000000000000000, 0.9238795325112867385, 1.000000000000000000, 0.9238795325112867385, 1.000000000000000000, 0.9238795325112867385, 1.000000000000000000, 0.9238795325112867385, 1.000000000000000000, 0.9238795325112867385, 1.000000000000000000, 0.9238795325112867385, 1.000000000000000000, 0.9238795325112867385, 1.000000000000000000, 0.9238795325112867385, 1.000000000000000000, 0.9238795325112867385, 1.000000000000000000, 0.9238795325112867385, 1.000000000000000000, 0.9238795325112867385, 1.000000000000000000, 0.9238795325112867385, 1.000000000000000000, 0.9238795325112867385, 1.000000000000000000, 0.9238795325112867385, 1.000000000000000000, 0.9238795325112867385, 1.000000000000000000, 0.9462258435690522607, 0.9684275710300105366),
 ( 1.000000000000000000, 0.9238795325112867385, 1.000000000000000000, 0.9238795325112867385, 1.000000000000000000, 0.9238795325112867385, 1.000000000000000000, 0.9238795325112867385, 1.000000000000000000, 0.9238795325112867385, 1.000000000000000000, 0.9238795325112867385, 1.000000000000000000, 0.9238795325112867385, 1.000000000000000000, 0.9238795325112867385, 1.000000000000000000, 0.9238795325112867385, 1.000000000000000000, 0.9238795325112867385, 1.000000000000000000, 0.9238795325112867385, 1.000000000000000000, 0.9238795325112867385, 1.000000000000000000, 0.9238795325112867385, 1.000000000000000000, 0.9238795325112867385, 1.000000000000000000, 0.9238795325112867385, 1.000000000000000000, 0.9238795325112867385, 1.000000000000000000, 0.9238795325112867385, 1.000000000000000000, 0.9238795325112867385, 1.000000000000000000, 0.9238795325112867385, 1.000000000000000000, 0.9238795325112867385, 1.000000000000000000, 0.9238795325112867385, 1.000000000000000000, 0.9238795325112867385, 1.000000000000000000, 0.9238795325112867385, 1.000000000000000000, 0.9238795325112867385, 1.000000000000000000, 0.9238795325112867385, 1.000000000000000000, 0.9238795325112867385, 1.000000000000000000, 0.9238795325112867385, 1.000000000000000000, 0.9238795325112867385, 1.000000000000000000, 0.9238795325112867385, 1.000000000000000000, 0.9238795325112867385, 1.000000000000000000, 0.9238795325112867385, 1.000000000000000000, 0.9238795325112867385, 1.000000000000000000, 0.9238795325112867385, 1.000000000000000000, 0.9238795325112867385, 1.000000000000000000, 0.9238795325112867385, 1.000000000000000000, 0.9238795325112867385, 1.000000000000000000, 0.9238795325112867385, 1.000000000000000000, 0.9238795325112867385, 1.000000000000000000, 0.9238795325112867385, 1.000000000000000000, 0.9238795325112867385, 1.000000000000000000, 0.9238795325112867385, 1.000000000000000000, 0.9238795325112867385, 1.000000000000000000, 0.9238795325112867385, 1.000000000000000000, 0.9238795325112867385, 1.000000000000000000, 0.9238795325112867385, 1.000000000000000000, 0.9238795325112867385, 1.000000000000000000, 0.9238795325112867385, 1.000000000000000000, 0.9238795325112867385, 1.000000000000000000, 0.9238795325112867385, 1.000000000000000000, 0.9238795325112867385, 1.000000000000000000, 0.9238795325112867385, 1.000000000000000000, 0.9238795325112867385, 1.000000000000000000, 0.9238795325112867385, 1.000000000000000000, 0.9238795325112867385, 1.000000000000000000, 0.9238795325112867385, 1.000000000000000000, 0.9238795325112867385, 1.000000000000000000, 0.9238795325112867385, 1.000000000000000000, 0.9238795325112867385, 1.000000000000000000, 0.9238795325112867385, 1.000000000000000000, 0.9238795325112867385, 1.000000000000000000, 0.9238795325112867385, 1.000000000000000000, 0.9238795325112867385, 1.000000000000000000, 0.9238795325112867385, 1.000000000000000000, 0.9238795325112867385, 1.000000000000000000, 0.9238795325112867385, 1.000000000000000000, 0.9238795325112867385, 1.000000000000000000, 0.9238795325112867385, 1.000000000000000000, 0.9238795325112867385, 1.000000000000000000, 0.9238795325112867385, 1.000000000000000000, 0.9238795325112867385, 1.000000000000000000, 0.9238795325112867385, 1.000000000000000000, 0.9238795325112867385, 1.000000000000000000, 0.9238795325112867385, 1.000000000000000000, 0.9238795325112867385, 1.000000000000000000, 0.9238795325112867385, 1.000000000000000000, 0.9238795325112867385, 1.000000000000000000, 0.9238795325112867385, 1.000000000000000000, 0.9238795325112867385, 1.000000000000000000, 0.9238795325112867385, 1.000000000000000000, 0.9238795325112867385, 1.000000000000000000, 0.9238795325112867385, 1.000000000000000000, 0.9238795325112867385, 1.000000000000000000, 0.9238795325112867385, 1.000000000000000000, 0.9238795325112867385, 1.000000000000000000, 0.9238795325112867385, 1.000000000000000000, 0.9238795325112867385, 1.000000000000000000, 0.9238795325112867385, 1.000000000000000000, 0.9238795325112867385, 1.000000000000000000, 0.9238795325112867385, 1.000000000000000000, 0.9238795325112867385, 1.000000000000000000, 0.9462258435690522607, 0.9684275710300105366) ) ) 
 REPRESENTATION_ITEM ( '' )  SURFACE ( )  );
#18041 = CARTESIAN_POINT ( 'NONE',  ( -6.161062174842506955, 51.27996893917265453, 14.99999999999930900 ) ) ;
#18042 = CARTESIAN_POINT ( 'NONE',  ( 112.9999999999999858, 123.0000000000000000, 12.99999999999998934 ) ) ;
#18043 = CARTESIAN_POINT ( 'NONE',  ( 139.5988444088204403, 35.14609374999999858, -9.598844408820458085 ) ) ;
#18044 = ADVANCED_FACE ( 'NONE', ( #6634 ), #17336, .T. ) ;
#18045 = EDGE_LOOP ( 'NONE', ( #15046, #1632, #27284, #22953 ) ) ;
#18046 = CARTESIAN_POINT ( 'NONE',  ( -13.57481594606304753, 40.25585937716787299, -5.622872871577872189 ) ) ;
#18047 =( BOUNDED_CURVE ( )  B_SPLINE_CURVE ( 2, ( #23886, #28028, #6491, #12750, #17179, #23471, #6628, #6084, #4363 ),
 .UNSPECIFIED., .F., .F. ) 
 B_SPLINE_CURVE_WITH_KNOTS ( ( 3, 2, 2, 2, 3 ),
 ( 0.3958333333333331483, 0.4062499999999999445, 0.4166666666666667407, 0.4270833333333335369, 0.4375000000000003331 ),
 .UNSPECIFIED. ) 
 CURVE ( )  GEOMETRIC_REPRESENTATION_ITEM ( )  RATIONAL_B_SPLINE_CURVE ( ( 1.000000000000001110, 0.9238795325112855172, 1.000000000000000000, 0.9238795325112867385, 1.000000000000000000, 0.9238795325112867385, 1.000000000000000000, 0.9238795325112842960, 1.000000000000002442 ) ) 
 REPRESENTATION_ITEM ( '' )  );
#18048 = CARTESIAN_POINT ( 'NONE',  ( -5.444914386472299306, 33.75703125108393721, 13.14518615778179722 ) ) ;
#18049 = CARTESIAN_POINT ( 'NONE',  ( 13.57481594606304931, 33.50898437716787015, 5.622872871577869525 ) ) ;
#18050 = CARTESIAN_POINT ( 'NONE',  ( 102.0710678118654329, -4.999999999999989342, 10.43750000273118417 ) ) ;
#18051 = CARTESIAN_POINT ( 'NONE',  ( 120.7049497278729575, 33.31054687608393294, -9.295050272127046043 ) ) ;
#18052 = CARTESIAN_POINT ( 'NONE',  ( 78.14518615778179367, 38.61875000108393152, -5.444914386472297529 ) ) ;
#18053 = CARTESIAN_POINT ( 'NONE',  ( 59.37712712842203189, 37.27929687716785878, 13.57481594606295161 ) ) ;
#18054 = CARTESIAN_POINT ( 'NONE',  ( -9.598844408820454532, 31.67343750216787512, 9.598844408820459861 ) ) ;
#18055 = CARTESIAN_POINT ( 'NONE',  ( 102.4999999999999858, 123.9500000021849502, -1.035533905932742638 ) ) ;
#18056 = AXIS2_PLACEMENT_3D ( 'NONE', #20152, #26714, #22858 ) ;
#18057 = CARTESIAN_POINT ( 'NONE',  ( 99.99999999999997158, 118.4984768113314146, -50.37499999726882294 ) ) ;
#18058 = CARTESIAN_POINT ( 'NONE',  ( 5.622872871577871301, 39.26367187716787299, -13.57481594606304753 ) ) ;
#18059 = CARTESIAN_POINT ( 'NONE',  ( 181.8548138422181921, 33.36015625108393579, -5.444914386472297529 ) ) ;
#18060 = DIRECTION ( 'NONE',  ( 1.000000000000000000, 0.000000000000000000, -5.551115123125784280E-15 ) ) ;
#18061 = DIRECTION ( 'NONE',  ( 0.000000000000000000, 0.000000000000000000, -1.000000000000000000 ) ) ;
#18062 = CARTESIAN_POINT ( 'NONE',  ( 97.93301270000000613, 123.7500000010924879, -9.540979117872439019E-15 ) ) ;
#18063 = CARTESIAN_POINT ( 'NONE',  ( 94.99999999999995737, 1.387778780781445676E-14, 12.12500000273118594 ) ) ;
#18064 = CARTESIAN_POINT ( 'NONE',  ( 104.9999999999999716, 1.449011120738813565E-14, 1.625000002731184834 ) ) ;
#18065 = DIRECTION ( 'NONE',  ( 0.000000000000000000, -0.000000000000000000, 1.000000000000000000 ) ) ;
#18066 = CARTESIAN_POINT ( 'NONE',  ( 5.622872871577871301, 35.19570312499999432, -13.57481594606304753 ) ) ;
#18067 = CARTESIAN_POINT ( 'NONE',  ( 97.83688103937538472, 116.6573956140660897, -54.40000000000000568 ) ) ;
#18068 = AXIS2_PLACEMENT_3D ( 'NONE', #16742, #16878, #27447 ) ;
#18069 = CARTESIAN_POINT ( 'NONE',  ( 5.444914386472302859, 35.44375000108393436, 13.14518615778179189 ) ) ;
#18070 = CARTESIAN_POINT ( 'NONE',  ( 2.414731522848535132E-15, 36.78320312608393294, 13.14518615778179544 ) ) ;
#18071 = CARTESIAN_POINT ( 'NONE',  ( -5.444914386472297529, 35.64218750108393152, -13.14518615778179722 ) ) ;
#18072 = EDGE_CURVE ( 'NONE', #6018, #13666, #1872, .T. ) ;
#18073 = CARTESIAN_POINT ( 'NONE',  ( -5.622872871577873077, 36.98164062716787015, -13.57481594606304753 ) ) ;
#18074 = CARTESIAN_POINT ( 'NONE',  ( 5.622872871577780707, 37.67617187716787441, -13.57481594606313990 ) ) ;
#18075 = CARTESIAN_POINT ( 'NONE',  ( 98.15313185440925281, 83.25000000136560629, -4.458734125000016313 ) ) ;
#18076 = CARTESIAN_POINT ( 'NONE',  ( 51.85481384221820633, 32.66562500108393863, 5.444914386472304635 ) ) ;
#18077 = CARTESIAN_POINT ( 'NONE',  ( 108.0825317500000153, 110.0000000000000000, -52.37500000273119838 ) ) ;
#18078 = CARTESIAN_POINT ( 'NONE',  ( 98.35030804145870320, 123.0000000000000284, -1.884035693330653904 ) ) ;
#18079 = ORIENTED_EDGE ( 'NONE', *, *, #15572, .F. ) ;
#18080 = CARTESIAN_POINT ( 'NONE',  ( 97.93301270000000613, 123.7500000010924879, -9.540979117872439019E-15 ) ) ;
#18081 = CARTESIAN_POINT ( 'NONE',  ( -13.57481594606304753, 34.60039062499999574, -5.622872871577873077 ) ) ;
#18082 = CARTESIAN_POINT ( 'NONE',  ( 124.5550856135277087, 37.42812500108394147, -13.14518615778179900 ) ) ;
#18083 = ORIENTED_EDGE ( 'NONE', *, *, #25674, .F. ) ;
#18084 = CARTESIAN_POINT ( 'NONE',  ( -20.00000000000000000, 75.00000000000000000, 15.00000000000000178 ) ) ;
#18085 = CARTESIAN_POINT ( 'NONE',  ( 99.99999999999997158, 117.3602355696678643, -47.50000000000001421 ) ) ;
#18086 = CARTESIAN_POINT ( 'NONE',  ( 101.8468681455906903, 84.12500000136560629, -4.458734125000016313 ) ) ;
#18087 = CARTESIAN_POINT ( 'NONE',  ( 104.9999999999999858, 91.00000000000000000, -6.938893903907228378E-15 ) ) ;
#18088 = LINE ( 'NONE', #3276, #15607 ) ;
#18089 =( BOUNDED_CURVE ( )  B_SPLINE_CURVE ( 2, ( #19923, #23918, #9090, #13053, #2268, #23776, #6945, #2119, #4829 ),
 .UNSPECIFIED., .F., .F. ) 
 B_SPLINE_CURVE_WITH_KNOTS ( ( 3, 2, 2, 2, 3 ),
 ( 0.6500000000000005773, 0.6750000000000005995, 0.7000000000000006217, 0.7250000000000006439, 0.7500000000000006661 ),
 .UNSPECIFIED. ) 
 CURVE ( )  GEOMETRIC_REPRESENTATION_ITEM ( )  RATIONAL_B_SPLINE_CURVE ( ( 0.9999999999999983347, 0.9238795325112884038, 1.000000000000000000, 0.9238795325112867385, 1.000000000000000000, 0.9238795325112867385, 1.000000000000000000, 0.9238795325112847401, 1.000000000000001998 ) ) 
 REPRESENTATION_ITEM ( '' )  );
#18090 = CARTESIAN_POINT ( 'NONE',  ( 95.67376207875069838, 104.0454443415356991, -54.70000000000001705 ) ) ;
#18091 = CARTESIAN_POINT ( 'NONE',  ( 51.85481384221820633, 32.86406250108393579, 5.444914386472304635 ) ) ;
#18092 = ORIENTED_EDGE ( 'NONE', *, *, #10643, .F. ) ;
#18093 = CLOSED_SHELL ( 'NONE', ( #256, #3956, #11422, #17439, #27261, #4261, #12111, #2726, #23643, #1394, #4548, #16618, #23616, #2696, #12323, #2342, #4605, #19014, #6729, #8017, #12915, #17638, #5509, #16620 ) ) ;
#18094 = CIRCLE ( 'NONE', #9439, 5.000000000000000000 ) ;
#18095 = LINE ( 'NONE', #8834, #2233 ) ;
#18096 = CARTESIAN_POINT ( 'NONE',  ( 98.15313185440925281, -4.458734124999987891, 0.8750000013655926390 ) ) ;
#18097 = VERTEX_POINT ( 'NONE', #18181 ) ;
#18098 = CARTESIAN_POINT ( 'NONE',  ( 5.444914386472297529, 36.53515625108393294, -13.14518615778179900 ) ) ;
#18099 = CARTESIAN_POINT ( 'NONE',  ( 208.5748159460630120, 34.30273437716787299, 5.622872871577869525 ) ) ;
#18100 = ORIENTED_EDGE ( 'NONE', *, *, #20458, .F. ) ;
#18101 = CARTESIAN_POINT ( 'NONE',  ( -13.14518615778179722, 31.77265625108393365, -5.444914386472297529 ) ) ;
#18102 = PRODUCT_DEFINITION_SHAPE ( 'NONE', 'NONE',  #13233 ) ;
#18103 = CARTESIAN_POINT ( 'NONE',  ( 219.9999999999999716, 55.00000000000000000, 9.999999999999946709 ) ) ;
#18104 = CARTESIAN_POINT ( 'NONE',  ( 2.493653234604083739E-15, 32.56640625216787299, 13.57481594606304576 ) ) ;
#18105 = CARTESIAN_POINT ( 'NONE',  ( 13.14518615778179544, 34.79882812608394005, -1.609821015232357215E-15 ) ) ;
#18106 = FACE_BOUND ( 'NONE', #9989, .T. ) ;
#18107 = CARTESIAN_POINT ( 'NONE',  ( 104.4587341249999781, 92.31249999863440792, -6.938893903907228378E-15 ) ) ;
#18108 = CARTESIAN_POINT ( 'NONE',  ( 0.000000000000000000, 36.00000000000000000, 0.000000000000000000 ) ) ;
#18109 = DIRECTION ( 'NONE',  ( 0.000000000000000000, 0.000000000000000000, 1.000000000000000000 ) ) ;
#18110 = PLANE ( 'NONE',  #7732 ) ;
#18111 = CARTESIAN_POINT ( 'NONE',  ( 96.84719886470459471, -3.152801135295355994, 7.812500001365592084 ) ) ;
#18112 = CARTESIAN_POINT ( 'NONE',  ( 134.1572863549629062, 35.99999999999997158, -12.92256159328817411 ) ) ;
#18113 = CARTESIAN_POINT ( 'NONE',  ( 98.15313185440923860, 4.458734125000016313, 10.25000000136559031 ) ) ;
#18114 = CARTESIAN_POINT ( 'NONE',  ( 93.00000000000001421, 107.7255621263696668, -52.40000000546238823 ) ) ;
#18115 = CARTESIAN_POINT ( 'NONE',  ( 0.000000000000000000, -7.395377635281828788, 0.000000000000000000 ) ) ;
#18116 = DIRECTION ( 'NONE',  ( 0.000000000000000000, 0.000000000000000000, -1.000000000000000000 ) ) ;
#18117 = DIRECTION ( 'NONE',  ( 0.000000000000000000, 0.000000000000000000, 1.000000000000000000 ) ) ;
#18118 = CARTESIAN_POINT ( 'NONE',  ( 9.295050272127047819, 32.31835937608393294, 9.295050272127046043 ) ) ;
#18119 = ORIENTED_EDGE ( 'NONE', *, *, #26391, .F. ) ;
#18120 = CARTESIAN_POINT ( 'NONE',  ( 7.171390501253594785, 31.30502191632583830, -11.52591802191987114 ) ) ;
#18121 = CARTESIAN_POINT ( 'NONE',  ( 0.000000000000000000, 31.00000000000000000, 0.000000000000000000 ) ) ;
#18122 = CARTESIAN_POINT ( 'NONE',  ( -13.57481594606304753, 36.18789062499999432, -5.622872871577872189 ) ) ;
#18123 = ADVANCED_FACE ( 'NONE', ( #7338 ), #2796, .T. ) ;
#18124 = CARTESIAN_POINT ( 'NONE',  ( 189.5550856135277229, 34.84843750108393579, -13.14518615778179900 ) ) ;
#18125 =( BOUNDED_CURVE ( )  B_SPLINE_CURVE ( 2, ( #24902, #17915, #18201 ),
 .UNSPECIFIED., .F., .T. ) 
 B_SPLINE_CURVE_WITH_KNOTS ( ( 3, 3 ),
 ( 0.9375000000000000000, 0.9448586968893691873 ),
 .UNSPECIFIED. ) 
 CURVE ( )  GEOMETRIC_REPRESENTATION_ITEM ( )  RATIONAL_B_SPLINE_CURVE ( ( 1.000000000000000000, 0.9462258450566536361, 0.9684275698016389100 ) ) 
 REPRESENTATION_ITEM ( '' )  );
#18126 = EDGE_LOOP ( 'NONE', ( #3167, #8138, #823 ) ) ;
#18127 = CARTESIAN_POINT ( 'NONE',  ( 5.622872871577976994, 40.05742187716787583, -13.57481594606294095 ) ) ;
#18128 = CARTESIAN_POINT ( 'NONE',  ( 98.15313185440925281, 4.458734125000016313, 10.50000000136559208 ) ) ;
#18129 = ORIENTED_EDGE ( 'NONE', *, *, #27140, .F. ) ;
#18130 = CARTESIAN_POINT ( 'NONE',  ( 99.99999999999998579, 101.5015231886685854, -50.87500000273119127 ) ) ;
#18131 = CARTESIAN_POINT ( 'NONE',  ( -13.14518615778179544, 38.17226562608393436, 0.000000000000000000 ) ) ;
#18132 = CARTESIAN_POINT ( 'NONE',  ( 101.7677669529663547, 124.7000000000000028, -1.767766952966370209 ) ) ;
#18133 = CARTESIAN_POINT ( 'NONE',  ( 92.99999999999998579, 112.2744378736303190, -53.10000000000000142 ) ) ;
#18134 = AXIS2_PLACEMENT_3D ( 'NONE', #5232, #24895, #13898 ) ;
#18135 = CARTESIAN_POINT ( 'NONE',  ( 143.1451861577818079, 36.98164062608393010, -1.609821015232357215E-15 ) ) ;
#18136 = CARTESIAN_POINT ( 'NONE',  ( 13.14518615778179544, 37.18007812608393436, -1.609821015232357215E-15 ) ) ;
#18137 = CARTESIAN_POINT ( 'NONE',  ( -5.444914386472299306, 34.35234375108392868, 13.14518615778179722 ) ) ;
#18138 = CARTESIAN_POINT ( 'NONE',  ( -9.295050272127046043, 38.86679687608393863, -9.295050272127046043 ) ) ;
#18139 = CARTESIAN_POINT ( 'NONE',  ( 104.9999999999999858, 95.87499999726881583, -6.938893903907228378E-15 ) ) ;
#18140 = CARTESIAN_POINT ( 'NONE',  ( 2.493653234604083739E-15, 36.53515625216787299, 13.57481594606304576 ) ) ;
#18141 = CARTESIAN_POINT ( 'NONE',  ( 91.91746824999998466, 107.3738262389971680, -53.27500000273119696 ) ) ;
#18142 = CARTESIAN_POINT ( 'NONE',  ( 195.0000000000000000, 39.61093749999999147, 13.57481594606304576 ) ) ;
#18143 = CARTESIAN_POINT ( 'NONE',  ( 74.03144042245413914, 36.00000000000002132, 9.765766397119163500 ) ) ;
#18144 = ORIENTED_EDGE ( 'NONE', *, *, #3119, .F. ) ;
#18145 = CARTESIAN_POINT ( 'NONE',  ( -13.14518615778179189, 35.24531250108393721, 5.444914386472304635 ) ) ;
#18146 = CARTESIAN_POINT ( 'NONE',  ( 103.1528011352953342, 3.152801135295383084, 6.312500001365592084 ) ) ;
#18147 = CARTESIAN_POINT ( 'NONE',  ( 74.29505027212704249, 36.28710937608393294, -9.295050272127046043 ) ) ;
#18148 = CARTESIAN_POINT ( 'NONE',  ( 93.00000000000000000, 110.0000000000000000, -55.00000000000000711 ) ) ;
#18149 = CARTESIAN_POINT ( 'NONE',  ( 181.8548138422182205, 36.63437500108393863, 5.444914386472304635 ) ) ;
#18150 = CARTESIAN_POINT ( 'NONE',  ( 13.14518615778179722, 35.64218750108393863, -5.444914386472297529 ) ) ;
#18151 = ORIENTED_EDGE ( 'NONE', *, *, #5141, .T. ) ;
#18152 = CARTESIAN_POINT ( 'NONE',  ( 97.93301270000000613, 122.9500000010924765, -9.540979117872439019E-15 ) ) ;
#18153 = CARTESIAN_POINT ( 'NONE',  ( 99.99999999999998579, 92.31249999863440792, 4.458734124999981674 ) ) ;
#18154 = CARTESIAN_POINT ( 'NONE',  ( 195.0000000000000000, 36.98164062608393721, 13.14518615778179544 ) ) ;
#18155 = CARTESIAN_POINT ( 'NONE',  ( 95.00472066334982912, 103.1245878333314323, -49.57499999726881157 ) ) ;
#18156 = AXIS2_PLACEMENT_3D ( 'NONE', #18245, #1015, #10324 ) ;
#18157 = VERTEX_POINT ( 'NONE', #20182 ) ;
#18158 = EDGE_CURVE ( 'NONE', #1420, #21223, #6590, .T. ) ;
#18159 = CARTESIAN_POINT ( 'NONE',  ( 5.622872871577878406, 32.51679687499999716, 13.57481594606304576 ) ) ;
#18160 = CARTESIAN_POINT ( 'NONE',  ( -5.444914386472297529, 33.26093750108393721, -13.14518615778179900 ) ) ;
#18161 = CIRCLE ( 'NONE', #26341, 11.57481594606304398 ) ;
#18162 = ORIENTED_EDGE ( 'NONE', *, *, #19982, .F. ) ;
#18163 = CARTESIAN_POINT ( 'NONE',  ( 130.0000000000000000, 31.82226562608393650, -13.14518615778179544 ) ) ;
#18164 = CARTESIAN_POINT ( 'NONE',  ( 181.4251840539369596, 37.18007812716787441, 5.622872871577880183 ) ) ;
#18165 = CARTESIAN_POINT ( 'NONE',  ( 208.1451861577818079, 34.00507812608393721, -1.609821015232357215E-15 ) ) ;
#18166 = VERTEX_POINT ( 'NONE', #3219 ) ;
#18167 = CARTESIAN_POINT ( 'NONE',  ( 100.8561741729129295, 123.5000000010924879, -2.066987299999998751 ) ) ;
#18168 = FACE_OUTER_BOUND ( 'NONE', #16155, .T. ) ;
#18169 = CARTESIAN_POINT ( 'NONE',  ( 99.99999999999998579, 90.00000000000000000, -4.999999999999996447 ) ) ;
#18170 = CARTESIAN_POINT ( 'NONE',  ( 135.6228728715778971, 36.58476562716787583, 13.57481594606304576 ) ) ;
#18171 = CARTESIAN_POINT ( 'NONE',  ( 91.91746824999998466, 107.3738262389971680, -45.02500000273118985 ) ) ;
#18172 = DIRECTION ( 'NONE',  ( 6.123233995736778362E-17, 0.8660254037844380415, -0.5000000000000009992 ) ) ;
#18173 = DIRECTION ( 'NONE',  ( -0.000000000000000000, -0.000000000000000000, -1.000000000000000000 ) ) ;
#18174 = CARTESIAN_POINT ( 'NONE',  ( 195.0000000000000000, 40.55351562608393579, -13.14518615778179544 ) ) ;
#18175 = FILL_AREA_STYLE_COLOUR ( '', #19070 ) ;
#18176 = STYLED_ITEM ( 'NONE', ( #20467 ), #24660 ) ;
#18177 = CARTESIAN_POINT ( 'NONE',  ( 96.84719886470459471, -3.152801135295355994, 3.562500001365591196 ) ) ;
#18178 = EDGE_LOOP ( 'NONE', ( #4331, #2009, #16240, #26473 ) ) ;
#18179 = CARTESIAN_POINT ( 'NONE',  ( -9.598844408820454532, 35.64218750216787868, 9.598844408820459861 ) ) ;
#18180 = CARTESIAN_POINT ( 'NONE',  ( 98.15313185440925281, 4.458734125000016313, 6.250000001365592084 ) ) ;
#18181 = CARTESIAN_POINT ( 'NONE',  ( 87.00000000000000000, 97.00000000000000000, 12.99999999999999467 ) ) ;
#18182 = CARTESIAN_POINT ( 'NONE',  ( -13.14518615778179900, 35.74140625108393721, -5.444914386472297529 ) ) ;
#18183 = CARTESIAN_POINT ( 'NONE',  ( 99.99999999999998579, 94.62499999726881583, 4.999999999999984013 ) ) ;
#18184 = CARTESIAN_POINT ( 'NONE',  ( 102.0710678118655181, 95.68749999726881583, 4.999999999999919176 ) ) ;
#18185 = EDGE_CURVE ( 'NONE', #370, #9199, #11747, .T. ) ;
#18186 = CARTESIAN_POINT ( 'NONE',  ( 106.5389055433251002, 105.2492070361643215, -46.32500000273119412 ) ) ;
#18187 = CARTESIAN_POINT ( 'NONE',  ( -8.312177448680279460E-16, 39.31328125216787583, -13.57481594606304576 ) ) ;
#18188 = CARTESIAN_POINT ( 'NONE',  ( 102.1631189606246153, 116.6573956140660897, -53.09999999453764019 ) ) ;
#18189 = FACE_OUTER_BOUND ( 'NONE', #11099, .T. ) ;
#18190 = CARTESIAN_POINT ( 'NONE',  ( 130.0000000000000000, 40.40468749999999432, 13.57481594606304576 ) ) ;
#18191 = CARTESIAN_POINT ( 'NONE',  ( 143.5748159460630688, 33.45937499999999432, -1.662435489736055892E-15 ) ) ;
#18192 = ORIENTED_EDGE ( 'NONE', *, *, #3035, .T. ) ;
#18193 = LINE ( 'NONE', #15762, #25862 ) ;
#18194 = CARTESIAN_POINT ( 'NONE',  ( 5.444914386472297529, 32.56640625108394005, -13.14518615778179900 ) ) ;
#18195 = CARTESIAN_POINT ( 'NONE',  ( -8.312177448680279460E-16, 35.34453125216787583, -13.57481594606304576 ) ) ;
#18196 = CARTESIAN_POINT ( 'NONE',  ( 94.99999999999995737, 1.387778780781445676E-14, 10.12500000273118594 ) ) ;
#18197 = CARTESIAN_POINT ( 'NONE',  ( 143.1451861577818079, 33.01289062608393010, -1.609821015232357215E-15 ) ) ;
#18198 = ADVANCED_FACE ( 'NONE', ( #20473 ), #952, .F. ) ;
#18199 = CARTESIAN_POINT ( 'NONE',  ( 55.70494972787295751, 39.06523437608392868, 9.295050272127047819 ) ) ;
#18200 = ADVANCED_FACE ( 'NONE', ( #20611 ), #3500, .F. ) ;
#18201 = CARTESIAN_POINT ( 'NONE',  ( 7.171391216998964424, 31.99955315621561525, -11.52591757658528948 ) ) ;
#18202 = CARTESIAN_POINT ( 'NONE',  ( -5.444914386472297529, 39.61093750108393152, -13.14518615778179900 ) ) ;
#18203 = EDGE_CURVE ( 'NONE', #15512, #10978, #5504, .T. ) ;
#18204 = CARTESIAN_POINT ( 'NONE',  ( 92.45873412499997812, 110.0000000000000000, -46.18749999590323085 ) ) ;
#18205 = LINE ( 'NONE', #15483, #5317 ) ;
#18206 = CARTESIAN_POINT ( 'NONE',  ( 104.9952793366501567, 103.1245878333314465, -53.17499999726882010 ) ) ;
#18207 = FACE_OUTER_BOUND ( 'NONE', #9187, .T. ) ;
#18208 = DIRECTION ( 'NONE',  ( -0.000000000000000000, -1.000000000000000000, -0.000000000000000000 ) ) ;
#18209 = CARTESIAN_POINT ( 'NONE',  ( -13.14518615778179544, 40.65273437608393436, 0.000000000000000000 ) ) ;
#18210 = CARTESIAN_POINT ( 'NONE',  ( 97.50000000000000000, 125.0162387953032663, 0.1913417161825344548 ) ) ;
#18211 = EDGE_CURVE ( 'NONE', #1506, #8614, #4777, .T. ) ;
#18212 = CARTESIAN_POINT ( 'NONE',  ( 99.14382582708707048, 123.6000000010924680, -2.066987299999999195 ) ) ;
#18213 = CARTESIAN_POINT ( 'NONE',  ( 118.0647576233092764, 36.00000000000000711, -5.809862729997675501 ) ) ;
#18214 = DIRECTION ( 'NONE',  ( 0.000000000000000000, 0.000000000000000000, -1.000000000000000000 ) ) ;
#18215 = DIRECTION ( 'NONE',  ( -0.000000000000000000, -1.000000000000000000, -0.000000000000000000 ) ) ;
#18216 = CARTESIAN_POINT ( 'NONE',  ( 13.57481594606304576, 34.25312499999999716, -1.662435489736055892E-15 ) ) ;
#18217 = CARTESIAN_POINT ( 'NONE',  ( -13.14917398115171743, 36.00000000000000711, -1.058935892997135975 ) ) ;
#18218 =( BOUNDED_CURVE ( )  B_SPLINE_CURVE ( 2, ( #2558, #19648, #17796, #130, #17935, #17505, #26206 ),
 .UNSPECIFIED., .F., .T. ) 
 B_SPLINE_CURVE_WITH_KNOTS ( ( 3, 2, 2, 3 ),
 ( 0.8000000000000000444, 0.8199999999999999512, 0.8399999999999999689, 0.8500000005328695041 ),
 .UNSPECIFIED. ) 
 CURVE ( )  GEOMETRIC_REPRESENTATION_ITEM ( )  RATIONAL_B_SPLINE_CURVE ( ( 1.000000000000000000, 0.9510565162951535312, 1.000000000000000000, 0.9510565162951535312, 1.000000000000000000, 0.9755282568435521551, 0.9755282581475768211 ) ) 
 REPRESENTATION_ITEM ( '' )  );
#18219 = CARTESIAN_POINT ( 'NONE',  ( -9.295050272127046043, 34.30273437608393294, -9.295050272127046043 ) ) ;
#18220 = CARTESIAN_POINT ( 'NONE',  ( -13.14518615778179544, 32.61601562608393579, 0.000000000000000000 ) ) ;
#18221 = CARTESIAN_POINT ( 'NONE',  ( 9.295050272127046043, 34.69960937608393436, -9.295050272127046043 ) ) ;
#18222 = EDGE_CURVE ( 'NONE', #27857, #27010, #23578, .T. ) ;
#18223 = CARTESIAN_POINT ( 'NONE',  ( -8.312177448680279460E-16, 34.55078125216787299, -13.57481594606304576 ) ) ;
#18224 = CARTESIAN_POINT ( 'NONE',  ( 2.493653234604083739E-15, 40.40468749999999432, 13.57481594606304576 ) ) ;
#18225 = CARTESIAN_POINT ( 'NONE',  ( -8.312177448680279460E-16, 35.24531249999999716, -13.57481594606304576 ) ) ;
#18226 = CARTESIAN_POINT ( 'NONE',  ( 74.29505027212704249, 32.11992187608393579, 9.295050272127046043 ) ) ;
#18227 = DIRECTION ( 'NONE',  ( -0.000000000000000000, -1.000000000000000000, -0.000000000000000000 ) ) ;
#18228 = CARTESIAN_POINT ( 'NONE',  ( 102.0244715095044512, 123.0000000000000000, -1.474530169995667883 ) ) ;
#18229 = CARTESIAN_POINT ( 'NONE',  ( 2.493653234604083739E-15, 32.46718749999999432, 13.57481594606304576 ) ) ;
#18230 = CARTESIAN_POINT ( 'NONE',  ( 120.7049497278729575, 35.09648437608393579, -9.295050272127046043 ) ) ;
#18231 = EDGE_CURVE ( 'NONE', #8989, #19422, #20263, .T. ) ;
#18232 = ORIENTED_EDGE ( 'NONE', *, *, #8133, .F. ) ;
#18233 = CARTESIAN_POINT ( 'NONE',  ( 102.0710678118654329, 82.31250000000000000, 4.999999999999989342 ) ) ;
#18234 = AXIS2_PLACEMENT_3D ( 'NONE', #23656, #12927, #23516 ) ;
#18235 = CARTESIAN_POINT ( 'NONE',  ( 95.67376207875072680, 115.9545556584642867, -47.30000000000000426 ) ) ;
#18236 = CARTESIAN_POINT ( 'NONE',  ( 95.54126587499995082, 82.50000000136560629, 1.846868145590724986 ) ) ;
#18237 = CARTESIAN_POINT ( 'NONE',  ( 96.46446609406726225, 93.62500000000000000, 3.535533905932723986 ) ) ;
#18238 = CARTESIAN_POINT ( 'NONE',  ( 200.6228728715779255, 37.27929687499999289, 13.57481594606297115 ) ) ;
#18239 = STYLED_ITEM ( 'NONE', ( #17494 ), #17477 ) ;
#18240 = EDGE_CURVE ( 'NONE', #28031, #7991, #22095, .T. ) ;
#18241 = CARTESIAN_POINT ( 'NONE',  ( 92.99999999999998579, 110.0000000000000000, -55.00000000000001421 ) ) ;
#18242 = CARTESIAN_POINT ( 'NONE',  ( 74.59884440882045453, 39.90859374999999432, -9.598844408820458085 ) ) ;
#18243 = CARTESIAN_POINT ( 'NONE',  ( 13.57481594606304576, 37.52734375216787299, -1.662435489736055892E-15 ) ) ;
#18244 = ORIENTED_EDGE ( 'NONE', *, *, #3119, .T. ) ;
#18245 = CARTESIAN_POINT ( 'NONE',  ( 99.99999999999995737, 1.387778780781445676E-14, 34.79898987322334136 ) ) ;
#18246 = EDGE_CURVE ( 'NONE', #13216, #467, #4606, .T. ) ;
#18247 = CARTESIAN_POINT ( 'NONE',  ( 104.9999999999999716, 1.449011120738813565E-14, 14.49999999999999822 ) ) ;
#18248 = EDGE_LOOP ( 'NONE', ( #20605, #20448, #2237, #21985 ) ) ;
#18249 = CARTESIAN_POINT ( 'NONE',  ( -8.049105076161786076E-16, 34.99726562608393721, -13.14518615778179544 ) ) ;
#18250 = CARTESIAN_POINT ( 'NONE',  ( 195.0000000000000000, 32.56640625216787299, 13.57481594606304576 ) ) ;
#18251 = CARTESIAN_POINT ( 'NONE',  ( 5.444914386472297529, 32.36796875108393579, -13.14518615778179722 ) ) ;
#18252 = CARTESIAN_POINT ( 'NONE',  ( 97.92893218813451028, -4.999999999999989342, 13.31250000273118772 ) ) ;
#18253 = PLANE ( 'NONE',  #25282 ) ;
#18254 = CARTESIAN_POINT ( 'NONE',  ( -8.049105076161786076E-16, 36.58476562608393579, -13.14518615778179544 ) ) ;
#18255 = CARTESIAN_POINT ( 'NONE',  ( 93.00000000000001421, 107.7255621263696668, -50.40000000546238113 ) ) ;
#18256 = CARTESIAN_POINT ( 'NONE',  ( 103.1528011352953484, 90.43749999863440792, -3.152801135295366208 ) ) ;
#18257 = CARTESIAN_POINT ( 'NONE',  ( 2.493653234604083739E-15, 34.84843749999999574, 13.57481594606304576 ) ) ;
#18258 = CARTESIAN_POINT ( 'NONE',  ( 0.000000000000000000, 0.000000000000000000, 0.000000000000000000 ) ) ;
#18259 = CARTESIAN_POINT ( 'NONE',  ( 70.62287287157786864, 36.88242187716787157, -13.57481594606304753 ) ) ;
#18260 = CARTESIAN_POINT ( 'NONE',  ( 104.4587341249999639, 1.442382525525748735E-14, 5.187500001365592972 ) ) ;
#18261 = CARTESIAN_POINT ( 'NONE',  ( 105.6631189606246295, 114.1144967660473242, -53.30000000546237970 ) ) ;
#18262 = CIRCLE ( 'NONE', #26916, 4.999999999999989342 ) ;
#18263 = CARTESIAN_POINT ( 'NONE',  ( 95.54126587499996504, 1.846868145590750077, 8.375000001365592084 ) ) ;
#18264 = CARTESIAN_POINT ( 'NONE',  ( 95.00472066334982912, 116.8754121666685393, -45.42500000273119554 ) ) ;
#18265 = CARTESIAN_POINT ( 'NONE',  ( 98.15313185440925281, 92.24999999863439371, 4.458734124999979898 ) ) ;
#18266 = CARTESIAN_POINT ( 'NONE',  ( 103.5355339059327093, 3.535533905932755072, 3.624999999999999556 ) ) ;
#18267 = CARTESIAN_POINT ( 'NONE',  ( 104.9952793366501567, 103.1245878333314465, -52.92499999726882010 ) ) ;
#18268 = CARTESIAN_POINT ( 'NONE',  ( 9.295050272127046043, 32.51679687608393721, -9.295050272127046043 ) ) ;
#18269 = ORIENTED_EDGE ( 'NONE', *, *, #21043, .F. ) ;
#18270 =( BOUNDED_CURVE ( )  B_SPLINE_CURVE ( 2, ( #149, #17525, #2851, #4564, #22099, #13225, #11520, #21957, #8977 ),
 .UNSPECIFIED., .F., .T. ) 
 B_SPLINE_CURVE_WITH_KNOTS ( ( 3, 2, 2, 2, 3 ),
 ( 0.7708333333333333703, 0.7812500000000000000, 0.7916666666666665186, 0.8020833333333332593, 0.8124999999999998890 ),
 .UNSPECIFIED. ) 
 CURVE ( )  GEOMETRIC_REPRESENTATION_ITEM ( )  RATIONAL_B_SPLINE_CURVE ( ( 1.000000000000000000, 0.9238795325112867385, 1.000000000000000000, 0.9238795325112867385, 1.000000000000000000, 0.9238795325112867385, 1.000000000000000000, 0.9238795325112875156, 0.9999999999999992228 ) ) 
 REPRESENTATION_ITEM ( '' )  );
#18271 = DIRECTION ( 'NONE',  ( 0.000000000000000000, 0.000000000000000000, 1.000000000000000000 ) ) ;
#18272 = CARTESIAN_POINT ( 'NONE',  ( 102.0710678118654329, -4.999999999999989342, 1.312499999999999334 ) ) ;
#18273 = AXIS2_PLACEMENT_3D ( 'NONE', #22735, #23290, #22875 ) ;
#18274 = EDGE_CURVE ( 'NONE', #19519, #8183, #17163, .T. ) ;
#18275 = CARTESIAN_POINT ( 'NONE',  ( 189.5550856135277229, 35.93984375108392726, 13.14518615778179722 ) ) ;
#18276 = VERTEX_POINT ( 'NONE', #9898 ) ;
#18277 = CARTESIAN_POINT ( 'NONE',  ( 185.8198241863518945, 55.00000000000000000, -15.00000000000000000 ) ) ;
#18278 = CARTESIAN_POINT ( 'NONE',  ( 96.84719886470459471, -3.152801135295355994, 9.812500001365593860 ) ) ;
#18279 = ORIENTED_EDGE ( 'NONE', *, *, #7755, .F. ) ;
#18280 = CARTESIAN_POINT ( 'NONE',  ( 102.1631189606246295, 103.3426043859339103, -45.40000000000001279 ) ) ;
#18281 = CARTESIAN_POINT ( 'NONE',  ( 13.14518615778179900, 35.44375000108393436, -5.444914386472297529 ) ) ;
#18282 = CARTESIAN_POINT ( 'NONE',  ( 101.7677669529663547, 124.5000000000000000, 1.767766952966350891 ) ) ;
#18283 = CARTESIAN_POINT ( 'NONE',  ( 97.50000000000000000, 123.3499999999999943, -1.035533905932742416 ) ) ;
#18284 = CARTESIAN_POINT ( 'NONE',  ( 116.8548138422182063, 39.01562500108393294, 5.444914386472304635 ) ) ;
#18285 = CARTESIAN_POINT ( 'NONE',  ( 13.14518615778179544, 37.97382812608393721, -1.609821015232357215E-15 ) ) ;
#18286 = CARTESIAN_POINT ( 'NONE',  ( -8.049105076161786076E-16, 34.00507812608393721, -13.14518615778179544 ) ) ;
#18287 = CARTESIAN_POINT ( 'NONE',  ( 95.54126587499999346, 90.99999999863439371, -1.846868145590737864 ) ) ;
#18288 = CARTESIAN_POINT ( 'NONE',  ( 66.94732592208626443, 51.47162402671428083, -15.00000000000065725 ) ) ;
#18289 = CARTESIAN_POINT ( 'NONE',  ( 93.46109445667491400, 105.2492070361643215, -51.17500000273119554 ) ) ;
#18290 = ORIENTED_EDGE ( 'NONE', *, *, #17674, .T. ) ;
#18291 = DIRECTION ( 'NONE',  ( -0.000000000000000000, 1.000000000000000000, -0.000000000000000000 ) ) ;
#18292 = CARTESIAN_POINT ( 'NONE',  ( -9.295050272127044266, 36.08867187608393579, 9.295050272127047819 ) ) ;
#18293 = CARTESIAN_POINT ( 'NONE',  ( 99.99999999999995737, 4.458734125000016313, 6.437500001365592084 ) ) ;
#18294 = CARTESIAN_POINT ( 'NONE',  ( 74.29505027212704249, 37.08085937608393579, -9.295050272127046043 ) ) ;
#18295 = CARTESIAN_POINT ( 'NONE',  ( 94.99999999999995737, 1.387778780781445676E-14, 1.999999999999998224 ) ) ;
#18296 = VERTEX_POINT ( 'NONE', #3641 ) ;
#18297 = CARTESIAN_POINT ( 'NONE',  ( -8.049105076161786076E-16, 34.20351562608394147, -13.14518615778179544 ) ) ;
#18298 = CARTESIAN_POINT ( 'NONE',  ( 98.96446609406727646, 122.8500000021849416, 2.499999999999977796 ) ) ;
#18299 = CARTESIAN_POINT ( 'NONE',  ( 96.84719886470463734, 90.93749999863440792, -3.152801135295366208 ) ) ;
#18300 = CARTESIAN_POINT ( 'NONE',  ( 185.7049497278729575, 38.27148437608393294, -9.295050272127046043 ) ) ;
#18301 = CARTESIAN_POINT ( 'NONE',  ( 93.46109445667489979, 114.7507929638356785, -50.07499999726882578 ) ) ;
#18302 = ORIENTED_EDGE ( 'NONE', *, *, #7618, .T. ) ;
#18303 = CARTESIAN_POINT ( 'NONE',  ( 5.622872871577871301, 34.40195312499999858, -13.57481594606304753 ) ) ;
#18304 = CARTESIAN_POINT ( 'NONE',  ( -9.295050272127046043, 32.51679687608393721, -9.295050272127046043 ) ) ;
#18305 = ORIENTED_EDGE ( 'NONE', *, *, #17805, .T. ) ;
#18306 = EDGE_LOOP ( 'NONE', ( #28086, #4589, #11128, #11383 ) ) ;
#18307 = CARTESIAN_POINT ( 'NONE',  ( 139.2950502721270425, 33.11210937608393579, 9.295050272127046043 ) ) ;
#18308 = CARTESIAN_POINT ( 'NONE',  ( 55.70494972787295751, 31.72304687608393081, -9.295050272127046043 ) ) ;
#18309 = CARTESIAN_POINT ( 'NONE',  ( 100.8561741729129295, 122.9000000010924794, -2.066987299999998751 ) ) ;
#18310 = CARTESIAN_POINT ( 'NONE',  ( 189.5550856135277229, 34.55078125108393294, 13.14518615778179722 ) ) ;
#18311 = EDGE_LOOP ( 'NONE', ( #26254, #17342, #20321, #15293 ) ) ;
#18312 = CARTESIAN_POINT ( 'NONE',  ( 97.92893218813451028, -4.999999999999989342, 13.18750000000000000 ) ) ;
#18313 = CARTESIAN_POINT ( 'NONE',  ( 104.9999999999999716, 2.071067811865491937, 8.687500002731184168 ) ) ;
#18314 = CARTESIAN_POINT ( 'NONE',  ( 99.99999999999995737, 1.387778780781445676E-14, 34.79898987322334136 ) ) ;
#18315 = CARTESIAN_POINT ( 'NONE',  ( 143.5748159460630688, 39.11484375216787157, -1.662435489736055892E-15 ) ) ;
#18316 = CARTESIAN_POINT ( 'NONE',  ( 106.5389055433251002, 114.7507929638356785, -45.92500000273119554 ) ) ;
#18317 = DIRECTION ( 'NONE',  ( 0.000000000000000000, 1.000000000000000000, 0.000000000000000000 ) ) ;
#18318 = LINE ( 'NONE', #27026, #3246 ) ;
#18319 = CARTESIAN_POINT ( 'NONE',  ( 65.32860027656705881, 53.49358765998906762, 14.99999999999997868 ) ) ;
#18320 = EDGE_LOOP ( 'NONE', ( #24399, #7992, #11813, #21727 ) ) ;
#18321 = EDGE_CURVE ( 'NONE', #28194, #4535, #1542, .T. ) ;
#18322 = ORIENTED_EDGE ( 'NONE', *, *, #4456, .F. ) ;
#18323 = FILL_AREA_STYLE_COLOUR ( '', #4528 ) ;
#18324 = CARTESIAN_POINT ( 'NONE',  ( 99.99999999999995737, 4.458734125000016313, 5.187500001365592972 ) ) ;
#18325 = ORIENTED_EDGE ( 'NONE', *, *, #19766, .T. ) ;
#18326 = CARTESIAN_POINT ( 'NONE',  ( -13.57481594606304576, 35.54296875216788010, 0.000000000000000000 ) ) ;
#18327 = CARTESIAN_POINT ( 'NONE',  ( 96.84719886470459471, -3.152801135295355994, 8.562500001365592084 ) ) ;
#18328 = DIRECTION ( 'NONE',  ( -0.000000000000000000, -1.000000000000000000, -0.000000000000000000 ) ) ;
#18329 = CARTESIAN_POINT ( 'NONE',  ( 189.3771271284222166, 40.15664062716787441, -13.57481594606315412 ) ) ;
#18330 = CARTESIAN_POINT ( 'NONE',  ( 74.29505027212704249, 33.11210937608393579, 9.295050272127046043 ) ) ;
#18331 = DIRECTION ( 'NONE',  ( -6.123233995736778362E-17, -0.8660254037844380415, -0.5000000000000009992 ) ) ;
#18332 = CARTESIAN_POINT ( 'NONE',  ( 102.4976396683250925, 102.3130555110000159, -48.52500000273119696 ) ) ;
#18333 = CARTESIAN_POINT ( 'NONE',  ( -13.57481594606304398, 38.66835937499999432, 5.622872871577880183 ) ) ;
#18334 = CARTESIAN_POINT ( 'NONE',  ( 92.99999999999995737, 112.2744378736303048, -52.59999999453763309 ) ) ;
#18335 = CARTESIAN_POINT ( 'NONE',  ( 5.323790963956049893, 54.47170356488337006, 14.99999999999999645 ) ) ;
#18336 = FACE_OUTER_BOUND ( 'NONE', #25164, .T. ) ;
#18337 = CARTESIAN_POINT ( 'NONE',  ( 116.4251840539369596, 34.69960937499999432, 5.622872871577880183 ) ) ;
#18338 = AXIS2_PLACEMENT_3D ( 'NONE', #17600, #24444, #26305 ) ;
#18339 = VERTEX_POINT ( 'NONE', #23857 ) ;
#18340 = CARTESIAN_POINT ( 'NONE',  ( 97.83688103937535629, 116.6573956140660897, -51.40000000000001279 ) ) ;
#18341 = CARTESIAN_POINT ( 'NONE',  ( 13.14518615778179900, 33.16171875108393863, 5.444914386472293977 ) ) ;
#18342 = CARTESIAN_POINT ( 'NONE',  ( -8.312177448680279460E-16, 32.96328125216787441, -13.57481594606304576 ) ) ;
#18343 = CARTESIAN_POINT ( 'NONE',  ( 96.46446609406721961, 3.535533905932755072, 10.00000000273118594 ) ) ;
#18344 = CARTESIAN_POINT ( 'NONE',  ( 143.1451861577818079, 34.55078125108393294, 5.444914386472293977 ) ) ;
#18345 = PRODUCT_DEFINITION_SHAPE ( 'NONE', 'NONE',  #27055 ) ;
#18346 = CARTESIAN_POINT ( 'NONE',  ( 59.37712712842213136, 32.21914062716787441, -13.57481594606304753 ) ) ;
#18347 = CARTESIAN_POINT ( 'NONE',  ( 13.14518615778179900, 39.41250000108393436, -5.444914386472297529 ) ) ;
#18348 = CARTESIAN_POINT ( 'NONE',  ( 3.755639919285892248, 31.78804746655075775, -13.14518615778179544 ) ) ;
#18349 = LINE ( 'NONE', #16200, #5352 ) ;
#18350 = CARTESIAN_POINT ( 'NONE',  ( 13.57481594606304576, 39.11484375216787157, -1.662435489736055892E-15 ) ) ;
#18351 = CARTESIAN_POINT ( 'NONE',  ( 99.99999999999995737, 82.37500000273119838, 4.999999999999990230 ) ) ;
#18352 = CARTESIAN_POINT ( 'NONE',  ( -5.622872871577965448, 31.72304687716787086, 13.57481594606295161 ) ) ;
#18353 = CARTESIAN_POINT ( 'NONE',  ( 98.23223304703363112, 124.9069999999781402, -1.767766952966370209 ) ) ;
#18354 = AXIS2_PLACEMENT_3D ( 'NONE', #14031, #11750, #22756 ) ;
#18355 = CARTESIAN_POINT ( 'NONE',  ( -8.312177448680279460E-16, 36.03906250000000000, -13.57481594606304576 ) ) ;
#18356 = CARTESIAN_POINT ( 'NONE',  ( 189.3771271284219608, 39.56132812500000284, 13.57481594606290720 ) ) ;
#18357 = CYLINDRICAL_SURFACE ( 'NONE', #24704, 2.499999999999995115 ) ;
#18358 = CARTESIAN_POINT ( 'NONE',  ( -13.57481594606304576, 35.49335937499999005, 5.622872871577880183 ) ) ;
#18359 = CARTESIAN_POINT ( 'NONE',  ( -12.56650672479864461, 36.00000000000000000, -4.295155080288879823 ) ) ;
#18360 = CARTESIAN_POINT ( 'NONE',  ( 5.444914386472297529, 34.15390625108393863, -13.14518615778179900 ) ) ;
#18361 = CARTESIAN_POINT ( 'NONE',  ( -5.444914386472299306, 31.97109375108393436, 13.14518615778179722 ) ) ;
#18362 = EDGE_CURVE ( 'NONE', #13578, #9543, #23913, .T. ) ;
#18363 = CARTESIAN_POINT ( 'NONE',  ( 9.295050272127047819, 34.50117187608393010, 9.295050272127046043 ) ) ;
#18364 = CARTESIAN_POINT ( 'NONE',  ( -5.622872871577873077, 36.18789062716787441, -13.57481594606304753 ) ) ;
#18365 = CARTESIAN_POINT ( 'NONE',  ( 13.57481594606304931, 37.47773437716787015, 5.622872871577868636 ) ) ;
#18366 = CARTESIAN_POINT ( 'NONE',  ( 95.54126587499995082, 84.37500000136562051, -1.846868145590750077 ) ) ;
#18367 = CARTESIAN_POINT ( 'NONE',  ( 78.14518615778179367, 33.85625000108393579, -5.444914386472297529 ) ) ;
#18368 = EDGE_CURVE ( 'NONE', #24154, #15008, #26851, .T. ) ;
#18369 = CARTESIAN_POINT ( 'NONE',  ( 95.00472066334982912, 116.8754121666685393, -53.67500000273118843 ) ) ;
#18370 = CARTESIAN_POINT ( 'NONE',  ( 195.0000000000000000, 40.80156249999999574, -13.57481594606304576 ) ) ;
#18371 = CARTESIAN_POINT ( 'NONE',  ( 130.0000000000000000, 37.72578125216787726, -13.57481594606304576 ) ) ;
#18372 = CARTESIAN_POINT ( 'NONE',  ( -9.598844408820458085, 32.16953124999999147, -9.598844408820458085 ) ) ;
#18373 = CARTESIAN_POINT ( 'NONE',  ( 97.50236033167490746, 117.6869444889999841, -52.27499999726882862 ) ) ;
#18374 = CARTESIAN_POINT ( 'NONE',  ( 130.0000000000000000, 33.01289062608393721, 13.14518615778179544 ) ) ;
#18375 = ORIENTED_EDGE ( 'NONE', *, *, #5863, .F. ) ;
#18376 = CARTESIAN_POINT ( 'NONE',  ( 94.99999999999995737, 81.06250000000000000, 2.071067811865466624 ) ) ;
#18377 = CARTESIAN_POINT ( 'NONE',  ( 107.0000000000000000, 110.0000000000000000, -46.00000000000001421 ) ) ;
#18378 = CARTESIAN_POINT ( 'NONE',  ( 103.1528011352953342, 83.81250000136560629, 3.152801135295355106 ) ) ;
#18379 = CARTESIAN_POINT ( 'NONE',  ( 95.00000000000000000, 90.43750000000000000, -2.071067811865479058 ) ) ;
#18380 = CARTESIAN_POINT ( 'NONE',  ( 120.4011555911795455, 38.51953124999999289, -9.598844408820458085 ) ) ;
#18381 = EDGE_CURVE ( 'NONE', #22191, #14907, #21014, .T. ) ;
#18382 = VECTOR ( 'NONE', #16204, 1000.000000000000000 ) ;
#18383 = CARTESIAN_POINT ( 'NONE',  ( 108.0825317499999869, 112.6261737610028320, -48.52499999726882152 ) ) ;
#18384 = CARTESIAN_POINT ( 'NONE',  ( 185.7049497278729575, 32.71523437608393436, 9.295050272127047819 ) ) ;
#18385 = CARTESIAN_POINT ( 'NONE',  ( 5.622872871577878406, 37.37851562716787157, 13.57481594606304576 ) ) ;
#18386 = ORIENTED_EDGE ( 'NONE', *, *, #11414, .F. ) ;
#18387 = CARTESIAN_POINT ( 'NONE',  ( 94.99999999999995737, 1.387778780781445676E-14, 9.999999999999998224 ) ) ;
#18388 = ORIENTED_EDGE ( 'NONE', *, *, #7194, .T. ) ;
#18389 = CARTESIAN_POINT ( 'NONE',  ( -13.14518615778179189, 37.62656250108393863, 5.444914386472304635 ) ) ;
#18390 = CARTESIAN_POINT ( 'NONE',  ( 185.7049497278729575, 40.45429687608393721, -9.295050272127046043 ) ) ;
#18391 =( BOUNDED_CURVE ( )  B_SPLINE_CURVE ( 2, ( #16723, #1627, #3895, #18855, #8166, #16858, #23146, #23421, #25557 ),
 .UNSPECIFIED., .F., .F. ) 
 B_SPLINE_CURVE_WITH_KNOTS ( ( 3, 2, 2, 2, 3 ),
 ( 0.8958333333333335924, 0.9062500000000002220, 0.9166666666666667407, 0.9270833333333334814, 0.9375000000000000000 ),
 .UNSPECIFIED. ) 
 CURVE ( )  GEOMETRIC_REPRESENTATION_ITEM ( )  RATIONAL_B_SPLINE_CURVE ( ( 0.9999999999999983347, 0.9238795325112884038, 1.000000000000000000, 0.9238795325112867385, 1.000000000000000000, 0.9238795325112867385, 1.000000000000000000, 0.9238795325112867385, 1.000000000000000000 ) ) 
 REPRESENTATION_ITEM ( '' )  );
#18392 = CARTESIAN_POINT ( 'NONE',  ( 13.14518615778179544, 32.21914062608393436, -1.609821015232357215E-15 ) ) ;
#18393 = CARTESIAN_POINT ( 'NONE',  ( 96.46446609406721961, -3.535533905932727539, 12.25000000273118594 ) ) ;
#18394 = CARTESIAN_POINT ( 'NONE',  ( 124.5550856135277087, 40.40468750108393436, -13.14518615778179722 ) ) ;
#18395 = CARTESIAN_POINT ( 'NONE',  ( -9.295050272127046043, 31.92148437608393508, -9.295050272127046043 ) ) ;
#18396 = CARTESIAN_POINT ( 'NONE',  ( 116.8548138422182063, 32.66562500108393863, 5.444914386472304635 ) ) ;
#18397 = CARTESIAN_POINT ( 'NONE',  ( 78.57481594606304043, 32.71523437500000142, -5.622872871577873077 ) ) ;
#18398 = CARTESIAN_POINT ( 'NONE',  ( 99.99999999999998579, 124.0000000000000000, -2.499999999999997780 ) ) ;
#18399 = EDGE_CURVE ( 'NONE', #15569, #13131, #157, .T. ) ;
#18400 = DIRECTION ( 'NONE',  ( 0.000000000000000000, 0.000000000000000000, 1.000000000000000000 ) ) ;
#18401 = CARTESIAN_POINT ( 'NONE',  ( 99.99999999999995737, 85.00000000000000000, -5.000000000000018652 ) ) ;
#18402 = CARTESIAN_POINT ( 'NONE',  ( 95.54126587499995082, 1.846868145590750077, 6.625000001365592084 ) ) ;
#18403 = CARTESIAN_POINT ( 'NONE',  ( 99.99999999999998579, 138.0000000000000000, -5.204170427930421283E-15 ) ) ;
#18404 = CARTESIAN_POINT ( 'NONE',  ( 95.54126587499996504, 1.846868145590750077, 10.37500000136559208 ) ) ;
#18405 = CARTESIAN_POINT ( 'NONE',  ( 104.3262379212492590, 115.9545556584642867, -51.20000000546237828 ) ) ;
#18406 = CYLINDRICAL_SURFACE ( 'NONE', #23197, 7.000000000000006217 ) ;
#18407 = PLANE ( 'NONE',  #24388 ) ;
#18408 = CARTESIAN_POINT ( 'NONE',  ( 95.00472066334981491, 103.1245878333314465, -53.32499999726881157 ) ) ;
#18409 = CARTESIAN_POINT ( 'NONE',  ( -9.295050272127046043, 33.50898437608393010, -9.295050272127046043 ) ) ;
#18410 = ADVANCED_FACE ( 'NONE', ( #20010 ), #22147, .T. ) ;
#18411 = ORIENTED_EDGE ( 'NONE', *, *, #7391, .F. ) ;
#18412 = CARTESIAN_POINT ( 'NONE',  ( 120.8198241863519797, 55.00000000000014211, -10.00000000000000000 ) ) ;
#18413 = CYLINDRICAL_SURFACE ( 'NONE', #6112, 5.000000000000000000 ) ;
#18414 = DIRECTION ( 'NONE',  ( 0.000000000000000000, 0.000000000000000000, -1.000000000000000000 ) ) ;
#18415 = EDGE_CURVE ( 'NONE', #6416, #13933, #8491, .T. ) ;
#18416 = CARTESIAN_POINT ( 'NONE',  ( 200.4449143864723055, 36.33671875108394289, -13.14518615778179900 ) ) ;
#18417 = VERTEX_POINT ( 'NONE', #3325 ) ;
#18418 = CARTESIAN_POINT ( 'NONE',  ( 200.3654965680425732, 54.48174559707338460, -15.00000000000000355 ) ) ;
#18419 = CARTESIAN_POINT ( 'NONE',  ( 98.15313185440925281, -4.458734124999987891, 11.87500000136559031 ) ) ;
#18420 = EDGE_LOOP ( 'NONE', ( #5167, #6714, #2495, #7427 ) ) ;
#18421 = CARTESIAN_POINT ( 'NONE',  ( 91.91746824999998466, 112.6261737610028320, -49.47500000273119269 ) ) ;
#18422 = CARTESIAN_POINT ( 'NONE',  ( 9.295050272127047819, 36.08867187608392868, 9.295050272127046043 ) ) ;
#18423 = CARTESIAN_POINT ( 'NONE',  ( 200.6228728715778686, 40.05742187716786873, -13.57481594606304753 ) ) ;
#18424 = CARTESIAN_POINT ( 'NONE',  ( 98.96446609406726225, 123.5500000000000114, 2.499999999999972022 ) ) ;
#18425 = CARTESIAN_POINT ( 'NONE',  ( 143.1451861577818079, 37.82500000108392868, -5.444914386472297529 ) ) ;
#18426 = CARTESIAN_POINT ( 'NONE',  ( 13.14518615778179722, 36.33671875108393579, 5.444914386472293977 ) ) ;
#18427 = CARTESIAN_POINT ( 'NONE',  ( 3.755639919285892248, 31.58960996655074993, -13.14518615778179544 ) ) ;
#18428 = AXIS2_PLACEMENT_3D ( 'NONE', #14009, #7752, #27160 ) ;
#18429 = CARTESIAN_POINT ( 'NONE',  ( 96.84719886470463734, 93.93749999863440792, -3.152801135295366208 ) ) ;
#18430 = DIRECTION ( 'NONE',  ( 0.000000000000000000, 4.625929269271485914E-16, 1.000000000000000000 ) ) ;
#18431 = CARTESIAN_POINT ( 'NONE',  ( 93.46109445667491400, 114.7507929638356785, -53.57500000273119412 ) ) ;
#18432 = VERTEX_POINT ( 'NONE', #14690 ) ;
#18433 = CARTESIAN_POINT ( 'NONE',  ( 1.662435489736055892E-15, 36.00000000000000000, 13.57481594606304576 ) ) ;
#18434 =( BOUNDED_CURVE ( )  B_SPLINE_CURVE ( 2, ( #26159, #11170, #21609, #24169, #4646, #8634, #6627, #26452, #12748 ),
 .UNSPECIFIED., .F., .F. ) 
 B_SPLINE_CURVE_WITH_KNOTS ( ( 3, 2, 2, 2, 3 ),
 ( 0.2499999999999998335, 0.2916666666666665741, 0.3333333333333332593, 0.3750000000000000000, 0.4166666666666667407 ),
 .UNSPECIFIED. ) 
 CURVE ( )  GEOMETRIC_REPRESENTATION_ITEM ( )  RATIONAL_B_SPLINE_CURVE ( ( 1.000000000000000222, 0.9238795325112864054, 1.000000000000000000, 0.9238795325112867385, 1.000000000000000000, 0.9238795325112867385, 1.000000000000000000, 0.9238795325112866275, 1.000000000000000000 ) ) 
 REPRESENTATION_ITEM ( '' )  );
#18435 = CARTESIAN_POINT ( 'NONE',  ( 5.444914386472297529, 37.32890625108393579, -13.14518615778179900 ) ) ;
#18436 = CARTESIAN_POINT ( 'NONE',  ( 104.4587341249999781, 1.846868145590750521, 5.250000001365592972 ) ) ;
#18437 = CARTESIAN_POINT ( 'NONE',  ( 74.29505027212704249, 36.08867187608392868, 9.295050272127046043 ) ) ;
#18438 = CARTESIAN_POINT ( 'NONE',  ( -9.598844408820454532, 38.81718750216787583, 9.598844408820459861 ) ) ;
#18439 = EDGE_CURVE ( 'NONE', #144, #13739, #22556, .T. ) ;
#18440 = B_SPLINE_CURVE_WITH_KNOTS ( 'NONE', 3,
 ( #410, #17360, #8949, #17215, #17640, #23779, #8668, #25920, #9094, #15347, #17788, #6394, #24062, #6806, #13201, #19640, #26491, #21935 ),
 .UNSPECIFIED., .F., .F.,
 ( 4, 2, 2, 2, 2, 2, 2, 2, 4 ),
 ( 0.000000000000000000, 0.004618502246277245149, 0.006927753369415865989, 0.009237004492554486829, 0.01039163005412375301, 0.01154625561569302093, 0.01385550673883156371, 0.01616475786197010128, 0.01847400898510864406 ),
 .UNSPECIFIED. ) ;
#18441 = DIRECTION ( 'NONE',  ( 0.000000000000000000, 1.000000000000000000, -1.156482317317871478E-16 ) ) ;
#18442 = CARTESIAN_POINT ( 'NONE',  ( 204.1801758136480203, 50.00000000000000000, 9.999999999999946709 ) ) ;
#18443 = EDGE_LOOP ( 'NONE', ( #3587, #5028, #9334, #13865 ) ) ;
#18444 = CARTESIAN_POINT ( 'NONE',  ( 5.444914386472302859, 36.23750000108393721, 13.14518615778179189 ) ) ;
#18445 = CARTESIAN_POINT ( 'NONE',  ( 101.0355339059327378, 123.2500000021849758, -2.499999999999997780 ) ) ;
#18446 = CARTESIAN_POINT ( 'NONE',  ( 95.54126587499999346, 93.12499999863439371, 1.846868145590722543 ) ) ;
#18447 = CARTESIAN_POINT ( 'NONE',  ( 94.99999999999995737, 1.387778780781445676E-14, 3.125000002731185944 ) ) ;
#18448 = CARTESIAN_POINT ( 'NONE',  ( 108.0825317499999869, 107.3738262389971538, -48.97499999726881015 ) ) ;
#18449 = VECTOR ( 'NONE', #20597, 1000.000000000000000 ) ;
#18450 = CARTESIAN_POINT ( 'NONE',  ( 2.493653234604083739E-15, 34.05468749999999289, 13.57481594606304576 ) ) ;
#18451 = CARTESIAN_POINT ( 'NONE',  ( 9.295050272127047819, 34.50117187608393010, 9.295050272127046043 ) ) ;
#18452 = ORIENTED_EDGE ( 'NONE', *, *, #14367, .F. ) ;
#18453 = LINE ( 'NONE', #27811, #26143 ) ;
#18454 = CARTESIAN_POINT ( 'NONE',  ( 7.020078988959679300, 31.47038648902007907, -11.28272846253492112 ) ) ;
#18455 = ORIENTED_EDGE ( 'NONE', *, *, #26275, .F. ) ;
#18456 = CARTESIAN_POINT ( 'NONE',  ( -8.312177448680279460E-16, 32.96328125216787441, -13.57481594606304576 ) ) ;
#18457 = CARTESIAN_POINT ( 'NONE',  ( 195.0000000000000000, 35.39414062608393863, 13.14518615778179544 ) ) ;
#18458 = ORIENTED_EDGE ( 'NONE', *, *, #12606, .F. ) ;
#18459 = CARTESIAN_POINT ( 'NONE',  ( 99.14382582708708469, 123.6000000010924680, -2.066987299999998751 ) ) ;
#18460 = CARTESIAN_POINT ( 'NONE',  ( 8.211314015175984693, 50.68678854790367438, -14.99999999999861799 ) ) ;
#18461 = CARTESIAN_POINT ( 'NONE',  ( 191.8834079195341928, 53.90895096933309816, 14.99999999999995026 ) ) ;
#18462 = CARTESIAN_POINT ( 'NONE',  ( 130.0000000000000000, 39.31328125216787583, -13.57481594606304576 ) ) ;
#18463 = CARTESIAN_POINT ( 'NONE',  ( 65.00000000000000000, 36.00000000000000000, -7.517135062566165128E-15 ) ) ;
#18464 = DIRECTION ( 'NONE',  ( -0.000000000000000000, -0.000000000000000000, -1.000000000000000000 ) ) ;
#18465 = CARTESIAN_POINT ( 'NONE',  ( 73.39593874129975859, 54.99999999495008041, 14.99999999999997691 ) ) ;
#18466 = VERTEX_POINT ( 'NONE', #19271 ) ;
#18467 = ORIENTED_EDGE ( 'NONE', *, *, #7618, .F. ) ;
#18468 = VERTEX_POINT ( 'NONE', #12693 ) ;
#18469 = CARTESIAN_POINT ( 'NONE',  ( 99.99999999999995737, -4.458734124999988779, 13.93750000136559208 ) ) ;
#18470 = CARTESIAN_POINT ( 'NONE',  ( 104.9999999999999716, 2.071067811865496822, 12.68750000273118772 ) ) ;
#18471 = CARTESIAN_POINT ( 'NONE',  ( 99.99999999999995737, -4.458734124999988779, 2.687500001365592528 ) ) ;
#18472 = CARTESIAN_POINT ( 'NONE',  ( 139.5988444088204687, 38.22187500216787015, 9.598844408820456309 ) ) ;
#18473 = CARTESIAN_POINT ( 'NONE',  ( 74.29505027212704249, 33.31054687608394005, -9.295050272127046043 ) ) ;
#18474 = LINE ( 'NONE', #11889, #10875 ) ;
#18475 = CARTESIAN_POINT ( 'NONE',  ( 108.0825317500000011, 112.6261737610028320, -48.02500000273118985 ) ) ;
#18476 = CARTESIAN_POINT ( 'NONE',  ( 1.137167824540872951, 35.99999999999998579, 13.09590655363602707 ) ) ;
#18477 = AXIS2_PLACEMENT_3D ( 'NONE', #20555, #9844, #9707 ) ;
#18478 = CARTESIAN_POINT ( 'NONE',  ( 92.99999999999998579, 110.0000000000000000, -52.49999999453763877 ) ) ;
#18479 = DIRECTION ( 'NONE',  ( 0.000000000000000000, 0.000000000000000000, 1.000000000000000000 ) ) ;
#18480 = CARTESIAN_POINT ( 'NONE',  ( 96.46446609406726225, 91.24999999726880162, -3.535533905932738197 ) ) ;
#18481 = CARTESIAN_POINT ( 'NONE',  ( 143.5748159460630404, 35.79101562499999289, 5.622872871577869525 ) ) ;
#18482 = ORIENTED_EDGE ( 'NONE', *, *, #440, .F. ) ;
#18483 = CARTESIAN_POINT ( 'NONE',  ( 99.99999999999995737, 85.00000000000000000, -1.387778780781445676E-14 ) ) ;
#18484 = CARTESIAN_POINT ( 'NONE',  ( -13.14518615778179544, 32.81445312608393294, 0.000000000000000000 ) ) ;
#18485 = CARTESIAN_POINT ( 'NONE',  ( -13.57481594606304576, 34.79882812716787299, 5.622872871577880183 ) ) ;
#18486 = CARTESIAN_POINT ( 'NONE',  ( 97.92893218813451028, -4.999999999999989342, 5.312500002731184168 ) ) ;
#18487 = CARTESIAN_POINT ( 'NONE',  ( 116.8548138422182063, 38.32109375108394289, -5.444914386472297529 ) ) ;
#18488 = CARTESIAN_POINT ( 'NONE',  ( 78.57481594606304043, 32.02070312716787015, -5.622872871577873077 ) ) ;
#18489 = ORIENTED_EDGE ( 'NONE', *, *, #27805, .T. ) ;
#18490 = EDGE_CURVE ( 'NONE', #15725, #5426, #5782, .T. ) ;
#18491 = CARTESIAN_POINT ( 'NONE',  ( 104.9999999999999716, 1.449011120738813565E-14, 13.50000000000000000 ) ) ;
#18492 = CARTESIAN_POINT ( 'NONE',  ( 5.444914386472297529, 39.51171875108392584, -13.14518615778179900 ) ) ;
#18493 = CARTESIAN_POINT ( 'NONE',  ( 9.295050272127046043, 33.31054687608394005, -9.295050272127046043 ) ) ;
#18494 = DIRECTION ( 'NONE',  ( -1.000000000000000000, 0.000000000000000000, 0.000000000000000000 ) ) ;
#18495 = CARTESIAN_POINT ( 'NONE',  ( 91.91746824999998466, 110.0000000000000000, -51.87499999726882294 ) ) ;
#18496 = PLANE ( 'NONE',  #3904 ) ;
#18497 = CARTESIAN_POINT ( 'NONE',  ( 65.00000000000000000, 36.00000000000000000, -11.57481594606305109 ) ) ;
#18498 = VECTOR ( 'NONE', #21279, 1000.000000000000000 ) ;
#18499 = DIRECTION ( 'NONE',  ( 0.000000000000000000, 1.000000000000000000, 0.000000000000000000 ) ) ;
#18500 = CARTESIAN_POINT ( 'NONE',  ( 92.99999999999998579, 107.7255621263696526, -52.90000000000001990 ) ) ;
#18501 = DIRECTION ( 'NONE',  ( -0.000000000000000000, 1.000000000000000000, -0.000000000000000000 ) ) ;
#18502 = CARTESIAN_POINT ( 'NONE',  ( 99.99999999999997158, 117.3602355696678643, -50.99999999453762456 ) ) ;
#18503 = DIRECTION ( 'NONE',  ( 0.000000000000000000, 0.000000000000000000, -1.000000000000000000 ) ) ;
#18504 = CARTESIAN_POINT ( 'NONE',  ( 9.598844408820456309, 35.14609374999999858, -9.598844408820458085 ) ) ;
#18505 = CARTESIAN_POINT ( 'NONE',  ( -13.14518615778179544, 34.40195312608393152, 0.000000000000000000 ) ) ;
#18506 = CARTESIAN_POINT ( 'NONE',  ( -13.14518615778179900, 32.56640625108394005, -5.444914386472297529 ) ) ;
#18507 = CARTESIAN_POINT ( 'NONE',  ( 5.444914386472302859, 35.24531250108393010, 13.14518615778179189 ) ) ;
#18508 = CARTESIAN_POINT ( 'NONE',  ( 5.622872871577878406, 35.79101562716787299, 13.57481594606304576 ) ) ;
#18509 = LINE ( 'NONE', #20083, #2660 ) ;
#18510 = CARTESIAN_POINT ( 'NONE',  ( 51.85481384221819923, 31.77265625108393365, -5.444914386472297529 ) ) ;
#18511 = DIRECTION ( 'NONE',  ( 5.782411586589357392E-17, 0.000000000000000000, 1.000000000000000000 ) ) ;
#18512 = CARTESIAN_POINT ( 'NONE',  ( 99.99999999999997158, 102.6397644303321215, -46.50000000000000711 ) ) ;
#18513 = VECTOR ( 'NONE', #628, 1000.000000000000000 ) ;
#18514 = EDGE_LOOP ( 'NONE', ( #6685, #13328, #14508, #10254 ) ) ;
#18515 = CYLINDRICAL_SURFACE ( 'NONE', #18908, 13.57481594606304576 ) ;
#18516 = CARTESIAN_POINT ( 'NONE',  ( -5.622872871577873077, 33.70742187500000142, -13.57481594606304753 ) ) ;
#18517 = CARTESIAN_POINT ( 'NONE',  ( 108.0825317500000011, 110.0000000000000000, -52.87499999726882294 ) ) ;
#18518 = CARTESIAN_POINT ( 'NONE',  ( 143.1451861577818079, 33.95546875108393436, 5.444914386472293977 ) ) ;
#18519 = ORIENTED_EDGE ( 'NONE', *, *, #17489, .T. ) ;
#18520 = CARTESIAN_POINT ( 'NONE',  ( 94.99999999999997158, 2.071067811865471953, 7.937500000000001776 ) ) ;
#18521 = CARTESIAN_POINT ( 'NONE',  ( 195.0000000000000000, 36.43593749999999432, 13.57481594606304576 ) ) ;
#18522 = CARTESIAN_POINT ( 'NONE',  ( 101.8468681455906903, 81.75000000136560629, 4.458734124999987891 ) ) ;
#18523 = AXIS2_PLACEMENT_3D ( 'NONE', #21356, #10216, #6375 ) ;
#18524 = CARTESIAN_POINT ( 'NONE',  ( 103.5355339059327235, 90.87500000000000000, 3.535533905932724874 ) ) ;
#18525 = CARTESIAN_POINT ( 'NONE',  ( 116.4251840539369596, 38.61874999999999147, 0.000000000000000000 ) ) ;
#18526 = CARTESIAN_POINT ( 'NONE',  ( 93.46109445667489979, 114.7507929638356785, -47.82499999726882578 ) ) ;
#18527 = CARTESIAN_POINT ( 'NONE',  ( 208.1451861577817795, 39.51171875108392584, 5.444914386472293977 ) ) ;
#18528 = CARTESIAN_POINT ( 'NONE',  ( 13.57481594606304931, 39.06523437716786873, 5.622872871577869525 ) ) ;
#18529 = VERTEX_POINT ( 'NONE', #19829 ) ;
#18530 = CARTESIAN_POINT ( 'NONE',  ( 104.9999999999999574, -2.071067811865462627, 7.437500000000000000 ) ) ;
#18531 = ORIENTED_EDGE ( 'NONE', *, *, #8798, .F. ) ;
#18532 = CARTESIAN_POINT ( 'NONE',  ( -5.444914386472297529, 31.87187500108393223, -13.14518615778179900 ) ) ;
#18533 = CARTESIAN_POINT ( 'NONE',  ( 189.3771271284221314, 32.51679687716787726, 13.57481594606304753 ) ) ;
#18534 = AXIS2_PLACEMENT_3D ( 'NONE', #25673, #12824, #12541 ) ;
#18535 = CARTESIAN_POINT ( 'NONE',  ( 9.598844408820459861, 35.84062500216786873, 9.598844408820456309 ) ) ;
#18536 = CARTESIAN_POINT ( 'NONE',  ( 104.9999999999999716, 1.449011120738813565E-14, 13.62500000273118417 ) ) ;
#18537 = DIRECTION ( 'NONE',  ( -0.000000000000000000, -0.000000000000000000, -1.000000000000000000 ) ) ;
#18538 = CARTESIAN_POINT ( 'NONE',  ( 97.92893218813445344, 80.31250000273119838, 4.999999999999948486 ) ) ;
#18539 = CARTESIAN_POINT ( 'NONE',  ( 103.5355339059327093, 3.535533905932755072, 11.75000000273118594 ) ) ;
#18540 = CARTESIAN_POINT ( 'NONE',  ( 74.59884440882045453, 32.56640625000000000, 9.598844408820456309 ) ) ;
#18541 = CARTESIAN_POINT ( 'NONE',  ( 100.8561741729129295, 123.4000000010924794, 2.066987299999979211 ) ) ;
#18542 = CARTESIAN_POINT ( 'NONE',  ( 195.0000000000000000, 0.000000000000000000, 0.000000000000000000 ) ) ;
#18543 = CARTESIAN_POINT ( 'NONE',  ( 116.9416181435491211, 36.00000000000000711, 1.569311539113940501 ) ) ;
#18544 = CARTESIAN_POINT ( 'NONE',  ( 104.4587341249999781, 1.846868145590750299, 6.250000001365592084 ) ) ;
#18545 = DIRECTION ( 'NONE',  ( 0.000000000000000000, 1.000000000000000000, 0.000000000000000000 ) ) ;
#18546 = CARTESIAN_POINT ( 'NONE',  ( 96.84719886470459471, -3.152801135295355994, 10.56250000136559208 ) ) ;
#18547 = CARTESIAN_POINT ( 'NONE',  ( 95.67376207875072680, 115.9545556584642867, -46.80000000546237970 ) ) ;
#18548 = CARTESIAN_POINT ( 'NONE',  ( 101.8468681455907330, 94.37499999863440792, 4.458734124999979898 ) ) ;
#18549 = FACE_BOUND ( 'NONE', #4890, .T. ) ;
#18550 = CARTESIAN_POINT ( 'NONE',  ( 108.0825317500000011, 110.0000000000000000, -54.62499999726882294 ) ) ;
#18551 = CARTESIAN_POINT ( 'NONE',  ( -5.444914386472297529, 34.25312500108393010, -13.14518615778179900 ) ) ;
#18552 = ORIENTED_EDGE ( 'NONE', *, *, #5869, .F. ) ;
#18553 = DIRECTION ( 'NONE',  ( -0.000000000000000000, 1.000000000000000000, -0.000000000000000000 ) ) ;
#18554 = EDGE_CURVE ( 'NONE', #12423, #27263, #8855, .T. ) ;
#18555 = AXIS2_PLACEMENT_3D ( 'NONE', #15022, #23742, #8065 ) ;
#18556 = CARTESIAN_POINT ( 'NONE',  ( -5.622872871577873966, 37.67617187499999432, -13.57481594606304753 ) ) ;
#18557 = CARTESIAN_POINT ( 'NONE',  ( 208.1451861577818079, 33.01289062608393010, -1.609821015232357215E-15 ) ) ;
#18558 = EDGE_LOOP ( 'NONE', ( #24091, #20193, #17722, #28132 ) ) ;
#18559 =( BOUNDED_CURVE ( )  B_SPLINE_CURVE ( 2, ( #22091, #14085, #20525, #22945, #22805, #3273, #3406, #11942, #7246 ),
 .UNSPECIFIED., .F., .F. ) 
 B_SPLINE_CURVE_WITH_KNOTS ( ( 3, 2, 2, 2, 3 ),
 ( 0.3541666666666666852, 0.3645833333333332593, 0.3749999999999998890, 0.3854166666666665741, 0.3958333333333331483 ),
 .UNSPECIFIED. ) 
 CURVE ( )  GEOMETRIC_REPRESENTATION_ITEM ( )  RATIONAL_B_SPLINE_CURVE ( ( 1.000000000000000000, 0.9238795325112867385, 1.000000000000000000, 0.9238795325112867385, 1.000000000000000000, 0.9238795325112867385, 1.000000000000000000, 0.9238795325112879597, 0.9999999999999987788 ) ) 
 REPRESENTATION_ITEM ( '' )  );
#18560 = EDGE_CURVE ( 'NONE', #7349, #9247, #8712, .T. ) ;
#18561 = CARTESIAN_POINT ( 'NONE',  ( 197.1699565831061420, 49.99999999883939950, -13.43548448457871558 ) ) ;
#18562 = CARTESIAN_POINT ( 'NONE',  ( 95.54126587499996504, 1.387778780781445676E-14, 6.687500001365592084 ) ) ;
#18563 = ADVANCED_FACE ( 'NONE', ( #2317 ), #6295, .T. ) ;
#18564 = ORIENTED_EDGE ( 'NONE', *, *, #16100, .F. ) ;
#18565 = CARTESIAN_POINT ( 'NONE',  ( 102.4976396683250925, 102.3130555110000159, -46.77500000273119696 ) ) ;
#18566 = CARTESIAN_POINT ( 'NONE',  ( 9.295050272127046043, 35.49335937608393010, -9.295050272127046043 ) ) ;
#18567 = CARTESIAN_POINT ( 'NONE',  ( 185.4011555911795313, 40.20625000216787726, -9.598844408820458085 ) ) ;
#18568 = DIRECTION ( 'NONE',  ( 0.000000000000000000, 0.000000000000000000, 1.000000000000000000 ) ) ;
#18569 = ADVANCED_FACE ( 'NONE', ( #10974 ), #4168, .F. ) ;
#18570 = CARTESIAN_POINT ( 'NONE',  ( 5.444914386472302859, 36.23750000108393721, 13.14518615778179189 ) ) ;
#18571 = CARTESIAN_POINT ( 'NONE',  ( 5.444914386472297529, 33.16171875108393152, -13.14518615778179900 ) ) ;
#18572 = CARTESIAN_POINT ( 'NONE',  ( 104.4587341249999923, 91.49999999863440792, 1.846868145590726318 ) ) ;
#18573 = DIRECTION ( 'NONE',  ( 1.000000000000000000, -0.000000000000000000, -5.782411586589357392E-17 ) ) ;
#18574 = EDGE_CURVE ( 'NONE', #15719, #25242, #21712, .T. ) ;
#18575 = CARTESIAN_POINT ( 'NONE',  ( -5.622872871577965448, 37.27929687716785878, 13.57481594606295161 ) ) ;
#18576 = CARTESIAN_POINT ( 'NONE',  ( -5.444914386472297529, 33.45937500108394147, -13.14518615778179900 ) ) ;
#18577 = CARTESIAN_POINT ( 'NONE',  ( 98.15313185440923860, -4.458734124999987891, 7.875000001365592084 ) ) ;
#18578 = CARTESIAN_POINT ( 'NONE',  ( 103.1528011352953342, 84.06250000136560629, 3.152801135295355106 ) ) ;
#18579 = CARTESIAN_POINT ( 'NONE',  ( 99.99999999999998579, 138.0000000000000000, -11.50000000000002309 ) ) ;
#18580 = VERTEX_POINT ( 'NONE', #28109 ) ;
#18581 = CARTESIAN_POINT ( 'NONE',  ( 13.14518615778179722, 34.84843750108393579, -5.444914386472297529 ) ) ;
#18582 = CARTESIAN_POINT ( 'NONE',  ( 97.50000000000000000, 122.6500000021849530, -1.035533905932742416 ) ) ;
#18583 = CARTESIAN_POINT ( 'NONE',  ( 103.1528011352953484, 92.68749999863440792, -3.152801135295366208 ) ) ;
#18584 = DIRECTION ( 'NONE',  ( 1.000000000000000000, 0.000000000000000000, 0.000000000000000000 ) ) ;
#18585 = CARTESIAN_POINT ( 'NONE',  ( 102.4976396683250783, 102.3130555110000159, -47.27499999726882152 ) ) ;
#18586 = EDGE_CURVE ( 'NONE', #18339, #20261, #9156, .T. ) ;
#18587 = CARTESIAN_POINT ( 'NONE',  ( 95.00000000000000000, 93.56250000000000000, 2.071067811865463959 ) ) ;
#18588 = CARTESIAN_POINT ( 'NONE',  ( -13.57481594606304398, 33.11210937499999574, 5.622872871577880183 ) ) ;
#18589 = VERTEX_POINT ( 'NONE', #26249 ) ;
#18590 = CARTESIAN_POINT ( 'NONE',  ( 195.0000000000000000, 37.32890625216786873, 13.57481594606304576 ) ) ;
#18591 = CARTESIAN_POINT ( 'NONE',  ( 74.29505027212704249, 37.87460937608393863, 9.295050272127046043 ) ) ;
#18592 = DIRECTION ( 'NONE',  ( -0.000000000000000000, 1.000000000000000000, -0.000000000000000000 ) ) ;
#18593 = AXIS2_PLACEMENT_3D ( 'NONE', #24494, #4839, #7233 ) ;
#18594 = CARTESIAN_POINT ( 'NONE',  ( 198.7556399192858976, 31.78804746655075419, -13.14518615778179544 ) ) ;
#18595 = VERTEX_POINT ( 'NONE', #6709 ) ;
#18596 = DIRECTION ( 'NONE',  ( -0.000000000000000000, -0.000000000000000000, -1.000000000000000000 ) ) ;
#18597 = EDGE_CURVE ( 'NONE', #3340, #3050, #1198, .T. ) ;
#18598 = CARTESIAN_POINT ( 'NONE',  ( 3.114697745540293106, 53.90847045361019241, -15.00000000000000000 ) ) ;
#18599 = PRESENTATION_LAYER_ASSIGNMENT (  '', '', ( #24512 ) ) ;
#18600 = CARTESIAN_POINT ( 'NONE',  ( 202.6165253254807794, 54.91574374957784954, 14.99999999999994493 ) ) ;
#18601 = ADVANCED_FACE ( 'NONE', ( #21697 ), #24108, .F. ) ;
#18602 = CARTESIAN_POINT ( 'NONE',  ( 116.4251840539369596, 36.38632812716788578, 5.622872871577880183 ) ) ;
#18603 =( BOUNDED_CURVE ( )  B_SPLINE_CURVE ( 2, ( #3073, #944, #11738, #16594, #14444, #3350, #1640, #8179, #20744 ),
 .UNSPECIFIED., .F., .F. ) 
 B_SPLINE_CURVE_WITH_KNOTS ( ( 3, 2, 2, 2, 3 ),
 ( 0.8541666666666670737, 0.8645833333333337034, 0.8750000000000003331, 0.8854166666666669627, 0.8958333333333335924 ),
 .UNSPECIFIED. ) 
 CURVE ( )  GEOMETRIC_REPRESENTATION_ITEM ( )  RATIONAL_B_SPLINE_CURVE ( ( 0.9999999999999967804, 0.9238795325112899581, 1.000000000000000000, 0.9238795325112867385, 1.000000000000000000, 0.9238795325112867385, 1.000000000000000000, 0.9238795325112850731, 1.000000000000001554 ) ) 
 REPRESENTATION_ITEM ( '' )  );
#18604 = DIRECTION ( 'NONE',  ( 0.000000000000000000, 1.000000000000000000, 0.000000000000000000 ) ) ;
#18605 = CARTESIAN_POINT ( 'NONE',  ( 208.1451861577818079, 37.18007812608393436, -1.609821015232357215E-15 ) ) ;
#18606 = ORIENTED_EDGE ( 'NONE', *, *, #5162, .F. ) ;
#18607 = CARTESIAN_POINT ( 'NONE',  ( 103.1528011352953342, 3.152801135295383084, 2.062500001365591640 ) ) ;
#18608 = CARTESIAN_POINT ( 'NONE',  ( 2.493653234604083739E-15, 35.74140625216787015, 13.57481594606304576 ) ) ;
#18609 = CARTESIAN_POINT ( 'NONE',  ( 103.5355339059327235, 90.87500000000000000, 3.535533905932724874 ) ) ;
#18610 = AXIS2_PLACEMENT_3D ( 'NONE', #13750, #2804, #22475 ) ;
#18611 = CARTESIAN_POINT ( 'NONE',  ( 99.99999999999995737, 83.68750000136560629, 4.458734124999988779 ) ) ;
#18612 = DIRECTION ( 'NONE',  ( -1.000000000000000000, -0.000000000000000000, -0.000000000000000000 ) ) ;
#18613 = CARTESIAN_POINT ( 'NONE',  ( -13.14518615778179189, 40.00781250108393294, 5.444914386472304635 ) ) ;
#18614 = CARTESIAN_POINT ( 'NONE',  ( -9.598844408820454532, 38.71796874999999716, 9.598844408820459861 ) ) ;
#18615 = VECTOR ( 'NONE', #20956, 1000.000000000000000 ) ;
#18616 = CARTESIAN_POINT ( 'NONE',  ( 0.000000000000000000, 21.95886589889650509, 0.000000000000000000 ) ) ;
#18617 = CARTESIAN_POINT ( 'NONE',  ( 104.9999999999999716, 93.81249999726880162, 2.071067811865467956 ) ) ;
#18618 = CARTESIAN_POINT ( 'NONE',  ( 130.0000000000000000, 34.45156249999999432, -13.57481594606304576 ) ) ;
#18619 = ORIENTED_EDGE ( 'NONE', *, *, #16850, .T. ) ;
#18620 = ORIENTED_EDGE ( 'NONE', *, *, #10798, .F. ) ;
#18621 = CARTESIAN_POINT ( 'NONE',  ( 92.99999999999998579, 110.0000000000000000, -55.00000000000002132 ) ) ;
#18622 = CARTESIAN_POINT ( 'NONE',  ( 13.14518615778179900, 34.74921875108395142, 5.444914386472293977 ) ) ;
#18623 = CARTESIAN_POINT ( 'NONE',  ( 13.57481594606304576, 35.14609375216787157, -1.662435489736055892E-15 ) ) ;
#18624 = APPLICATION_CONTEXT ( 'automotive_design' ) ;
#18625 = CARTESIAN_POINT ( 'NONE',  ( 103.5355339059327093, -3.535533905932726206, 5.500000002731185056 ) ) ;
#18626 = CARTESIAN_POINT ( 'NONE',  ( 143.1451861577818079, 40.30546875108393579, 5.444914386472293977 ) ) ;
#18627 = CARTESIAN_POINT ( 'NONE',  ( 51.85481384221819923, 39.71015625108393010, -5.444914386472297529 ) ) ;
#18628 = EDGE_CURVE ( 'NONE', #26813, #7460, #7973, .T. ) ;
#18629 = CARTESIAN_POINT ( 'NONE',  ( 59.43094144809686696, 36.00000000000000000, 11.91493531101255954 ) ) ;
#18630 = CARTESIAN_POINT ( 'NONE',  ( -5.444914386472299306, 38.32109375108394289, 13.14518615778179722 ) ) ;
#18631 = CARTESIAN_POINT ( 'NONE',  ( -5.444914386472297529, 32.66562500108393863, -13.14518615778179722 ) ) ;
#18632 = CARTESIAN_POINT ( 'NONE',  ( 105.6631189606246295, 114.1144967660473242, -48.80000000000001137 ) ) ;
#18633 = CARTESIAN_POINT ( 'NONE',  ( 102.4976396683250783, 102.3130555110000159, -53.27499999726882862 ) ) ;
#18634 = CARTESIAN_POINT ( 'NONE',  ( -5.622872871577873966, 33.70742187499999432, -13.57481594606304753 ) ) ;
#18635 = CARTESIAN_POINT ( 'NONE',  ( 99.99999999999995737, 82.87500000273119838, -5.000000000000018652 ) ) ;
#18636 = CARTESIAN_POINT ( 'NONE',  ( 97.50000000000000000, 124.2000000000000028, -9.540979117872439019E-15 ) ) ;
#18637 = CARTESIAN_POINT ( 'NONE',  ( 102.4999999999999858, 122.9906688167216373, 0.1932551333443592867 ) ) ;
#18638 = CARTESIAN_POINT ( 'NONE',  ( 102.0669872999999797, 124.3500000010924822, -9.794112055954760458E-15 ) ) ;
#18639 = CARTESIAN_POINT ( 'NONE',  ( 130.3745404134768648, 36.00000000000000000, -13.51869779562199447 ) ) ;
#18640 = CARTESIAN_POINT ( 'NONE',  ( 195.0000000000000000, 39.71015625216787015, 13.57481594606304576 ) ) ;
#18641 = CARTESIAN_POINT ( 'NONE',  ( 98.15313185440925281, 4.458734125000016313, 13.25000000136559208 ) ) ;
#18642 = CARTESIAN_POINT ( 'NONE',  ( 9.598844408820456309, 34.35234374999999574, -9.598844408820458085 ) ) ;
#18643 = EDGE_LOOP ( 'NONE', ( #26442, #27141 ) ) ;
#18644 = CARTESIAN_POINT ( 'NONE',  ( -9.078091922698781957, 36.00000000000000711, -9.794392408849049048 ) ) ;
#18645 = CARTESIAN_POINT ( 'NONE',  ( -5.622872871577873077, 40.35507812499998437, 13.57481594606304753 ) ) ;
#18646 = CARTESIAN_POINT ( 'NONE',  ( -5.444914386472297529, 31.67343750108393863, -13.14518615778179900 ) ) ;
#18647 = CARTESIAN_POINT ( 'NONE',  ( -9.295050272127044266, 35.89023437608393152, 9.295050272127047819 ) ) ;
#18648 = CARTESIAN_POINT ( 'NONE',  ( 5.622872871577878406, 34.20351562716788862, 13.57481594606304576 ) ) ;
#18649 = LINE ( 'NONE', #7812, #17206 ) ;
#18650 = CARTESIAN_POINT ( 'NONE',  ( 95.54126587499995082, 82.50000000136560629, 1.846868145590724986 ) ) ;
#18651 = CARTESIAN_POINT ( 'NONE',  ( 51.85481384221819923, 40.70234375108393721, -5.444914386472297529 ) ) ;
#18652 = CARTESIAN_POINT ( 'NONE',  ( 99.99999999999998579, 118.4984768113314004, -45.87500000273118417 ) ) ;
#18653 = CARTESIAN_POINT ( 'NONE',  ( 2.493653234604083739E-15, 34.94765625216787441, 13.57481594606304576 ) ) ;
#18654 = ORIENTED_EDGE ( 'NONE', *, *, #12876, .T. ) ;
#18655 = CARTESIAN_POINT ( 'NONE',  ( 102.0669872999999797, 124.3500000010924822, -9.794112055954760458E-15 ) ) ;
#18656 = CARTESIAN_POINT ( 'NONE',  ( -15.00000000000000355, 75.00000000000000000, -14.99999999999999822 ) ) ;
#18657 = CARTESIAN_POINT ( 'NONE',  ( 104.3262379212492448, 115.9545556584642867, -47.19999999453762740 ) ) ;
#18658 = CARTESIAN_POINT ( 'NONE',  ( 139.2950502721270425, 35.49335937608393721, 9.295050272127046043 ) ) ;
#18659 = ORIENTED_EDGE ( 'NONE', *, *, #1180, .F. ) ;
#18660 = CARTESIAN_POINT ( 'NONE',  ( 2.493653234604083739E-15, 38.91640625216786731, 13.57481594606304576 ) ) ;
#18661 = CARTESIAN_POINT ( 'NONE',  ( 70.62287287157793969, 38.46992187716787726, -13.57481594606299247 ) ) ;
#18662 = CARTESIAN_POINT ( 'NONE',  ( 101.8468681455906903, 83.75000000136560629, 4.458734124999987891 ) ) ;
#18663 = CARTESIAN_POINT ( 'NONE',  ( 130.0000000000000000, 38.76757812608393294, -13.14518615778179544 ) ) ;
#18664 = PRESENTATION_LAYER_ASSIGNMENT (  '', '', ( #11342 ) ) ;
#18665 = CARTESIAN_POINT ( 'NONE',  ( 208.5748159460630688, 37.47773437500001137, -5.622872871577873966 ) ) ;
#18666 = CARTESIAN_POINT ( 'NONE',  ( 106.5389055433250860, 114.7507929638356785, -52.42499999726882010 ) ) ;
#18667 = CARTESIAN_POINT ( 'NONE',  ( -13.57481594606304753, 37.87460937716787868, -5.622872871577873077 ) ) ;
#18668 = VERTEX_POINT ( 'NONE', #11830 ) ;
#18669 = CIRCLE ( 'NONE', #24580, 13.57481594606304398 ) ;
#18670 = CARTESIAN_POINT ( 'NONE',  ( 104.9999999999999574, -2.071067811865462627, 9.437500000000000000 ) ) ;
#18671 = ORIENTED_EDGE ( 'NONE', *, *, #6192, .F. ) ;
#18672 = CARTESIAN_POINT ( 'NONE',  ( 12.07727640983618400, 35.99999999999999289, -6.197985357348143154 ) ) ;
#18673 = CARTESIAN_POINT ( 'NONE',  ( 181.4251840539369596, 31.57421875216786944, 0.000000000000000000 ) ) ;
#18674 = CARTESIAN_POINT ( 'NONE',  ( 107.5412658750000077, 110.0000000000000000, -53.81250000409679046 ) ) ;
#18675 = CARTESIAN_POINT ( 'NONE',  ( 96.46446609406721961, 3.535533905932755072, 1.000000002731185944 ) ) ;
#18676 = CARTESIAN_POINT ( 'NONE',  ( 139.2950502721270425, 38.66835937608393436, -9.295050272127046043 ) ) ;
#18677 = CARTESIAN_POINT ( 'NONE',  ( 99.99999999999995737, 80.37500000273119838, 4.999999999999990230 ) ) ;
#18678 = LINE ( 'NONE', #12228, #19977 ) ;
#18679 = CARTESIAN_POINT ( 'NONE',  ( 98.15313185440923860, 93.99999999863439371, 4.458734124999980786 ) ) ;
#18680 = CARTESIAN_POINT ( 'NONE',  ( 97.93301269999999192, 124.0000000010924879, 0.8561741729129329626 ) ) ;
#18681 = CARTESIAN_POINT ( 'NONE',  ( 181.4251840539369596, 40.99999999999999289, 0.000000000000000000 ) ) ;
#18682 = DIRECTION ( 'NONE',  ( -1.000000000000000000, 0.000000000000000000, 0.000000000000000000 ) ) ;
#18683 = CARTESIAN_POINT ( 'NONE',  ( 96.84719886470459471, 3.152801135295383084, 8.562500001365592084 ) ) ;
#18684 = ADVANCED_FACE ( 'NONE', ( #314 ), #20121, .F. ) ;
#18685 = CARTESIAN_POINT ( 'NONE',  ( 104.4587341249999781, -1.846868145590721655, 9.875000001365593860 ) ) ;
#18686 = CARTESIAN_POINT ( 'NONE',  ( 94.33688103937537051, 105.8855032339526758, -48.30000000546237970 ) ) ;
#18687 = CARTESIAN_POINT ( 'NONE',  ( 98.15313185440925281, 92.87499999863440792, -4.458734124999994997 ) ) ;
#18688 = CARTESIAN_POINT ( 'NONE',  ( 74.18017581364799184, 55.00000000000000000, -14.99999999999999822 ) ) ;
#18689 = CARTESIAN_POINT ( 'NONE',  ( 102.4999999999999858, 122.9375000002731184, -9.847140817659276890E-15 ) ) ;
#18690 = CARTESIAN_POINT ( 'NONE',  ( -8.049105076161786076E-16, 32.61601562608393579, -13.14518615778179544 ) ) ;
#18691 = ORIENTED_EDGE ( 'NONE', *, *, #17865, .T. ) ;
#18692 = CARTESIAN_POINT ( 'NONE',  ( 98.15313185440925281, 81.87500000136559208, 4.458734124999987891 ) ) ;
#18693 = CARTESIAN_POINT ( 'NONE',  ( 95.54126587499999346, 90.87499999863439371, 1.846868145590722543 ) ) ;
#18694 = CARTESIAN_POINT ( 'NONE',  ( 208.1451861577817795, 33.85625000108393579, -5.444914386472297529 ) ) ;
#18695 = EDGE_LOOP ( 'NONE', ( #974, #19924, #27770, #5728 ) ) ;
#18696 = CARTESIAN_POINT ( 'NONE',  ( 191.0201855541805855, 50.00000000123257848, -13.01613927312581787 ) ) ;
#18697 = CARTESIAN_POINT ( 'NONE',  ( 101.8468681455906903, 4.458734125000016313, 6.375000001365592084 ) ) ;
#18698 = ORIENTED_EDGE ( 'NONE', *, *, #19400, .F. ) ;
#18699 = CARTESIAN_POINT ( 'NONE',  ( 91.91746824999998466, 107.3738262389971538, -47.27500000273118275 ) ) ;
#18700 = CARTESIAN_POINT ( 'NONE',  ( 2.414731522848535132E-15, 32.02070312608393010, 13.14518615778179544 ) ) ;
#18701 = CARTESIAN_POINT ( 'NONE',  ( 189.3771271284221598, 38.56914062716787583, -13.57481594606310260 ) ) ;
#18702 = CARTESIAN_POINT ( 'NONE',  ( 13.14518615778179722, 39.31328125108392868, 5.444914386472293977 ) ) ;
#18703 = CARTESIAN_POINT ( 'NONE',  ( -8.049105076161786076E-16, 37.37851562608393863, -13.14518615778179544 ) ) ;
#18704 = CARTESIAN_POINT ( 'NONE',  ( -9.295050272127046043, 33.31054687608393294, -9.295050272127046043 ) ) ;
#18705 = CARTESIAN_POINT ( 'NONE',  ( 98.15313185440925281, 92.24999999863439371, 4.458734124999979898 ) ) ;
#18706 = DIRECTION ( 'NONE',  ( 0.000000000000000000, -0.8660254037844380415, 0.5000000000000009992 ) ) ;
#18707 = CARTESIAN_POINT ( 'NONE',  ( -5.622872871577873966, 36.98164062716787015, -13.57481594606304753 ) ) ;
#18708 = CARTESIAN_POINT ( 'NONE',  ( 3.755639919285892248, 31.78804746655075419, -13.14518615778179544 ) ) ;
#18709 = CARTESIAN_POINT ( 'NONE',  ( 95.54126587499996504, 1.387778780781445676E-14, 1.687500001365591418 ) ) ;
#18710 =( BOUNDED_CURVE ( )  B_SPLINE_CURVE ( 2, ( #2453, #6568, #23826, #26248, #23968, #22117, #13100, #21696, #2597 ),
 .UNSPECIFIED., .F., .T. ) 
 B_SPLINE_CURVE_WITH_KNOTS ( ( 3, 2, 2, 2, 3 ),
 ( 0.4166666666666667407, 0.4583333333333334259, 0.5000000000000002220, 0.5416666666666668517, 0.5833333333333337034 ),
 .UNSPECIFIED. ) 
 CURVE ( )  GEOMETRIC_REPRESENTATION_ITEM ( )  RATIONAL_B_SPLINE_CURVE ( ( 0.9999999999999998890, 0.9238795325112868495, 1.000000000000000000, 0.9238795325112867385, 1.000000000000000000, 0.9238795325112867385, 1.000000000000000000, 0.9238795325112861834, 1.000000000000000666 ) ) 
 REPRESENTATION_ITEM ( '' )  );
#18711 = EDGE_CURVE ( 'NONE', #24077, #19327, #7542, .T. ) ;
#18712 = CARTESIAN_POINT ( 'NONE',  ( 99.99999999999995737, 82.93750000136560629, 4.458734124999988779 ) ) ;
#18713 = CARTESIAN_POINT ( 'NONE',  ( 13.14518615778179900, 35.34453125108392868, 5.444914386472293977 ) ) ;
#18714 = CARTESIAN_POINT ( 'NONE',  ( 2.493653234604083739E-15, 32.46718749999999432, 13.57481594606304576 ) ) ;
#18715 = AXIS2_PLACEMENT_3D ( 'NONE', #27426, #16584, #25277 ) ;
#18716 = CARTESIAN_POINT ( 'NONE',  ( 65.71976059610913978, 53.51499872091922327, 14.99999999999997513 ) ) ;
#18717 = ORIENTED_EDGE ( 'NONE', *, *, #10096, .F. ) ;
#18718 = EDGE_CURVE ( 'NONE', #20101, #923, #19377, .T. ) ;
#18719 = CARTESIAN_POINT ( 'NONE',  ( 2.414731522848535132E-15, 32.21914062608393436, 13.14518615778179544 ) ) ;
#18720 = CARTESIAN_POINT ( 'NONE',  ( 99.99999999999998579, 123.9500000010924765, 2.066987299999980099 ) ) ;
#18721 = CARTESIAN_POINT ( 'NONE',  ( 103.1528011352953484, 93.43749999863440792, 3.152801135295352886 ) ) ;
#18722 = CARTESIAN_POINT ( 'NONE',  ( 98.09035273295538104, 123.0000000000000142, 0.7910017786517971050 ) ) ;
#18723 = CARTESIAN_POINT ( 'NONE',  ( 102.4976396683250783, 102.3130555110000159, -55.27499999726882152 ) ) ;
#18724 = CARTESIAN_POINT ( 'NONE',  ( 124.3771271284220745, 39.36289062716787157, -13.57481594606297293 ) ) ;
#18725 = CARTESIAN_POINT ( 'NONE',  ( 13.14518615778179544, 32.21914062608393436, -1.609821015232357215E-15 ) ) ;
#18726 = VERTEX_POINT ( 'NONE', #11259 ) ;
#18727 = CARTESIAN_POINT ( 'NONE',  ( 70.44491438647229131, 37.03125000108393294, 13.14518615778179189 ) ) ;
#18728 = CYLINDRICAL_SURFACE ( 'NONE', #18715, 12.50000000000001599 ) ;
#18729 = ADVANCED_FACE ( 'NONE', ( #893 ), #11683, .T. ) ;
#18730 = CARTESIAN_POINT ( 'NONE',  ( 94.99999999999995737, 85.00000000000000000, -1.387778780781445676E-14 ) ) ;
#18731 = ORIENTED_EDGE ( 'NONE', *, *, #28113, .T. ) ;
#18732 = DIRECTION ( 'NONE',  ( -2.674902700537828060E-32, 1.000000000000000000, -4.625929269271485914E-16 ) ) ;
#18733 = CYLINDRICAL_SURFACE ( 'NONE', #15394, 7.000000000000006217 ) ;
#18734 = CARTESIAN_POINT ( 'NONE',  ( 135.6228728715778686, 36.88242187716787157, -13.57481594606304753 ) ) ;
#18735 = CARTESIAN_POINT ( 'NONE',  ( 139.5988444088204687, 37.42812500216787441, 9.598844408820456309 ) ) ;
#18736 = CYLINDRICAL_SURFACE ( 'NONE', #12831, 4.999999999999989342 ) ;
#18737 = CARTESIAN_POINT ( 'NONE',  ( 94.33688103937534208, 114.1144967660473242, -46.69999999453764161 ) ) ;
#18738 = PRODUCT_DEFINITION_SHAPE ( 'NONE', 'NONE',  #28211 ) ;
#18739 = CARTESIAN_POINT ( 'NONE',  ( 185.7049497278729575, 36.88242187608393152, 9.295050272127047819 ) ) ;
#18740 = ADVANCED_FACE ( 'NONE', ( #6851 ), #5019, .T. ) ;
#18741 = ORIENTED_EDGE ( 'NONE', *, *, #27102, .F. ) ;
#18742 = ORIENTED_EDGE ( 'NONE', *, *, #10555, .F. ) ;
#18743 = CARTESIAN_POINT ( 'NONE',  ( 104.4587341249999781, 1.846868145590750299, 1.000000001365592528 ) ) ;
#18744 = CARTESIAN_POINT ( 'NONE',  ( 116.6399989480775901, 40.87597656304196647, 0.000000000000000000 ) ) ;
#18745 = CARTESIAN_POINT ( 'NONE',  ( 13.57481594606304753, 33.60820312716787583, -5.622872871577873966 ) ) ;
#18746 = CARTESIAN_POINT ( 'NONE',  ( 96.84719886470459471, 83.31250000136560629, -3.152801135295383084 ) ) ;
#18747 = CARTESIAN_POINT ( 'NONE',  ( 99.99999999999998579, 128.0000000000000000, -5.204170427930421283E-15 ) ) ;
#18748 =( NAMED_UNIT ( * ) SI_UNIT ( $, .STERADIAN. ) SOLID_ANGLE_UNIT ( ) );
#18749 = CARTESIAN_POINT ( 'NONE',  ( 2.414731522848535132E-15, 39.36289062608393152, 13.14518615778179544 ) ) ;
#18750 = CARTESIAN_POINT ( 'NONE',  ( 94.99999999999995737, 81.06250000000001421, 2.071067811865466624 ) ) ;
#18751 = FACE_OUTER_BOUND ( 'NONE', #14553, .T. ) ;
#18752 = LINE ( 'NONE', #1650, #6310 ) ;
#18753 = CARTESIAN_POINT ( 'NONE',  ( 108.0825317499999869, 107.3738262389971538, -48.72499999726881015 ) ) ;
#18754 = ORIENTED_EDGE ( 'NONE', *, *, #17301, .T. ) ;
#18755 = EDGE_CURVE ( 'NONE', #13582, #7547, #6993, .T. ) ;
#18756 = EDGE_LOOP ( 'NONE', ( #5763, #4192, #12219, #20566 ) ) ;
#18757 = CARTESIAN_POINT ( 'NONE',  ( 9.598844408820456309, 39.90859374999999432, -9.598844408820458085 ) ) ;
#18758 = CARTESIAN_POINT ( 'NONE',  ( -5.444914386472299306, 39.90859375108393436, 13.14518615778179722 ) ) ;
#18759 = CARTESIAN_POINT ( 'NONE',  ( 102.0710678118654329, 5.000000000000018652, 5.812500002731185056 ) ) ;
#18760 = CARTESIAN_POINT ( 'NONE',  ( 130.0000000000000000, 40.55351562608393579, -13.14518615778179544 ) ) ;
#18761 = CARTESIAN_POINT ( 'NONE',  ( 74.29505027212704249, 37.08085937608393579, -9.295050272127046043 ) ) ;
#18762 =( BOUNDED_SURFACE ( )  B_SPLINE_SURFACE ( 3, 2, ( 
 ( #26756, #5228, #11471 ),
 ( #13893, #13611, #3089 ),
 ( #22619, #7198, #20333 ),
 ( #11756, #22188, #24464 ),
 ( #5372, #18041, #5513 ),
 ( #820, #7345, #675 ),
 ( #14039, #1103, #5088 ),
 ( #9488, #20481, #15758 ),
 ( #20618, #16036, #9770 ),
 ( #2939, #15893, #24748 ),
 ( #22334, #7489, #25030 ),
 ( #7637, #24610, #3227 ),
 ( #11610, #27042, #7061 ),
 ( #961, #20051, #16185 ),
 ( #9630, #16332, #24891 ),
 ( #11894, #2668, #18335 ),
 ( #17904, #11329, #529 ),
 ( #9210, #26614, #4947 ),
 ( #17013, #20756, #23036 ),
 ( #14180, #16466, #19017 ) ),
 .UNSPECIFIED., .F., .F., .F. ) 
 B_SPLINE_SURFACE_WITH_KNOTS ( ( 4, 2, 2, 2, 2, 2, 2, 2, 2, 4 ),
 ( 3, 3 ),
 ( 0.009073803551359458167, 0.01139250602759181441, 0.01371120850382416892, 0.01602991098005652343, 0.01834861345628887794, 0.01950796469440505693, 0.02066731593252123245, 0.02298601840875359043, 0.02530472088498594493, 0.02762342336121829944 ),
 ( 0.000000000000000000, 1.000000000000000000 ),
 .UNSPECIFIED. ) 
 GEOMETRIC_REPRESENTATION_ITEM ( )  RATIONAL_B_SPLINE_SURFACE ( (
 ( 1.000000000000000000, 0.7071067811865470176, 1.000000000000000000),
 ( 1.000000000000000000, 0.7344871497829198459, 1.000000000000000000),
 ( 1.000000000000000000, 0.7612510203318438862, 1.000000000000000000),
 ( 1.000000000000000000, 0.8116663633844432013, 1.000000000000000000),
 ( 1.000000000000000000, 0.8353358059752060694, 1.000000000000000000),
 ( 1.000000000000000000, 0.8764699612585808985, 1.000000000000000000),
 ( 1.000000000000000000, 0.8939017358719159034, 1.000000000000000000),
 ( 1.000000000000000000, 0.9185314935647115320, 1.000000000000000000),
 ( 1.000000000000000000, 0.9256439951239472386, 1.000000000000000000),
 ( 1.000000000000000000, 0.9261623622476506945, 1.000000000000000000),
 ( 1.000000000000000000, 0.9246301385979278642, 1.000000000000000000),
 ( 1.000000000000000000, 0.9183304321347580679, 1.000000000000000000),
 ( 1.000000000000000000, 0.9135987334168627072, 1.000000000000000000),
 ( 1.000000000000000000, 0.8954110486039240646, 1.000000000000000000),
 ( 1.000000000000000000, 0.8779877431164836432, 1.000000000000000000),
 ( 1.000000000000000000, 0.8366182664708666783, 1.000000000000000000),
 ( 1.000000000000000000, 0.8126941604017877685, 1.000000000000000000),
 ( 1.000000000000000000, 0.7617527316303357443, 1.000000000000000000),
 ( 1.000000000000000000, 0.7347103785793935860, 1.000000000000000000),
 ( 1.000000000000000000, 0.7071067811865462405, 1.000000000000000000) ) ) 
 REPRESENTATION_ITEM ( '' )  SURFACE ( )  );
#18763 = DIRECTION ( 'NONE',  ( 0.000000000000000000, 0.000000000000000000, -1.000000000000000000 ) ) ;
#18764 = CARTESIAN_POINT ( 'NONE',  ( 5.444914386472297529, 36.33671875108394289, -13.14518615778179900 ) ) ;
#18765 = LINE ( 'NONE', #18894, #13406 ) ;
#18766 = CYLINDRICAL_SURFACE ( 'NONE', #26718, 13.57481594606304576 ) ;
#18767 = CARTESIAN_POINT ( 'NONE',  ( 94.99999999999995737, 82.06250000000001421, 2.071067811865466624 ) ) ;
#18768 = CARTESIAN_POINT ( 'NONE',  ( 95.54126587499996504, 1.387778780781445676E-14, 14.56250000136559208 ) ) ;
#18769 = CYLINDRICAL_SURFACE ( 'NONE', #14941, 13.57481594606304576 ) ;
#18770 = CARTESIAN_POINT ( 'NONE',  ( 181.6399989480775901, 40.42949218912590936, 0.000000000000000000 ) ) ;
#18771 = CARTESIAN_POINT ( 'NONE',  ( 101.7677669529663547, 123.7069999999781515, 1.767766952966350891 ) ) ;
#18772 = CARTESIAN_POINT ( 'NONE',  ( 99.14382582708707048, 124.6000000010924822, -2.066987299999999195 ) ) ;
#18773 = CARTESIAN_POINT ( 'NONE',  ( 104.3262379212492448, 115.9545556584642867, -51.19999999453763451 ) ) ;
#18774 = CARTESIAN_POINT ( 'NONE',  ( -8.312177448680279460E-16, 32.16953125216787157, -13.57481594606304576 ) ) ;
#18775 = CARTESIAN_POINT ( 'NONE',  ( 104.4587341249999781, -1.846868145590721655, 13.87500000136559208 ) ) ;
#18776 = CARTESIAN_POINT ( 'NONE',  ( 99.99999999999998579, 102.6397644303321215, -48.00000000546237544 ) ) ;
#18777 = ORIENTED_EDGE ( 'NONE', *, *, #6047, .T. ) ;
#18778 = CYLINDRICAL_SURFACE ( 'NONE', #9333, 13.57481594606304398 ) ;
#18779 = CARTESIAN_POINT ( 'NONE',  ( -13.57481594606304576, 40.20624999999999005, 0.000000000000000000 ) ) ;
#18780 = CARTESIAN_POINT ( 'NONE',  ( 5.444914386472302859, 32.07031250108393294, 13.14518615778179189 ) ) ;
#18781 = CARTESIAN_POINT ( 'NONE',  ( -9.598844408820458085, 33.85625000216787583, -9.598844408820458085 ) ) ;
#18782 = CARTESIAN_POINT ( 'NONE',  ( 94.99999999999995737, 80.00000000000000000, -1.387778780781445676E-14 ) ) ;
#18783 = CARTESIAN_POINT ( 'NONE',  ( 104.4587341249999639, 80.93750000136559208, -1.442382525525748735E-14 ) ) ;
#18784 = CARTESIAN_POINT ( 'NONE',  ( 70.44491438647230552, 39.71015625108393010, -13.14518615778179900 ) ) ;
#18785 = CARTESIAN_POINT ( 'NONE',  ( 102.4976396683250925, 117.6869444889999841, -49.97500000273119269 ) ) ;
#18786 = CARTESIAN_POINT ( 'NONE',  ( -13.36000105192242060, 40.42949218912590936, 0.000000000000000000 ) ) ;
#18787 = CARTESIAN_POINT ( 'NONE',  ( 98.53841926354351699, 124.6500000010924651, -1.461580736456474794 ) ) ;
#18788 = DIRECTION ( 'NONE',  ( -0.000000000000000000, 1.000000000000000000, -0.000000000000000000 ) ) ;
#18789 = CARTESIAN_POINT ( 'NONE',  ( 94.33688103937534208, 114.1144967660473242, -48.69999999453764161 ) ) ;
#18790 = CARTESIAN_POINT ( 'NONE',  ( 124.5550856135277087, 33.45937500108394147, -13.14518615778179900 ) ) ;
#18791 = ORIENTED_EDGE ( 'NONE', *, *, #4266, .T. ) ;
#18792 = CARTESIAN_POINT ( 'NONE',  ( 102.1631189606246295, 103.3426043859339103, -51.89999999453764445 ) ) ;
#18793 = CARTESIAN_POINT ( 'NONE',  ( -9.295050272127046043, 40.65273437608393436, -9.295050272127046043 ) ) ;
#18794 = CARTESIAN_POINT ( 'NONE',  ( 5.622872871577871301, 39.26367187716787299, -13.57481594606304753 ) ) ;
#18795 = CARTESIAN_POINT ( 'NONE',  ( 139.2950502721270425, 38.46992187608393010, 9.295050272127046043 ) ) ;
#18796 = CARTESIAN_POINT ( 'NONE',  ( 70.62287287157788285, 37.37851562716787157, 13.57481594606304576 ) ) ;
#18797 = CARTESIAN_POINT ( 'NONE',  ( 0.000000000000000000, 21.36169591142201440, 23.85284712729792389 ) ) ;
#18798 = CARTESIAN_POINT ( 'NONE',  ( 13.57481594606304576, 39.11484375216787157, -1.662435489736055892E-15 ) ) ;
#18799 = ORIENTED_EDGE ( 'NONE', *, *, #18274, .T. ) ;
#18800 = AXIS2_PLACEMENT_3D ( 'NONE', #13997, #13570, #18005 ) ;
#18801 = CARTESIAN_POINT ( 'NONE',  ( 103.5355339059327093, 3.535533905932755072, 10.62499999999999822 ) ) ;
#18802 = VERTEX_POINT ( 'NONE', #15687 ) ;
#18803 = CARTESIAN_POINT ( 'NONE',  ( 13.14518615778179900, 34.05468750108394005, -5.444914386472297529 ) ) ;
#18804 = CARTESIAN_POINT ( 'NONE',  ( 208.5748159460630120, 32.71523437716787441, 5.622872871577869525 ) ) ;
#18805 = LINE ( 'NONE', #10092, #15565 ) ;
#18806 = CARTESIAN_POINT ( 'NONE',  ( 94.99999999999995737, 1.387778780781445676E-14, 12.12500000273118594 ) ) ;
#18807 = CARTESIAN_POINT ( 'NONE',  ( 143.1451861577818079, 39.36289062608393152, -1.609821015232357215E-15 ) ) ;
#18808 = CARTESIAN_POINT ( 'NONE',  ( 3.755639919285892248, 31.78804746655075419, -13.14518615778179544 ) ) ;
#18809 = CARTESIAN_POINT ( 'NONE',  ( 94.99999999999995737, 2.071067811865491493, 12.06250000273118950 ) ) ;
#18810 = CARTESIAN_POINT ( 'NONE',  ( 96.84719886470463734, 92.93749999863440792, 3.152801135295351997 ) ) ;
#18811 = CARTESIAN_POINT ( 'NONE',  ( 97.93301269999999192, 123.9000000010924794, -0.8561741729129505041 ) ) ;
#18812 = CARTESIAN_POINT ( 'NONE',  ( 189.3771271284221314, 37.97382812499999716, 13.57481594606304753 ) ) ;
#18813 = ITEM_DEFINED_TRANSFORMATION ( 'NONE', 'NONE', #13099,  #26844 ) ;
#18814 = CARTESIAN_POINT ( 'NONE',  ( 13.57481594606304753, 35.89023437499999858, -5.622872871577873966 ) ) ;
#18815 = CARTESIAN_POINT ( 'NONE',  ( 96.84719886470459471, 3.152801135295383084, 4.562500001365592084 ) ) ;
#18816 = CARTESIAN_POINT ( 'NONE',  ( 185.4011555911795313, 36.93203124999999432, -9.598844408820458085 ) ) ;
#18817 = CARTESIAN_POINT ( 'NONE',  ( 95.54126587499996504, 1.387778780781445676E-14, 6.437500001365592084 ) ) ;
#18818 = CARTESIAN_POINT ( 'NONE',  ( 93.00000000000001421, 112.2744378736303332, -50.60000000546236976 ) ) ;
#18819 = CARTESIAN_POINT ( 'NONE',  ( 96.84719886470463734, 95.18749999863440792, 3.152801135295351997 ) ) ;
#18820 = CARTESIAN_POINT ( 'NONE',  ( 208.5748159460630688, 39.75976562499999289, 5.622872871577868636 ) ) ;
#18821 = CARTESIAN_POINT ( 'NONE',  ( 1.137167824541903460, 36.00000000000000000, 13.09590655363594180 ) ) ;
#18822 = CARTESIAN_POINT ( 'NONE',  ( 13.57481594606304931, 40.55351562499998863, 5.622872871577869525 ) ) ;
#18823 = VERTEX_POINT ( 'NONE', #22263 ) ;
#18824 = CARTESIAN_POINT ( 'NONE',  ( 104.4587341249999781, 81.25000000136560629, -1.846868145590750299 ) ) ;
#18825 = DIRECTION ( 'NONE',  ( -0.000000000000000000, 1.000000000000000000, -0.000000000000000000 ) ) ;
#18826 = ORIENTED_EDGE ( 'NONE', *, *, #13303, .F. ) ;
#18827 = ORIENTED_EDGE ( 'NONE', *, *, #8942, .T. ) ;
#18828 = CARTESIAN_POINT ( 'NONE',  ( 196.9473259220809780, 51.47162402671693116, -15.00000000000000178 ) ) ;
#18829 = CARTESIAN_POINT ( 'NONE',  ( 101.8468681455906903, 4.458734125000016313, 7.375000001365592084 ) ) ;
#18830 = EDGE_CURVE ( 'NONE', #26423, #11228, #24389, .T. ) ;
#18831 = ORIENTED_EDGE ( 'NONE', *, *, #18939, .F. ) ;
#18832 = CARTESIAN_POINT ( 'NONE',  ( -8.312177448680279460E-16, 39.31328125216787583, -13.57481594606304576 ) ) ;
#18833 = CARTESIAN_POINT ( 'NONE',  ( -9.295050272127046043, 33.31054687608393294, -9.295050272127046043 ) ) ;
#18834 = CARTESIAN_POINT ( 'NONE',  ( 204.5988444088204403, 40.00781250216787299, -9.598844408820458085 ) ) ;
#18835 = CARTESIAN_POINT ( 'NONE',  ( 5.444914386472297529, 38.71796875108393721, -13.14518615778179722 ) ) ;
#18836 = CARTESIAN_POINT ( 'NONE',  ( 93.46109445667491400, 105.2492070361643215, -50.92500000273119554 ) ) ;
#18837 = CARTESIAN_POINT ( 'NONE',  ( 139.2950502721270425, 38.86679687608393863, -9.295050272127046043 ) ) ;
#18838 = CARTESIAN_POINT ( 'NONE',  ( -9.295050272127044266, 40.05742187608393579, 9.295050272127047819 ) ) ;
#18839 = ORIENTED_EDGE ( 'NONE', *, *, #7861, .T. ) ;
#18840 = CARTESIAN_POINT ( 'NONE',  ( 70.62287287157786864, 39.16445312499999432, -13.57481594606304753 ) ) ;
#18841 = CARTESIAN_POINT ( 'NONE',  ( 65.00000000000000000, 39.71015625216787015, 13.57481594606304576 ) ) ;
#18842 = PLANE ( 'NONE',  #23508 ) ;
#18843 = CARTESIAN_POINT ( 'NONE',  ( -13.14518615778179544, 32.02070312608393010, 0.000000000000000000 ) ) ;
#18844 = CARTESIAN_POINT ( 'NONE',  ( 101.8468681455907046, 4.458734125000016313, 1.375000001365592972 ) ) ;
#18845 = CARTESIAN_POINT ( 'NONE',  ( 104.4587341249999781, 82.12500000136560629, 1.846868145590721655 ) ) ;
#18846 = CARTESIAN_POINT ( 'NONE',  ( -13.14518615778179189, 34.25312500108393010, 5.444914386472304635 ) ) ;
#18847 = CARTESIAN_POINT ( 'NONE',  ( -13.14518615778179900, 39.90859375108394147, -5.444914386472297529 ) ) ;
#18848 = CARTESIAN_POINT ( 'NONE',  ( 63.39472812342341967, 53.60388944777321285, 14.99999999999998224 ) ) ;
#18849 = ORIENTED_EDGE ( 'NONE', *, *, #160, .T. ) ;
#18850 = CARTESIAN_POINT ( 'NONE',  ( -13.14518615778179544, 32.81445312608393294, 0.000000000000000000 ) ) ;
#18851 = FACE_OUTER_BOUND ( 'NONE', #23730, .T. ) ;
#18852 = CARTESIAN_POINT ( 'NONE',  ( 104.4587341249999781, 95.56249999863440792, -6.938893903907228378E-15 ) ) ;
#18853 = CARTESIAN_POINT ( 'NONE',  ( 92.99999999999998579, 110.0000000000000000, -145.0000000000000284 ) ) ;
#18854 = CARTESIAN_POINT ( 'NONE',  ( 102.4999999999999858, 123.0000000000000000, -8.724596124144689908E-15 ) ) ;
#18855 = CARTESIAN_POINT ( 'NONE',  ( -13.57481594606304398, 32.31835937499999289, 5.622872871577880183 ) ) ;
#18856 = EDGE_LOOP ( 'NONE', ( #17620, #23852, #11317, #4055, #18619, #24288, #21714, #27939, #25571, #27997, #27454, #6312, #27916, #15761, #4274, #10945, #28112 ) ) ;
#18857 = CARTESIAN_POINT ( 'NONE',  ( 51.85481384221821344, 37.62656250108393152, 5.444914386472304635 ) ) ;
#18858 = LINE ( 'NONE', #25423, #7790 ) ;
#18859 = DIRECTION ( 'NONE',  ( 1.000000000000000000, 0.000000000000000000, -0.000000000000000000 ) ) ;
#18860 = VERTEX_POINT ( 'NONE', #24681 ) ;
#18861 = CARTESIAN_POINT ( 'NONE',  ( 104.9999999999999574, 2.071067811865511032, 1.687500002731185944 ) ) ;
#18862 = VECTOR ( 'NONE', #11977, 1000.000000000000000 ) ;
#18863 = CARTESIAN_POINT ( 'NONE',  ( -8.754898953240607185, 50.00000000000000000, -10.39041163856195027 ) ) ;
#18864 = CARTESIAN_POINT ( 'NONE',  ( 135.6228728715778686, 35.29492187716788720, -13.57481594606304753 ) ) ;
#18865 = ADVANCED_FACE ( 'NONE', ( #599 ), #2737, .F. ) ;
#18866 =( BOUNDED_CURVE ( )  B_SPLINE_CURVE ( 2, ( #3643, #28002, #25155, #14725, #23580, #21305, #27585, #1927, #19012 ),
 .UNSPECIFIED., .F., .T. ) 
 B_SPLINE_CURVE_WITH_KNOTS ( ( 3, 2, 2, 2, 3 ),
 ( 0.02083333333333358892, 0.03125000000000020123, 0.04166666666666681007, 0.05208333333333342585, 0.06250000000000004163 ),
 .UNSPECIFIED. ) 
 CURVE ( )  GEOMETRIC_REPRESENTATION_ITEM ( )  RATIONAL_B_SPLINE_CURVE ( ( 0.9999999999999981126, 0.9238795325112886259, 1.000000000000000000, 0.9238795325112867385, 1.000000000000000000, 0.9238795325112867385, 1.000000000000000000, 0.9238795325112864054, 1.000000000000000222 ) ) 
 REPRESENTATION_ITEM ( '' )  );
#18867 = CARTESIAN_POINT ( 'NONE',  ( 94.99999999999995737, 1.387778780781445676E-14, 6.999999999999999112 ) ) ;
#18868 = CARTESIAN_POINT ( 'NONE',  ( 99.99999999999995737, 1.387778780781445676E-14, 34.79898987322334136 ) ) ;
#18869 = CARTESIAN_POINT ( 'NONE',  ( 208.1451861577818079, 36.38632812608393863, -1.609821015232357215E-15 ) ) ;
#18870 = ORIENTED_EDGE ( 'NONE', *, *, #9309, .T. ) ;
#18871 =( NAMED_UNIT ( * ) PLANE_ANGLE_UNIT ( ) SI_UNIT ( $, .RADIAN. ) );
#18872 = CARTESIAN_POINT ( 'NONE',  ( 99.99999999999998579, 123.0000000000000000, -5.204170427930421283E-15 ) ) ;
#18873 = CARTESIAN_POINT ( 'NONE',  ( 13.57481594606304931, 33.50898437716787015, 5.622872871577868636 ) ) ;
#18874 = CARTESIAN_POINT ( 'NONE',  ( 96.46446609406721961, 3.535533905932755072, 13.87499999999999822 ) ) ;
#18875 = CARTESIAN_POINT ( 'NONE',  ( 181.8548138422182205, 40.50390625108394005, -5.444914386472297529 ) ) ;
#18876 = DIRECTION ( 'NONE',  ( 0.000000000000000000, -1.000000000000000000, 0.000000000000000000 ) ) ;
#18877 = CARTESIAN_POINT ( 'NONE',  ( 99.99999999999998579, 94.25000000000000000, -4.999999999999997335 ) ) ;
#18878 = AXIS2_PLACEMENT_3D ( 'NONE', #363, #17172, #21747 ) ;
#18879 = CARTESIAN_POINT ( 'NONE',  ( 1.685511649082866548, 35.99999999999997868, 13.05727741351675597 ) ) ;
#18880 = LINE ( 'NONE', #27590, #21394 ) ;
#18881 = CARTESIAN_POINT ( 'NONE',  ( 143.5748159460630404, 32.71523437500000142, -5.622872871577873077 ) ) ;
#18882 = ORIENTED_EDGE ( 'NONE', *, *, #17489, .F. ) ;
#18883 = EDGE_CURVE ( 'NONE', #21904, #3329, #13891, .T. ) ;
#18884 = CARTESIAN_POINT ( 'NONE',  ( -8.049105076161786076E-16, 31.82226562608393650, -13.14518615778179544 ) ) ;
#18885 = CARTESIAN_POINT ( 'NONE',  ( -9.295050272127046043, 40.45429687608393721, -9.295050272127046043 ) ) ;
#18886 = CARTESIAN_POINT ( 'NONE',  ( 97.92893218813451028, -4.999999999999989342, 6.312500002731185056 ) ) ;
#18887 = CARTESIAN_POINT ( 'NONE',  ( 130.0000000000000000, 38.56914062608393579, 13.14518615778179544 ) ) ;
#18888 = CARTESIAN_POINT ( 'NONE',  ( 74.29505027212704249, 37.67617187608393436, 9.295050272127046043 ) ) ;
#18889 = VERTEX_POINT ( 'NONE', #11402 ) ;
#18890 = DIRECTION ( 'NONE',  ( -0.000000000000000000, 1.000000000000000000, -0.000000000000000000 ) ) ;
#18891 = CARTESIAN_POINT ( 'NONE',  ( 13.14518615778179900, 34.55078125108393294, 5.444914386472293977 ) ) ;
#18892 = CARTESIAN_POINT ( 'NONE',  ( 192.1079374786958738, 36.00000000000001421, -13.15766692561456708 ) ) ;
#18893 = EDGE_CURVE ( 'NONE', #6644, #26730, #13618, .T. ) ;
#18894 = CARTESIAN_POINT ( 'NONE',  ( 99.99999999999998579, 128.0000000000000000, 2.500000000000003553 ) ) ;
#18895 = CARTESIAN_POINT ( 'NONE',  ( 107.0000000000000142, 112.2744378736303048, -48.89999999999999858 ) ) ;
#18896 = DIRECTION ( 'NONE',  ( 0.000000000000000000, 0.000000000000000000, 1.000000000000000000 ) ) ;
#18897 = CIRCLE ( 'NONE', #24359, 11.57481594606304398 ) ;
#18898 = CARTESIAN_POINT ( 'NONE',  ( 99.99999999999995737, 85.00000000000000000, -1.387778780781445676E-14 ) ) ;
#18899 = CARTESIAN_POINT ( 'NONE',  ( -5.444914386472299306, 38.32109375108394289, 13.14518615778179722 ) ) ;
#18900 = CARTESIAN_POINT ( 'NONE',  ( 133.8295627579928748, 36.00000000000000000, 12.63428651647566170 ) ) ;
#18901 = CARTESIAN_POINT ( 'NONE',  ( 102.4999999999999858, 124.6000000000000085, -9.847140817659276890E-15 ) ) ;
#18902 = EDGE_CURVE ( 'NONE', #8752, #18933, #21645, .T. ) ;
#18903 = CARTESIAN_POINT ( 'NONE',  ( 101.4615807364564546, 124.4500000010924765, -1.461580736456474794 ) ) ;
#18904 = CARTESIAN_POINT ( 'NONE',  ( 100.8561741729129295, 124.5000000010924737, -2.066987299999998751 ) ) ;
#18905 = CARTESIAN_POINT ( 'NONE',  ( -8.312177448680279460E-16, 37.72578125216787726, -13.57481594606304576 ) ) ;
#18906 = CARTESIAN_POINT ( 'NONE',  ( 95.54126587499995082, 1.846868145590750077, 13.37500000136559386 ) ) ;
#18907 = CYLINDRICAL_SURFACE ( 'NONE', #774, 2.500000000000008882 ) ;
#18908 = AXIS2_PLACEMENT_3D ( 'NONE', #14219, #13651, #9383 ) ;
#18909 = ORIENTED_EDGE ( 'NONE', *, *, #10229, .T. ) ;
#18910 = CARTESIAN_POINT ( 'NONE',  ( 130.0000000000000000, 40.80156249999999574, -13.57481594606304576 ) ) ;
#18911 = CARTESIAN_POINT ( 'NONE',  ( 13.57481594606304576, 39.01562500000000000, -1.662435489736055892E-15 ) ) ;
#18912 = CARTESIAN_POINT ( 'NONE',  ( 97.92893218813451028, 5.000000000000018652, 8.812500000000000000 ) ) ;
#18913 = EDGE_CURVE ( 'NONE', #5976, #12843, #26192, .T. ) ;
#18914 = CARTESIAN_POINT ( 'NONE',  ( 5.622872871577871301, 32.11992187716787583, -13.57481594606304753 ) ) ;
#18915 = DIRECTION ( 'NONE',  ( 0.8660254037844380415, 0.5000000000000013323, 0.000000000000000000 ) ) ;
#18916 = CARTESIAN_POINT ( 'NONE',  ( 104.4587341249999781, 81.87500000136559208, 1.846868145590721655 ) ) ;
#18917 = CARTESIAN_POINT ( 'NONE',  ( 74.29505027212704249, 37.08085937608393579, 9.295050272127046043 ) ) ;
#18918 = CARTESIAN_POINT ( 'NONE',  ( 104.9952793366501851, 103.1245878333314323, -48.67500000273119554 ) ) ;
#18919 = CARTESIAN_POINT ( 'NONE',  ( 99.99999999999998579, 89.99899999999999523, -9.540979117872439019E-15 ) ) ;
#18920 = CARTESIAN_POINT ( 'NONE',  ( 97.93301269999999192, 124.0000000010924879, 0.8561741729129329626 ) ) ;
#18921 = CARTESIAN_POINT ( 'NONE',  ( 65.00000000000000000, 38.91640625216786731, 13.57481594606304576 ) ) ;
#18922 = CARTESIAN_POINT ( 'NONE',  ( 93.00000000000000000, 107.7255621263696526, -52.39999999453763024 ) ) ;
#18923 = CARTESIAN_POINT ( 'NONE',  ( 116.4251840539369454, 40.95039062499999005, -5.622872871577873077 ) ) ;
#18924 = ORIENTED_EDGE ( 'NONE', *, *, #24657, .F. ) ;
#18925 = CARTESIAN_POINT ( 'NONE',  ( 93.00000000000000000, 110.0000000000000000, -50.00000000000000711 ) ) ;
#18926 =( BOUNDED_CURVE ( )  B_SPLINE_CURVE ( 2, ( #23164, #10592, #19300, #8184, #27999, #1508, #27443, #4195, #16876 ),
 .UNSPECIFIED., .F., .T. ) 
 B_SPLINE_CURVE_WITH_KNOTS ( ( 3, 2, 2, 2, 3 ),
 ( 0.1500000000000001332, 0.1750000000000001554, 0.2000000000000001776, 0.2250000000000001998, 0.2500000000000002220 ),
 .UNSPECIFIED. ) 
 CURVE ( )  GEOMETRIC_REPRESENTATION_ITEM ( )  RATIONAL_B_SPLINE_CURVE ( ( 0.9999999999999995559, 0.9238795325112871826, 1.000000000000000000, 0.9238795325112867385, 1.000000000000000000, 0.9238795325112867385, 1.000000000000000000, 0.9238795325112860723, 1.000000000000000666 ) ) 
 REPRESENTATION_ITEM ( '' )  );
#18927 = CARTESIAN_POINT ( 'NONE',  ( -13.14518615778179900, 39.11484375108394573, -5.444914386472297529 ) ) ;
#18928 = CARTESIAN_POINT ( 'NONE',  ( 96.84719886470459471, 81.31250000136559208, -3.152801135295383084 ) ) ;
#18929 = CARTESIAN_POINT ( 'NONE',  ( 120.7049497278729575, 39.85898437608393152, 9.295050272127047819 ) ) ;
#18930 = CARTESIAN_POINT ( 'NONE',  ( 51.42518405393695957, 37.87460937716787868, -5.622872871577873077 ) ) ;
#18931 = CARTESIAN_POINT ( 'NONE',  ( 102.4976396683250783, 117.6869444889999841, -54.22499999726881725 ) ) ;
#18932 = CARTESIAN_POINT ( 'NONE',  ( 13.57481594606304753, 35.98945312716787015, -5.622872871577873077 ) ) ;
#18933 = VERTEX_POINT ( 'NONE', #5860 ) ;
#18934 = CARTESIAN_POINT ( 'NONE',  ( 99.99999999999995737, -4.999999999999990230, 11.25000000000000000 ) ) ;
#18935 = ORIENTED_EDGE ( 'NONE', *, *, #14474, .F. ) ;
#18936 = CARTESIAN_POINT ( 'NONE',  ( 2.414731522848535132E-15, 34.60039062608393579, 13.14518615778179544 ) ) ;
#18937 = CARTESIAN_POINT ( 'NONE',  ( 181.8548138422182205, 36.58476562608393579, 0.000000000000000000 ) ) ;
#18938 = CARTESIAN_POINT ( 'NONE',  ( 13.57481594606304576, 36.73359375216787015, -1.662435489736055892E-15 ) ) ;
#18939 = EDGE_CURVE ( 'NONE', #17592, #8172, #11971, .T. ) ;
#18940 = CARTESIAN_POINT ( 'NONE',  ( 116.8548138422182205, 38.91640625108393436, -5.444914386472297529 ) ) ;
#18941 = CARTESIAN_POINT ( 'NONE',  ( 94.99999999999995737, 80.06250000273119838, -2.071067811865491493 ) ) ;
#18942 = FACE_OUTER_BOUND ( 'NONE', #15746, .T. ) ;
#18943 = DIRECTION ( 'NONE',  ( -0.000000000000000000, 1.000000000000000000, -0.000000000000000000 ) ) ;
#18944 = AXIS2_PLACEMENT_3D ( 'NONE', #2898, #9168, #17860 ) ;
#18945 = CARTESIAN_POINT ( 'NONE',  ( 99.14382582708707048, 123.8000000010924850, -2.066987299999999195 ) ) ;
#18946 = CARTESIAN_POINT ( 'NONE',  ( 185.4011555911795313, 37.72578124999999005, -9.598844408820458085 ) ) ;
#18947 = CARTESIAN_POINT ( 'NONE',  ( 9.598844408820456309, 35.93984374999999432, -9.598844408820458085 ) ) ;
#18948 = CARTESIAN_POINT ( 'NONE',  ( 98.15313185440925281, -4.458734124999987891, 1.875000001365591862 ) ) ;
#18949 = CARTESIAN_POINT ( 'NONE',  ( 59.55508561352770158, 39.61093750108393152, -13.14518615778179900 ) ) ;
#18950 = CARTESIAN_POINT ( 'NONE',  ( 101.8468681455907046, 4.458734125000016313, 8.125000001365592084 ) ) ;
#18951 = CARTESIAN_POINT ( 'NONE',  ( 97.83688103937537051, 103.3426043859339103, -52.10000000546238397 ) ) ;
#18952 = CARTESIAN_POINT ( 'NONE',  ( 95.54126587499999346, 90.87499999863439371, 1.846868145590722543 ) ) ;
#18953 = AXIS2_PLACEMENT_3D ( 'NONE', #25044, #18494, #14472 ) ;
#18954 = CARTESIAN_POINT ( 'NONE',  ( -7.778504368121306634, 36.00000000000000000, 10.60546543669474318 ) ) ;
#18955 = CARTESIAN_POINT ( 'NONE',  ( 13.57481594606304576, 38.22187499999999716, -1.662435489736055892E-15 ) ) ;
#18956 = PLANE ( 'NONE',  #15305 ) ;
#18957 = EDGE_LOOP ( 'NONE', ( #2120, #12171, #18375, #24928 ) ) ;
#18958 = CARTESIAN_POINT ( 'NONE',  ( 101.8468681455906903, 84.37500000136562051, -4.458734125000016313 ) ) ;
#18959 =( BOUNDED_CURVE ( )  B_SPLINE_CURVE ( 2, ( #19569, #21296, #4326, #25986, #8311, #23571, #21152, #10585, #17142 ),
 .UNSPECIFIED., .F., .T. ) 
 B_SPLINE_CURVE_WITH_KNOTS ( ( 3, 2, 2, 2, 3 ),
 ( 0.4500000000000003997, 0.4750000000000003664, 0.5000000000000004441, 0.5250000000000004663, 0.5500000000000004885 ),
 .UNSPECIFIED. ) 
 CURVE ( )  GEOMETRIC_REPRESENTATION_ITEM ( )  RATIONAL_B_SPLINE_CURVE ( ( 0.9999999999999987788, 0.9238795325112879597, 1.000000000000000000, 0.9238795325112867385, 1.000000000000000000, 0.9238795325112867385, 1.000000000000000000, 0.9238795325112854062, 1.000000000000001332 ) ) 
 REPRESENTATION_ITEM ( '' )  );
#18960 = CARTESIAN_POINT ( 'NONE',  ( -13.57481594606304576, 31.57421875216786944, 0.000000000000000000 ) ) ;
#18961 = ORIENTED_EDGE ( 'NONE', *, *, #25699, .T. ) ;
#18962 =( BOUNDED_CURVE ( )  B_SPLINE_CURVE ( 2, ( #22924, #10334, #12054, #20780, #3384 ),
 .UNSPECIFIED., .F., .F. ) 
 B_SPLINE_CURVE_WITH_KNOTS ( ( 3, 2, 3 ),
 ( 0.000000000000000000, 0.01041666666666679446, 0.02083333333333358892 ),
 .UNSPECIFIED. ) 
 CURVE ( )  GEOMETRIC_REPRESENTATION_ITEM ( )  RATIONAL_B_SPLINE_CURVE ( ( 1.000000000000000000, 0.9238795325112867385, 1.000000000000000000, 0.9238795325112848511, 1.000000000000001776 ) ) 
 REPRESENTATION_ITEM ( '' )  );
#18963 = ORIENTED_EDGE ( 'NONE', *, *, #10525, .F. ) ;
#18964 = CIRCLE ( 'NONE', #20361, 15.57481594606304576 ) ;
#18965 = CARTESIAN_POINT ( 'NONE',  ( 2.493653234604083739E-15, 32.46718749999999432, 13.57481594606304576 ) ) ;
#18966 = CARTESIAN_POINT ( 'NONE',  ( 104.4587341249999781, -1.846868145590721655, 7.125000001365592084 ) ) ;
#18967 = ORIENTED_EDGE ( 'NONE', *, *, #17878, .T. ) ;
#18968 = CARTESIAN_POINT ( 'NONE',  ( 102.4976396683250925, 117.6869444889999841, -49.97500000273119269 ) ) ;
#18969 = CARTESIAN_POINT ( 'NONE',  ( 9.295050272127046043, 33.90585937608393152, -9.295050272127046043 ) ) ;
#18970 = CYLINDRICAL_SURFACE ( 'NONE', #21331, 11.57481594606304398 ) ;
#18971 = CARTESIAN_POINT ( 'NONE',  ( -13.14518615778179189, 39.80937500108393579, 5.444914386472304635 ) ) ;
#18972 = CARTESIAN_POINT ( 'NONE',  ( 106.5389055433251002, 105.2492070361643215, -48.32500000273119412 ) ) ;
#18973 = CARTESIAN_POINT ( 'NONE',  ( 94.33688103937537051, 105.8855032339526758, -51.80000000000000426 ) ) ;
#18974 = CARTESIAN_POINT ( 'NONE',  ( 139.2950502721270425, 40.45429687608393721, -9.295050272127046043 ) ) ;
#18975 = CARTESIAN_POINT ( 'NONE',  ( 9.295050272127047819, 33.70742187608393436, 9.295050272127046043 ) ) ;
#18976 = ORIENTED_EDGE ( 'NONE', *, *, #24484, .F. ) ;
#18977 = CARTESIAN_POINT ( 'NONE',  ( 74.59884440882045453, 38.12265624999999858, 9.598844408820456309 ) ) ;
#18978 = CYLINDRICAL_SURFACE ( 'NONE', #19103, 7.000000000000006217 ) ;
#18979 = CARTESIAN_POINT ( 'NONE',  ( 204.0314404224550628, 36.00000000000000000, 9.765766397118353481 ) ) ;
#18980 = CARTESIAN_POINT ( 'NONE',  ( 104.4587341249999781, 1.846868145590750299, 4.000000001365592084 ) ) ;
#18981 = CARTESIAN_POINT ( 'NONE',  ( -9.295050272127044266, 33.70742187608393436, 9.295050272127047819 ) ) ;
#18982 = CARTESIAN_POINT ( 'NONE',  ( 101.8468681455907046, -4.458734124999987891, 5.000000001365592972 ) ) ;
#18983 = CARTESIAN_POINT ( 'NONE',  ( 101.8468681455907046, 84.00000000136560629, 4.458734124999987891 ) ) ;
#18984 = CARTESIAN_POINT ( 'NONE',  ( -13.14518615778179900, 32.56640625108394005, -5.444914386472297529 ) ) ;
#18985 = CARTESIAN_POINT ( 'NONE',  ( 9.295050272127047819, 39.46210937608393721, 9.295050272127046043 ) ) ;
#18986 = CARTESIAN_POINT ( 'NONE',  ( 55.81982418635200816, 55.00000000000000000, 14.99999999999998401 ) ) ;
#18987 = ORIENTED_EDGE ( 'NONE', *, *, #1899, .F. ) ;
#18988 = CARTESIAN_POINT ( 'NONE',  ( -13.14518615778179722, 31.97109375108393792, -5.444914386472297529 ) ) ;
#18989 = EDGE_CURVE ( 'NONE', #19422, #16728, #27468, .T. ) ;
#18990 = CARTESIAN_POINT ( 'NONE',  ( 97.93301270000000613, 123.7000000010924765, -0.8561741729129506151 ) ) ;
#18991 = CARTESIAN_POINT ( 'NONE',  ( 101.8468681455907330, 93.37499999863440792, 4.458734124999980786 ) ) ;
#18992 = CARTESIAN_POINT ( 'NONE',  ( 204.2950502721270425, 36.28710937608393294, 9.295050272127046043 ) ) ;
#18993 = CARTESIAN_POINT ( 'NONE',  ( 108.0825317499999869, 107.3738262389971538, -52.97499999726881015 ) ) ;
#18994 = CARTESIAN_POINT ( 'NONE',  ( 120.4011555911795455, 39.41250000216787441, -9.598844408820458085 ) ) ;
#18995 = ORIENTED_EDGE ( 'NONE', *, *, #22394, .T. ) ;
#18996 = CARTESIAN_POINT ( 'NONE',  ( 70.44491438647229131, 39.41250000108393436, 13.14518615778179189 ) ) ;
#18997 = DIRECTION ( 'NONE',  ( 0.000000000000000000, -0.000000000000000000, 1.000000000000000000 ) ) ;
#18998 = CARTESIAN_POINT ( 'NONE',  ( 208.1451861577818079, 32.41757812608393863, -1.609821015232357215E-15 ) ) ;
#18999 = EDGE_LOOP ( 'NONE', ( #25833, #1593, #18531, #21393 ) ) ;
#19000 = CARTESIAN_POINT ( 'NONE',  ( 96.46446609406726225, 92.62500000000000000, 3.535533905932723986 ) ) ;
#19001 = CARTESIAN_POINT ( 'NONE',  ( 143.5748159460630688, 36.73359375216787015, -1.662435489736055892E-15 ) ) ;
#19002 = VECTOR ( 'NONE', #6486, 1000.000000000000000 ) ;
#19003 = CARTESIAN_POINT ( 'NONE',  ( 124.3771271284221314, 35.39414062716787157, -13.57481594606304753 ) ) ;
#19004 = CARTESIAN_POINT ( 'NONE',  ( 51.85481384221820633, 39.21406250108392300, 5.444914386472304635 ) ) ;
#19005 = CARTESIAN_POINT ( 'NONE',  ( 114.9999999999999858, 120.0000000000000000, -15.00000000000000711 ) ) ;
#19006 = CARTESIAN_POINT ( 'NONE',  ( 189.5550856135277229, 38.22187500108393010, -13.14518615778179900 ) ) ;
#19007 = VERTEX_POINT ( 'NONE', #14530 ) ;
#19008 = VERTEX_POINT ( 'NONE', #18688 ) ;
#19009 =( NAMED_UNIT ( * ) SI_UNIT ( $, .STERADIAN. ) SOLID_ANGLE_UNIT ( ) );
#19010 = CARTESIAN_POINT ( 'NONE',  ( 104.9999999999999716, 91.06250000000000000, -2.071067811865478170 ) ) ;
#19011 = FACE_OUTER_BOUND ( 'NONE', #9718, .T. ) ;
#19012 = CARTESIAN_POINT ( 'NONE',  ( 65.00000000000000000, 39.71015625216787015, 13.57481594606304576 ) ) ;
#19013 = CARTESIAN_POINT ( 'NONE',  ( 102.4364866161514556, 122.9999999999999574, 0.6508234534886077061 ) ) ;
#19014 = ADVANCED_FACE ( 'NONE', ( #18549, #3582 ), #18407, .T. ) ;
#19015 = FACE_BOUND ( 'NONE', #13663, .T. ) ;
#19016 = CARTESIAN_POINT ( 'NONE',  ( 12.07727640983618400, 35.99999999999999289, -6.197985357348143154 ) ) ;
#19017 = CARTESIAN_POINT ( 'NONE',  ( 9.180175813648018490, 55.00000000000000711, 14.99999999999999289 ) ) ;
#19018 = CARTESIAN_POINT ( 'NONE',  ( 116.4251840539369596, 32.26874999999999716, 0.000000000000000000 ) ) ;
#19019 = AXIS2_PLACEMENT_3D ( 'NONE', #18483, #27190, #16335 ) ;
#19020 = ORIENTED_EDGE ( 'NONE', *, *, #24118, .T. ) ;
#19021 = CARTESIAN_POINT ( 'NONE',  ( -5.622872871577873077, 40.85117187499999147, -13.57481594606304753 ) ) ;
#19022 = CARTESIAN_POINT ( 'NONE',  ( 5.444914386472297529, 39.51171875108392584, -13.14518615778179900 ) ) ;
#19023 = AXIS2_PLACEMENT_3D ( 'NONE', #20400, #11002, #11141 ) ;
#19024 = CARTESIAN_POINT ( 'NONE',  ( 97.92893218813451028, 5.000000000000018652, 1.937500002731185500 ) ) ;
#19025 = CARTESIAN_POINT ( 'NONE',  ( 143.1451861577818079, 38.81718750108393579, -5.444914386472297529 ) ) ;
#19026 = CARTESIAN_POINT ( 'NONE',  ( 74.29505027212704249, 38.46992187608393010, 9.295050272127046043 ) ) ;
#19027 = CARTESIAN_POINT ( 'NONE',  ( 185.7049497278729575, 39.26367187608393294, 9.295050272127047819 ) ) ;
#19028 = CARTESIAN_POINT ( 'NONE',  ( 99.99999999999998579, 136.0000000000000000, -5.204170427930421283E-15 ) ) ;
#19029 = CARTESIAN_POINT ( 'NONE',  ( -8.049105076161786076E-16, 34.79882812608393294, -13.14518615778179544 ) ) ;
#19030 =( BOUNDED_SURFACE ( )  B_SPLINE_SURFACE ( 1, 2, ( 
 ( #5489, #14158, #16587, #12150, #27430, #27571, #20875, #1360, #8031, #16729, #23293, #2046, #15122, #17561, #28124, #8448, #17278, #21715, #19289, #4463, #21991, #14846, #26265, #23985, #25695, #10850, #13119, #2189, #2468, #8728, #10715, #4047, #6178, #23567, #8589, #10989, #19423, #19563, #1914, #19145, #12844, #12710, #21434, #25980, #23844, #6725, #6451, #17137, #4320, #46, #27987, #21856, #27850, #12979, #6313, #8869, #10579, #25838, #17420, #14989, #15411, #26119, #2331, #6584, #15266, #19701, #187, #24127, #4599, #13259, #8306, #16996, #23706, #4182, #21572, #11273, #15701, #24549, #9431, #24264, #473, #6869, #5172, #24694, #614, #9290, #26551, #22704, #22132, #2611, #13554, #22560, #26986, #11416, #5315, #7146, #18280, #9576, #24403, #22415, #19993 ),
 ( #2753, #9155, #20135, #11696, #13835, #17848, #22278, #3027, #7431, #17986, #15980, #26696, #20421, #15840, #7006, #20271, #5032, #16126, #13698, #4891, #24832, #2884, #905, #13976, #13405, #11129, #19843, #330, #9016, #11555, #17708, #26411, #757, #15555, #4746, #18130, #26842, #7291, #25248, #11984, #6009, #11844, #8139, #10258, #18968, #9719, #5738, #25529, #27539, #18421, #16695, #14673, #1323, #10119, #7863, #22985, #20708, #3452, #3734, #25394, #1190, #14265, #14545, #27675, #12118, #7996, #20845, #5875, #9990, #9858, #12255, #18699, #16833, #27402, #7723, #3172, #18565, #23260, #20567, #5455, #21115, #12394, #1602, #1047, #27267, #27128, #7579, #16557, #16273, #24971, #16415, #14405, #23122, #3597, #25112, #14125, #22846, #3313, #5599, #20982, #1462 ) ),
 .UNSPECIFIED., .F., .F., .F. ) 
 B_SPLINE_SURFACE_WITH_KNOTS ( ( 2, 2 ),
 ( 3, 2, 2, 2, 2, 2, 2, 2, 2, 2, 2, 2, 2, 2, 2, 2, 2, 2, 2, 2, 2, 2, 2, 2, 2, 2, 2, 2, 2, 2, 2, 2, 2, 2, 2, 2, 2, 2, 2, 2, 2, 2, 2, 2, 2, 2, 2, 2, 2, 2, 3 ),
 ( 0.000000000000000000, 1.000000000000000000 ),
 ( 0.000000000000000000, 0.02000000000000000042, 0.04000000000000000083, 0.05999999999999999778, 0.08000000000000000167, 0.1000000000000000056, 0.1199999999999999956, 0.1400000000000000133, 0.1600000000000000033, 0.1799999999999999933, 0.2000000000000000111, 0.2200000000000000011, 0.2399999999999999911, 0.2600000000000000089, 0.2800000000000000266, 0.2999999999999999889, 0.3200000000000000067, 0.3400000000000000244, 0.3599999999999999867, 0.3800000000000000044, 0.4000000000000000222, 0.4199999999999999845, 0.4400000000000000022, 0.4600000000000000200, 0.4799999999999999822, 0.5000000000000000000, 0.5200000000000000178, 0.5400000000000000355, 0.5600000000000000533, 0.5799999999999999600, 0.5999999999999999778, 0.6199999999999999956, 0.6400000000000000133, 0.6600000000000000311, 0.6800000000000000488, 0.6999999999999999556, 0.7199999999999999734, 0.7399999999999999911, 0.7600000000000000089, 0.7800000000000000266, 0.8000000000000000444, 0.8199999999999999512, 0.8399999999999999689, 0.8599999999999999867, 0.8800000000000000044, 0.9000000000000000222, 0.9200000000000000400, 0.9399999999999999467, 0.9599999999999999645, 0.9799999999999999822, 1.000000000000000000 ),
 .UNSPECIFIED. ) 
 GEOMETRIC_REPRESENTATION_ITEM ( )  RATIONAL_B_SPLINE_SURFACE ( (
 ( 1.000000000000000000, 0.9510565162951535312, 1.000000000000000000, 0.9510565162951535312, 1.000000000000000000, 0.9510565162951535312, 1.000000000000000000, 0.9510565162951535312, 1.000000000000000000, 0.9510565162951535312, 1.000000000000000000, 0.9510565162951535312, 1.000000000000000000, 0.9510565162951535312, 1.000000000000000000, 0.9510565162951535312, 1.000000000000000000, 0.9510565162951535312, 1.000000000000000000, 0.9510565162951535312, 1.000000000000000000, 0.9510565162951535312, 1.000000000000000000, 0.9510565162951535312, 1.000000000000000000, 0.9510565162951535312, 1.000000000000000000, 0.9510565162951535312, 1.000000000000000000, 0.9510565162951535312, 1.000000000000000000, 0.9510565162951535312, 1.000000000000000000, 0.9510565162951535312, 1.000000000000000000, 0.9510565162951535312, 1.000000000000000000, 0.9510565162951535312, 1.000000000000000000, 0.9510565162951535312, 1.000000000000000000, 0.9510565162951535312, 1.000000000000000000, 0.9510565162951535312, 1.000000000000000000, 0.9510565162951535312, 1.000000000000000000, 0.9510565162951535312, 1.000000000000000000, 0.9510565162951535312, 1.000000000000000000, 0.9510565162951535312, 1.000000000000000000, 0.9510565162951535312, 1.000000000000000000, 0.9510565162951535312, 1.000000000000000000, 0.9510565162951535312, 1.000000000000000000, 0.9510565162951535312, 1.000000000000000000, 0.9510565162951535312, 1.000000000000000000, 0.9510565162951535312, 1.000000000000000000, 0.9510565162951535312, 1.000000000000000000, 0.9510565162951535312, 1.000000000000000000, 0.9510565162951535312, 1.000000000000000000, 0.9510565162951535312, 1.000000000000000000, 0.9510565162951535312, 1.000000000000000000, 0.9510565162951535312, 1.000000000000000000, 0.9510565162951535312, 1.000000000000000000, 0.9510565162951535312, 1.000000000000000000, 0.9510565162951535312, 1.000000000000000000, 0.9510565162951535312, 1.000000000000000000, 0.9510565162951535312, 1.000000000000000000, 0.9510565162951535312, 1.000000000000000000, 0.9510565162951535312, 1.000000000000000000, 0.9510565162951535312, 1.000000000000000000, 0.9510565162951535312, 1.000000000000000000, 0.9510565162951535312, 1.000000000000000000, 0.9510565162951535312, 1.000000000000000000, 0.9510565162951535312, 1.000000000000000000),
 ( 1.000000000000000000, 0.9510565162951535312, 1.000000000000000000, 0.9510565162951535312, 1.000000000000000000, 0.9510565162951535312, 1.000000000000000000, 0.9510565162951535312, 1.000000000000000000, 0.9510565162951535312, 1.000000000000000000, 0.9510565162951535312, 1.000000000000000000, 0.9510565162951535312, 1.000000000000000000, 0.9510565162951535312, 1.000000000000000000, 0.9510565162951535312, 1.000000000000000000, 0.9510565162951535312, 1.000000000000000000, 0.9510565162951535312, 1.000000000000000000, 0.9510565162951535312, 1.000000000000000000, 0.9510565162951535312, 1.000000000000000000, 0.9510565162951535312, 1.000000000000000000, 0.9510565162951535312, 1.000000000000000000, 0.9510565162951535312, 1.000000000000000000, 0.9510565162951535312, 1.000000000000000000, 0.9510565162951535312, 1.000000000000000000, 0.9510565162951535312, 1.000000000000000000, 0.9510565162951535312, 1.000000000000000000, 0.9510565162951535312, 1.000000000000000000, 0.9510565162951535312, 1.000000000000000000, 0.9510565162951535312, 1.000000000000000000, 0.9510565162951535312, 1.000000000000000000, 0.9510565162951535312, 1.000000000000000000, 0.9510565162951535312, 1.000000000000000000, 0.9510565162951535312, 1.000000000000000000, 0.9510565162951535312, 1.000000000000000000, 0.9510565162951535312, 1.000000000000000000, 0.9510565162951535312, 1.000000000000000000, 0.9510565162951535312, 1.000000000000000000, 0.9510565162951535312, 1.000000000000000000, 0.9510565162951535312, 1.000000000000000000, 0.9510565162951535312, 1.000000000000000000, 0.9510565162951535312, 1.000000000000000000, 0.9510565162951535312, 1.000000000000000000, 0.9510565162951535312, 1.000000000000000000, 0.9510565162951535312, 1.000000000000000000, 0.9510565162951535312, 1.000000000000000000, 0.9510565162951535312, 1.000000000000000000, 0.9510565162951535312, 1.000000000000000000, 0.9510565162951535312, 1.000000000000000000, 0.9510565162951535312, 1.000000000000000000, 0.9510565162951535312, 1.000000000000000000, 0.9510565162951535312, 1.000000000000000000, 0.9510565162951535312, 1.000000000000000000, 0.9510565162951535312, 1.000000000000000000, 0.9510565162951535312, 1.000000000000000000, 0.9510565162951535312, 1.000000000000000000, 0.9510565162951535312, 1.000000000000000000) ) ) 
 REPRESENTATION_ITEM ( '' )  SURFACE ( )  );
#19031 = CARTESIAN_POINT ( 'NONE',  ( 102.0710678118654329, -4.999999999999989342, 9.437500002731184168 ) ) ;
#19032 = CARTESIAN_POINT ( 'NONE',  ( -15.00000000000000355, 55.00000000000000000, -14.99999999999999822 ) ) ;
#19033 = CARTESIAN_POINT ( 'NONE',  ( 65.00000000000000000, -7.395377635281828788, -13.57481594606305109 ) ) ;
#19034 = EDGE_LOOP ( 'NONE', ( #7893, #14535, #16229, #5215, #12807, #9011 ) ) ;
#19035 = CARTESIAN_POINT ( 'NONE',  ( 9.295050272127047819, 37.67617187608393436, 9.295050272127046043 ) ) ;
#19036 = CARTESIAN_POINT ( 'NONE',  ( 142.0095733385115864, 36.00000000000000000, 5.901833544881823990 ) ) ;
#19037 = CARTESIAN_POINT ( 'NONE',  ( 98.23223304703363112, 124.1000000000000085, -1.767766952966370209 ) ) ;
#19038 = AXIS2_PLACEMENT_3D ( 'NONE', #9119, #6973, #15668 ) ;
#19039 = CARTESIAN_POINT ( 'NONE',  ( 104.9999999999999716, 1.449011120738813565E-14, 10.49999999999999822 ) ) ;
#19040 = CARTESIAN_POINT ( 'NONE',  ( 98.53841926354351699, 123.2500000010924737, 1.461580736456455920 ) ) ;
#19041 = EDGE_CURVE ( 'NONE', #11228, #27159, #27306, .T. ) ;
#19042 = CARTESIAN_POINT ( 'NONE',  ( -13.57481594606304576, 40.30546875216787583, 0.000000000000000000 ) ) ;
#19043 = CIRCLE ( 'NONE', #6755, 5.000000000000000888 ) ;
#19044 = CARTESIAN_POINT ( 'NONE',  ( 96.84719886470459471, 3.152801135295383084, 11.31250000136559208 ) ) ;
#19045 = CARTESIAN_POINT ( 'NONE',  ( 99.99999999999998579, 125.0000000000000000, -9.540979117872439019E-15 ) ) ;
#19046 = EDGE_LOOP ( 'NONE', ( #6450, #17907 ) ) ;
#19047 = CARTESIAN_POINT ( 'NONE',  ( 99.99999999999998579, 123.7000000021849502, 2.499999999999978684 ) ) ;
#19048 = CARTESIAN_POINT ( 'NONE',  ( -5.444914386472299306, 32.16953125108393152, 13.14518615778179722 ) ) ;
#19049 = CARTESIAN_POINT ( 'NONE',  ( -13.14518615778179722, 33.36015625108393579, -5.444914386472297529 ) ) ;
#19050 = CARTESIAN_POINT ( 'NONE',  ( 13.57481594606304753, 32.81445312716787299, -5.622872871577873077 ) ) ;
#19051 = CARTESIAN_POINT ( 'NONE',  ( 189.3771271284222735, 36.18789062716787441, -13.57481594606318254 ) ) ;
#19052 = CARTESIAN_POINT ( 'NONE',  ( 101.8468681455906903, 81.12500000136559208, -4.458734125000016313 ) ) ;
#19053 = CARTESIAN_POINT ( 'NONE',  ( 74.29505027212704249, 38.66835937608393436, 9.295050272127046043 ) ) ;
#19054 = CARTESIAN_POINT ( 'NONE',  ( 106.5389055433251002, 114.7507929638356785, -46.17500000273119554 ) ) ;
#19055 = CARTESIAN_POINT ( 'NONE',  ( -5.444914386472297529, 40.40468750108393436, -13.14518615778179722 ) ) ;
#19056 = ORIENTED_EDGE ( 'NONE', *, *, #18628, .T. ) ;
#19057 = EDGE_CURVE ( 'NONE', #7211, #6644, #19460, .T. ) ;
#19058 = CARTESIAN_POINT ( 'NONE',  ( 102.0669872999999939, 123.5000000010924595, 0.8561741729129311862 ) ) ;
#19059 = CARTESIAN_POINT ( 'NONE',  ( 130.0000000000000000, 39.21406249999999716, -13.57481594606304576 ) ) ;
#19060 = CARTESIAN_POINT ( 'NONE',  ( 104.3262379212492448, 104.0454443415356991, -51.79999999453762882 ) ) ;
#19061 = CARTESIAN_POINT ( 'NONE',  ( 139.5988444088204403, 39.11484374999999858, -9.598844408820458085 ) ) ;
#19062 = ORIENTED_EDGE ( 'NONE', *, *, #733, .F. ) ;
#19063 = EDGE_CURVE ( 'NONE', #25247, #10395, #3819, .T. ) ;
#19064 = FACE_BOUND ( 'NONE', #14395, .T. ) ;
#19065 = CARTESIAN_POINT ( 'NONE',  ( 95.54126587499995082, 80.50000000136560629, 1.846868145590724986 ) ) ;
#19066 = FACE_OUTER_BOUND ( 'NONE', #16334, .T. ) ;
#19067 = CARTESIAN_POINT ( 'NONE',  ( 78.57481594606305464, 38.32109375216786873, -1.662435489736055892E-15 ) ) ;
#19068 = ADVANCED_FACE ( 'NONE', ( #9647, #2684 ), #5245, .F. ) ;
#19069 = LINE ( 'NONE', #18797, #16607 ) ;
#19070 = COLOUR_RGB ( '', 0.72549020, 0.75294118, 0.79215686) ;
#19071 = CARTESIAN_POINT ( 'NONE',  ( -8.312177448680279460E-16, 36.13828125216787157, -13.57481594606304576 ) ) ;
#19072 = ORIENTED_EDGE ( 'NONE', *, *, #22375, .T. ) ;
#19073 = CIRCLE ( 'NONE', #3177, 5.000000000000000000 ) ;
#19074 = CARTESIAN_POINT ( 'NONE',  ( 103.5355339059327093, 3.535533905932755072, 3.624999999999999556 ) ) ;
#19075 = EDGE_CURVE ( 'NONE', #22143, #25472, #10697, .T. ) ;
#19076 = CARTESIAN_POINT ( 'NONE',  ( 104.9999999999999574, 2.071067811865511032, 1.562500000000000444 ) ) ;
#19077 = CARTESIAN_POINT ( 'NONE',  ( 189.5550856135277229, 38.32109375108394289, 13.14518615778179722 ) ) ;
#19078 = CARTESIAN_POINT ( 'NONE',  ( 104.9999999999999716, 1.449011120738813565E-14, 0.000000000000000000 ) ) ;
#19079 = CARTESIAN_POINT ( 'NONE',  ( 116.8548138422182205, 36.53515625108393294, -5.444914386472297529 ) ) ;
#19080 = CARTESIAN_POINT ( 'NONE',  ( 130.0000000000000000, 52.00000000000000711, -11.57481594606305997 ) ) ;
#19081 = CARTESIAN_POINT ( 'NONE',  ( 94.99999999999995737, 1.387778780781445676E-14, 9.000000000000000000 ) ) ;
#19082 = CARTESIAN_POINT ( 'NONE',  ( 96.84719886470463734, 93.68749999863440792, -3.152801135295366208 ) ) ;
#19083 = LINE ( 'NONE', #23924, #27564 ) ;
#19084 = CARTESIAN_POINT ( 'NONE',  ( 13.14518615778179544, 39.36289062608393152, -1.609821015232357215E-15 ) ) ;
#19085 = CARTESIAN_POINT ( 'NONE',  ( 204.5988444088204687, 38.12265624999999858, 9.598844408820456309 ) ) ;
#19086 = ADVANCED_FACE ( 'NONE', ( #18207 ), #10540, .T. ) ;
#19087 = FACE_OUTER_BOUND ( 'NONE', #6202, .T. ) ;
#19088 = CARTESIAN_POINT ( 'NONE',  ( 99.99999999999995737, 4.458734125000016313, 2.437500001365592084 ) ) ;
#19089 = CARTESIAN_POINT ( 'NONE',  ( 59.55508561352770158, 38.02343750108394005, -13.14518615778179900 ) ) ;
#19090 = CARTESIAN_POINT ( 'NONE',  ( 103.1528011352953342, -3.152801135295355106, 6.812500001365592084 ) ) ;
#19091 = CARTESIAN_POINT ( 'NONE',  ( 97.83688103937537051, 103.3426043859339103, -44.10000000546238397 ) ) ;
#19092 = CARTESIAN_POINT ( 'NONE',  ( 101.8468681455907330, 91.12499999863439371, 4.458734124999979898 ) ) ;
#19093 = VECTOR ( 'NONE', #4522, 1000.000000000000000 ) ;
#19094 = DIRECTION ( 'NONE',  ( 0.000000000000000000, -1.000000000000000000, 0.000000000000000000 ) ) ;
#19095 = CARTESIAN_POINT ( 'NONE',  ( 5.622872871577878406, 40.45429687500001137, 13.57481594606304576 ) ) ;
#19096 = CARTESIAN_POINT ( 'NONE',  ( 51.42518405393695957, 40.65273437608393436, 0.000000000000000000 ) ) ;
#19097 = EDGE_LOOP ( 'NONE', ( #12331, #1018, #16414, #23628, #8039 ) ) ;
#19098 = CARTESIAN_POINT ( 'NONE',  ( 96.84719886470459471, 82.56250000136559208, -3.152801135295383084 ) ) ;
#19099 = EDGE_CURVE ( 'NONE', #1922, #14596, #24208, .T. ) ;
#19100 = CARTESIAN_POINT ( 'NONE',  ( 98.15313185440925281, 91.62499999863440792, -4.458734124999994997 ) ) ;
#19101 = ORIENTED_EDGE ( 'NONE', *, *, #151, .F. ) ;
#19102 = EDGE_CURVE ( 'NONE', #747, #4145, #3438, .T. ) ;
#19103 = AXIS2_PLACEMENT_3D ( 'NONE', #20716, #23270, #6020 ) ;
#19104 = CARTESIAN_POINT ( 'NONE',  ( 200.6228728715777834, 37.37851562716787157, 13.57481594606313813 ) ) ;
#19105 = CARTESIAN_POINT ( 'NONE',  ( 65.00000000000000000, 34.20351562608394147, -13.14518615778179544 ) ) ;
#19106 = ORIENTED_EDGE ( 'NONE', *, *, #606, .F. ) ;
#19107 = CARTESIAN_POINT ( 'NONE',  ( 13.57481594606304576, 32.66562499999999858, -1.662435489736055892E-15 ) ) ;
#19108 = CARTESIAN_POINT ( 'NONE',  ( 104.4587341249999781, 1.846868145590750299, 5.250000001365592972 ) ) ;
#19109 = VERTEX_POINT ( 'NONE', #24682 ) ;
#19110 = CARTESIAN_POINT ( 'NONE',  ( 2.414731522848535132E-15, 35.39414062608393863, 13.14518615778179544 ) ) ;
#19111 = CARTESIAN_POINT ( 'NONE',  ( 13.14518615778179900, 33.75703125108393010, 5.444914386472293977 ) ) ;
#19112 = CARTESIAN_POINT ( 'NONE',  ( 204.5988444088204403, 36.83281250216787583, -9.598844408820458085 ) ) ;
#19113 = EDGE_CURVE ( 'NONE', #26902, #17678, #11156, .T. ) ;
#19114 = CARTESIAN_POINT ( 'NONE',  ( -9.295050272127044266, 39.85898437608393152, 9.295050272127047819 ) ) ;
#19115 = DIRECTION ( 'NONE',  ( 0.000000000000000000, 1.000000000000000000, 0.000000000000000000 ) ) ;
#19116 = CARTESIAN_POINT ( 'NONE',  ( 201.0859442159868138, 54.65299103241510181, 14.99999999999994671 ) ) ;
#19117 = CARTESIAN_POINT ( 'NONE',  ( 135.4449143864723339, 40.50390625108394005, -13.14518615778179722 ) ) ;
#19119 = VECTOR ( 'NONE', #16464, 1000.000000000000000 ) ;
#19118 = CARTESIAN_POINT ( 'NONE',  ( 13.14518615778179900, 39.51171875108392584, 5.444914386472293977 ) ) ;
#19120 = VERTEX_POINT ( 'NONE', #2871 ) ;
#19121 = CARTESIAN_POINT ( 'NONE',  ( 70.62287287157788285, 38.07304687499998863, 13.57481594606304576 ) ) ;
#19122 = LINE ( 'NONE', #23962, #17317 ) ;
#19123 = CARTESIAN_POINT ( 'NONE',  ( 198.8295627579930454, 36.00000000000000000, 12.63428651647560841 ) ) ;
#19124 = CARTESIAN_POINT ( 'NONE',  ( 104.4587341249999781, 1.846868145590750299, 5.000000001365592972 ) ) ;
#19125 = CARTESIAN_POINT ( 'NONE',  ( -13.14518615778179189, 32.07031250108393294, 5.444914386472304635 ) ) ;
#19126 = CARTESIAN_POINT ( 'NONE',  ( 96.84719886470459471, -3.152801135295355994, 1.812500001365591640 ) ) ;
#19127 =( BOUNDED_CURVE ( )  B_SPLINE_CURVE ( 2, ( #10930, #2271, #15494, #4685, #10652, #19360, #9517, #27065, #7516 ),
 .UNSPECIFIED., .F., .F. ) 
 B_SPLINE_CURVE_WITH_KNOTS ( ( 3, 2, 2, 2, 3 ),
 ( 0.1041666666666664909, 0.1145833333333332732, 0.1250000000000000833, 0.1354166666666668517, 0.1458333333333336757 ),
 .UNSPECIFIED. ) 
 CURVE ( )  GEOMETRIC_REPRESENTATION_ITEM ( )  RATIONAL_B_SPLINE_CURVE ( ( 1.000000000000001332, 0.9238795325112854062, 1.000000000000000000, 0.9238795325112867385, 1.000000000000000000, 0.9238795325112867385, 1.000000000000000000, 0.9238795325112842960, 1.000000000000002442 ) ) 
 REPRESENTATION_ITEM ( '' )  );
#19128 = CARTESIAN_POINT ( 'NONE',  ( 95.54126587499996504, 83.75000000136560629, 1.846868145590724986 ) ) ;
#19129 = CARTESIAN_POINT ( 'NONE',  ( -9.295050272127044266, 39.26367187608393294, 9.295050272127047819 ) ) ;
#19130 = ADVANCED_FACE ( 'NONE', ( #15968 ), #20831, .F. ) ;
#19131 = CARTESIAN_POINT ( 'NONE',  ( 181.4251840539369596, 38.56914062499999574, -5.622872871577872189 ) ) ;
#19132 = EDGE_LOOP ( 'NONE', ( #25800, #1601, #17443, #8447 ) ) ;
#19133 = CARTESIAN_POINT ( 'NONE',  ( 1.662435489736055892E-15, 36.00000000000000000, 13.57481594606304576 ) ) ;
#19134 = LINE ( 'NONE', #27840, #7044 ) ;
#19135 = CARTESIAN_POINT ( 'NONE',  ( 100.0265503228089301, 123.0000000000000426, 2.336440708561638768 ) ) ;
#19136 = CARTESIAN_POINT ( 'NONE',  ( 94.99999999999995737, 83.06250000273119838, -2.071067811865491048 ) ) ;
#19137 = CARTESIAN_POINT ( 'NONE',  ( 91.91746824999998466, 110.0000000000000000, -53.87499999726882294 ) ) ;
#19138 = AXIS2_PLACEMENT_3D ( 'NONE', #20852, #16422, #12265 ) ;
#19139 = CARTESIAN_POINT ( 'NONE',  ( 99.99999999999995737, -4.999999999999990230, 6.375000002731185944 ) ) ;
#19140 = ORIENTED_EDGE ( 'NONE', *, *, #2221, .F. ) ;
#19141 = CARTESIAN_POINT ( 'NONE',  ( 65.00000000000000000, 38.56914062608393579, 13.14518615778179544 ) ) ;
#19142 = CYLINDRICAL_SURFACE ( 'NONE', #23915, 13.57481594606304398 ) ;
#19143 = CARTESIAN_POINT ( 'NONE',  ( 13.57481594606304753, 35.09648437499999574, -5.622872871577873966 ) ) ;
#19144 = EDGE_LOOP ( 'NONE', ( #329, #24370, #603, #825 ) ) ;
#19145 = CARTESIAN_POINT ( 'NONE',  ( 107.0000000000000142, 107.7255621263696526, -51.10000000000000142 ) ) ;
#19146 = CARTESIAN_POINT ( 'NONE',  ( -6.085944215997575846, 54.65299103241510181, -15.00000000000000000 ) ) ;
#19147 = CARTESIAN_POINT ( 'NONE',  ( 98.53841926354351699, 123.8500000010924680, -1.461580736456474794 ) ) ;
#19148 = CARTESIAN_POINT ( 'NONE',  ( 143.5748159460630688, 35.14609375216787157, -1.662435489736055892E-15 ) ) ;
#19149 =( REPRESENTATION_RELATIONSHIP ('NONE','NONE', #2411, #19878 ) REPRESENTATION_RELATIONSHIP_WITH_TRANSFORMATION ( #25639 )SHAPE_REPRESENTATION_RELATIONSHIP( ) );
#19150 = CARTESIAN_POINT ( 'NONE',  ( 78.14518615778179367, 39.61093750108393863, -5.444914386472297529 ) ) ;
#19151 = CARTESIAN_POINT ( 'NONE',  ( 2.493653234604083739E-15, 37.22968749999999716, 13.57481594606304576 ) ) ;
#19152 = AXIS2_PLACEMENT_3D ( 'NONE', #1491, #5485, #1630 ) ;
#19153 = CARTESIAN_POINT ( 'NONE',  ( 185.7049497278729575, 36.08867187608393579, 9.295050272127047819 ) ) ;
#19154 = ORIENTED_EDGE ( 'NONE', *, *, #2547, .F. ) ;
#19155 = ORIENTED_EDGE ( 'NONE', *, *, #17241, .T. ) ;
#19156 = CARTESIAN_POINT ( 'NONE',  ( -9.295050272127044266, 32.71523437608393436, 9.295050272127047819 ) ) ;
#19157 = CARTESIAN_POINT ( 'NONE',  ( 103.1528011352953342, -3.152801135295355106, 14.06250000136559208 ) ) ;
#19158 = CARTESIAN_POINT ( 'NONE',  ( -8.312177448680279460E-16, 40.00781250000000000, -13.57481594606304576 ) ) ;
#19159 = CARTESIAN_POINT ( 'NONE',  ( 104.4587341249999781, 84.00000000136560629, -1.846868145590750521 ) ) ;
#19160 = LINE ( 'NONE', #27864, #4883 ) ;
#19161 = CARTESIAN_POINT ( 'NONE',  ( 139.5988444088204403, 40.00781250216787299, -9.598844408820458085 ) ) ;
#19162 = AXIS2_PLACEMENT_3D ( 'NONE', #1367, #8037, #1229 ) ;
#19163 = DIRECTION ( 'NONE',  ( 0.000000000000000000, 0.000000000000000000, -1.000000000000000000 ) ) ;
#19164 = FACE_OUTER_BOUND ( 'NONE', #12974, .T. ) ;
#19165 = CARTESIAN_POINT ( 'NONE',  ( 99.99999999999998579, 93.62499999726881583, 4.999999999999984013 ) ) ;
#19166 = CARTESIAN_POINT ( 'NONE',  ( 214.9999999999999716, 50.00000000000000000, 9.999999999999946709 ) ) ;
#19167 = ORIENTED_EDGE ( 'NONE', *, *, #16850, .F. ) ;
#19168 =( BOUNDED_CURVE ( )  B_SPLINE_CURVE ( 2, ( #17358, #28199, #1982, #121, #14648, #15200, #1712, #26054, #6392 ),
 .UNSPECIFIED., .F., .T. ) 
 B_SPLINE_CURVE_WITH_KNOTS ( ( 3, 2, 2, 2, 3 ),
 ( 0.2291666666666665741, 0.2395833333333332316, 0.2499999999999998335, 0.2604166666666665186, 0.2708333333333330928 ),
 .UNSPECIFIED. ) 
 CURVE ( )  GEOMETRIC_REPRESENTATION_ITEM ( )  RATIONAL_B_SPLINE_CURVE ( ( 1.000000000000000666, 0.9238795325112861834, 1.000000000000000000, 0.9238795325112867385, 1.000000000000000000, 0.9238795325112867385, 1.000000000000000000, 0.9238795325112884038, 0.9999999999999983347 ) ) 
 REPRESENTATION_ITEM ( '' )  );
#19169 = CARTESIAN_POINT ( 'NONE',  ( -13.57481594606304576, 40.25585937499999289, 5.622872871577880183 ) ) ;
#19170 = CARTESIAN_POINT ( 'NONE',  ( 5.622872871577878406, 31.82226562716787654, 13.57481594606304576 ) ) ;
#19171 = CARTESIAN_POINT ( 'NONE',  ( 104.9999999999999574, 2.071067811865491937, 2.687500002731185500 ) ) ;
#19172 = CARTESIAN_POINT ( 'NONE',  ( 139.2950502721270425, 37.27929687608394005, -9.295050272127046043 ) ) ;
#19173 = CARTESIAN_POINT ( 'NONE',  ( 59.55508561352770158, 36.43593750108392726, -13.14518615778179900 ) ) ;
#19174 = CARTESIAN_POINT ( 'NONE',  ( 195.0000000000000000, 38.96601562608393721, -13.14518615778179544 ) ) ;
#19175 = CARTESIAN_POINT ( 'NONE',  ( 52.00051176980939260, 36.00000000000000000, 1.999176114741853638 ) ) ;
#19176 = CARTESIAN_POINT ( 'NONE',  ( 2.414731522848535132E-15, 36.78320312608393294, 13.14518615778179544 ) ) ;
#19177 = CARTESIAN_POINT ( 'NONE',  ( 128.1856446454164598, 51.46618445021834987, -14.99999999999965716 ) ) ;
#19178 = CARTESIAN_POINT ( 'NONE',  ( 191.8638263786528171, 36.00000000000002842, 12.79489613812767068 ) ) ;
#19179 = CARTESIAN_POINT ( 'NONE',  ( 0.000000000000000000, -7.395377635281828788, 0.000000000000000000 ) ) ;
#19180 = ADVANCED_FACE ( 'NONE', ( #26973 ), #745, .F. ) ;
#19181 = CARTESIAN_POINT ( 'NONE',  ( -8.049105076161786076E-16, 38.76757812608393294, -13.14518615778179544 ) ) ;
#19182 = CARTESIAN_POINT ( 'NONE',  ( 8.392215291638386532, 54.99999999999999289, 14.99999999999999645 ) ) ;
#19183 = CARTESIAN_POINT ( 'NONE',  ( 101.7677669529663547, 124.5000000000000000, 1.767766952966350891 ) ) ;
#19184 = CARTESIAN_POINT ( 'NONE',  ( 98.53841926354351699, 123.0500000010924850, -1.461580736456474794 ) ) ;
#19186 = ORIENTED_EDGE ( 'NONE', *, *, #7742, .F. ) ;
#19185 = DIRECTION ( 'NONE',  ( -0.000000000000000000, -1.000000000000000000, -0.000000000000000000 ) ) ;
#19187 =( LENGTH_UNIT ( ) NAMED_UNIT ( * ) SI_UNIT ( .MILLI., .METRE. ) );
#19188 = CARTESIAN_POINT ( 'NONE',  ( 96.84719886470459471, 3.152801135295383084, 13.31250000136559386 ) ) ;
#19189 = LINE ( 'NONE', #23473, #25340 ) ;
#19190 = ORIENTED_EDGE ( 'NONE', *, *, #6000, .T. ) ;
#19191 = CARTESIAN_POINT ( 'NONE',  ( 98.23223304703363112, 124.2000000021849502, -1.767766952966370209 ) ) ;
#19192 = CARTESIAN_POINT ( 'NONE',  ( 103.1528011352953342, -3.152801135295355106, 11.81250000136559208 ) ) ;
#19193 = CARTESIAN_POINT ( 'NONE',  ( -5.444914386472297529, 33.26093750108393721, -13.14518615778179722 ) ) ;
#19194 = CARTESIAN_POINT ( 'NONE',  ( -13.57481594606304753, 33.11210937716786873, -5.622872871577873077 ) ) ;
#19195 = CARTESIAN_POINT ( 'NONE',  ( 99.99999999999995737, 5.000000000000018652, 2.875000002731185944 ) ) ;
#19196 = CARTESIAN_POINT ( 'NONE',  ( 99.99999999999995737, 81.68750000136559208, 4.458734124999988779 ) ) ;
#19197 = CARTESIAN_POINT ( 'NONE',  ( 74.29505027212704249, 38.07304687608393579, -9.295050272127046043 ) ) ;
#19198 = CARTESIAN_POINT ( 'NONE',  ( 93.46109445667491400, 105.2492070361643215, -47.17500000273119554 ) ) ;
#19199 = FACE_OUTER_BOUND ( 'NONE', #17242, .T. ) ;
#19200 = VERTEX_POINT ( 'NONE', #22836 ) ;
#19201 = CARTESIAN_POINT ( 'NONE',  ( 98.53841926354351699, 124.0500000010924708, 1.461580736456455920 ) ) ;
#19202 = CARTESIAN_POINT ( 'NONE',  ( 139.1801758136479918, 55.00000000000000000, -9.999999999999998224 ) ) ;
#19203 = CARTESIAN_POINT ( 'NONE',  ( 99.99999999999997158, 117.3602355696678501, -52.99999999453763166 ) ) ;
#19204 = CARTESIAN_POINT ( 'NONE',  ( 116.4251840539369596, 40.25585937499999289, 5.622872871577880183 ) ) ;
#19205 = VERTEX_POINT ( 'NONE', #9979 ) ;
#19206 = FACE_OUTER_BOUND ( 'NONE', #15667, .T. ) ;
#19207 = CARTESIAN_POINT ( 'NONE',  ( -5.444914386472299306, 40.10703125108393152, 13.14518615778179722 ) ) ;
#19208 = CARTESIAN_POINT ( 'NONE',  ( -5.622872871577873077, 39.66054687716786731, 13.57481594606304753 ) ) ;
#19209 = CARTESIAN_POINT ( 'NONE',  ( 135.4449143864723055, 39.51171875108392584, -13.14518615778179900 ) ) ;
#19210 = CARTESIAN_POINT ( 'NONE',  ( 55.40115559117954547, 35.64218750216787868, 9.598844408820459861 ) ) ;
#19211 = CARTESIAN_POINT ( 'NONE',  ( 108.0825317499999869, 112.6261737610028320, -50.52499999726881441 ) ) ;
#19212 = CARTESIAN_POINT ( 'NONE',  ( 5.622872871577878406, 35.79101562716787299, 13.57481594606304576 ) ) ;
#19213 = ORIENTED_EDGE ( 'NONE', *, *, #6344, .T. ) ;
#19214 = CARTESIAN_POINT ( 'NONE',  ( 99.99999999999995737, 5.000000000000018652, 4.749999999999999112 ) ) ;
#19215 = CARTESIAN_POINT ( 'NONE',  ( 93.00000000000000000, 110.0000000000000000, -46.50000000546238255 ) ) ;
#19216 = CARTESIAN_POINT ( 'NONE',  ( 200.4449143864723055, 38.71796875108393721, -13.14518615778179900 ) ) ;
#19217 = EDGE_CURVE ( 'NONE', #1696, #18432, #24959, .T. ) ;
#19218 = CARTESIAN_POINT ( 'NONE',  ( -20.00000000000000355, 55.00000000000000000, -9.999999999999998224 ) ) ;
#19219 = AXIS2_PLACEMENT_3D ( 'NONE', #20499, #19922, #15486 ) ;
#19220 = CARTESIAN_POINT ( 'NONE',  ( 135.4449143864723339, 36.83281250108392868, 13.14518615778179189 ) ) ;
#19221 = CARTESIAN_POINT ( 'NONE',  ( 13.57481594606304576, 35.84062499999999574, -1.662435489736055892E-15 ) ) ;
#19222 = EDGE_CURVE ( 'NONE', #17238, #12623, #1178, .T. ) ;
#19223 = CARTESIAN_POINT ( 'NONE',  ( 94.99999999999995737, 1.387778780781445676E-14, 5.125000002731184168 ) ) ;
#19224 = CARTESIAN_POINT ( 'NONE',  ( 96.84719886470463734, 94.93749999863440792, 3.152801135295351997 ) ) ;
#19225 = CARTESIAN_POINT ( 'NONE',  ( 97.93301270000000613, 124.5500000010924850, -9.540979117872439019E-15 ) ) ;
#19226 = CARTESIAN_POINT ( 'NONE',  ( 13.14518615778179544, 40.15664062608393436, -1.609821015232357215E-15 ) ) ;
#19227 = CARTESIAN_POINT ( 'NONE',  ( 200.6228728715778686, 38.37070312499999147, -13.57481594606304753 ) ) ;
#19228 = CONTEXT_DEPENDENT_SHAPE_REPRESENTATION ( #24269, #18738 ) ;
#19229 = CARTESIAN_POINT ( 'NONE',  ( 5.622872871577694553, 35.69179687499999432, 13.57481594606322695 ) ) ;
#19230 = CARTESIAN_POINT ( 'NONE',  ( 98.15313185440925281, -4.458734124999987891, 2.875000001365592084 ) ) ;
#19231 = CARTESIAN_POINT ( 'NONE',  ( 55.70494972787295751, 39.06523437608392868, 9.295050272127047819 ) ) ;
#19232 = CARTESIAN_POINT ( 'NONE',  ( 101.8468681455907046, -4.458734124999987891, 6.750000001365592084 ) ) ;
#19233 = CARTESIAN_POINT ( 'NONE',  ( 105.6631189606246295, 105.8855032339526758, -45.70000000546237828 ) ) ;
#19234 = CARTESIAN_POINT ( 'NONE',  ( 104.4587341249999923, 94.37499999863440792, -1.846868145590737198 ) ) ;
#19235 = LINE ( 'NONE', #25646, #6180 ) ;
#19236 = CARTESIAN_POINT ( 'NONE',  ( 5.622872871577871301, 40.75195312500000711, -13.57481594606304753 ) ) ;
#19237 = CARTESIAN_POINT ( 'NONE',  ( 9.180175813647991845, 55.00000000000000000, -14.99999999999999822 ) ) ;
#19238 = EDGE_CURVE ( 'NONE', #12415, #1189, #14344, .T. ) ;
#19239 = ORIENTED_EDGE ( 'NONE', *, *, #19952, .T. ) ;
#19240 = CARTESIAN_POINT ( 'NONE',  ( 95.54126587499995082, 82.75000000136560629, 1.846868145590724986 ) ) ;
#19241 = CARTESIAN_POINT ( 'NONE',  ( 104.9999999999999716, 1.449011120738813565E-14, 6.625000002731185944 ) ) ;
#19242 = ORIENTED_EDGE ( 'NONE', *, *, #7041, .T. ) ;
#19243 = VECTOR ( 'NONE', #10796, 1000.000000000000000 ) ;
#19244 = DIRECTION ( 'NONE',  ( 0.000000000000000000, -0.000000000000000000, 1.000000000000000000 ) ) ;
#19245 = CARTESIAN_POINT ( 'NONE',  ( 55.70494972787295751, 34.50117187608393721, 9.295050272127047819 ) ) ;
#19246 = ORIENTED_EDGE ( 'NONE', *, *, #3410, .F. ) ;
#19247 = DIRECTION ( 'NONE',  ( -0.000000000000000000, 4.625929269271485914E-16, 1.000000000000000000 ) ) ;
#19248 = CARTESIAN_POINT ( 'NONE',  ( 95.54126587499995082, 1.846868145590750077, 3.625000001365592972 ) ) ;
#19249 = ORIENTED_EDGE ( 'NONE', *, *, #6386, .T. ) ;
#19250 = CARTESIAN_POINT ( 'NONE',  ( -13.14518615778179189, 35.24531250108393721, 5.444914386472304635 ) ) ;
#19251 = CARTESIAN_POINT ( 'NONE',  ( 5.444914386472297529, 39.71015625108393010, -13.14518615778179900 ) ) ;
#19252 = CARTESIAN_POINT ( 'NONE',  ( 204.5988444088204403, 39.21406250216787015, -9.598844408820458085 ) ) ;
#19253 = EDGE_CURVE ( 'NONE', #24513, #17238, #724, .T. ) ;
#19254 = CARTESIAN_POINT ( 'NONE',  ( 13.14518615778179722, 36.13828125108393152, 5.444914386472293977 ) ) ;
#19255 = EDGE_CURVE ( 'NONE', #1369, #2793, #2072, .T. ) ;
#19256 = CARTESIAN_POINT ( 'NONE',  ( 3.100818213308542287E-15, 52.00000000000000711, 12.99999999999999645 ) ) ;
#19257 = CARTESIAN_POINT ( 'NONE',  ( 201.8735082435670449, 51.14166184781640112, 15.00000000000191669 ) ) ;
#19258 = CARTESIAN_POINT ( 'NONE',  ( 120.7049497278729575, 39.26367187608393294, 9.295050272127047819 ) ) ;
#19259 = CARTESIAN_POINT ( 'NONE',  ( -8.049105076161786076E-16, 37.37851562608393863, -13.14518615778179544 ) ) ;
#19260 = EDGE_LOOP ( 'NONE', ( #7399, #8442, #24820, #21709 ) ) ;
#19261 = CARTESIAN_POINT ( 'NONE',  ( 143.1451861577818079, 33.80664062608393294, -1.609821015232357215E-15 ) ) ;
#19262 = CARTESIAN_POINT ( 'NONE',  ( 51.42518405393695957, 38.61874999999999147, 0.000000000000000000 ) ) ;
#19263 = CARTESIAN_POINT ( 'NONE',  ( 51.42518405393695957, 39.46210937716787726, -5.622872871577872189 ) ) ;
#19264 = EDGE_CURVE ( 'NONE', #3329, #11554, #19235, .T. ) ;
#19265 = VECTOR ( 'NONE', #22808, 1000.000000000000000 ) ;
#19266 = CARTESIAN_POINT ( 'NONE',  ( 101.8468681455906903, -4.458734124999987891, 14.00000000136559208 ) ) ;
#19267 = CARTESIAN_POINT ( 'NONE',  ( 2.493653234604083739E-15, 38.12265625216787157, 13.57481594606304576 ) ) ;
#19268 = CARTESIAN_POINT ( 'NONE',  ( 98.15313185440925281, -4.458734124999987891, 2.625000001365592084 ) ) ;
#19269 = CARTESIAN_POINT ( 'NONE',  ( 102.4976396683250925, 117.6869444889999841, -49.72500000273119269 ) ) ;
#19270 = CARTESIAN_POINT ( 'NONE',  ( 99.99999999999995737, 4.458734125000016313, 2.437500001365592084 ) ) ;
#19271 = CARTESIAN_POINT ( 'NONE',  ( 99.99999999999998579, 123.2000000000000028, -2.499999999999997780 ) ) ;
#19272 = CARTESIAN_POINT ( 'NONE',  ( 5.444914386472302859, 32.07031250108393294, 13.14518615778179189 ) ) ;
#19273 = CARTESIAN_POINT ( 'NONE',  ( 9.295050272127046043, 39.66054687608393436, -9.295050272127046043 ) ) ;
#19274 = EDGE_CURVE ( 'NONE', #6030, #24651, #25382, .T. ) ;
#19275 = CARTESIAN_POINT ( 'NONE',  ( 104.9952793366501709, 103.1245878333314323, -49.17499999726881299 ) ) ;
#19276 = ORIENTED_EDGE ( 'NONE', *, *, #6013, .T. ) ;
#19277 = CARTESIAN_POINT ( 'NONE',  ( -8.049105076161786076E-16, 32.61601562608393579, -13.14518615778179544 ) ) ;
#19278 = CARTESIAN_POINT ( 'NONE',  ( 99.14382582708708469, 123.6000000010924680, -2.066987299999998751 ) ) ;
#19279 = CYLINDRICAL_SURFACE ( 'NONE', #11173, 13.57481594606304398 ) ;
#19280 = CARTESIAN_POINT ( 'NONE',  ( 99.99999999999997158, 118.4984768113314004, -54.37499999726880873 ) ) ;
#19281 = CARTESIAN_POINT ( 'NONE',  ( -9.598844408820458085, 37.03125000216787299, -9.598844408820458085 ) ) ;
#19282 = CARTESIAN_POINT ( 'NONE',  ( 208.1451861577817795, 39.31328125108392868, 5.444914386472293977 ) ) ;
#19283 = ORIENTED_EDGE ( 'NONE', *, *, #22394, .F. ) ;
#19284 = FACE_OUTER_BOUND ( 'NONE', #4254, .T. ) ;
#19285 = CARTESIAN_POINT ( 'NONE',  ( 2.493653234604083739E-15, 39.61093749999999147, 13.57481594606304576 ) ) ;
#19286 = CARTESIAN_POINT ( 'NONE',  ( 130.0000000000000000, 40.00781250000000000, -13.57481594606304576 ) ) ;
#19287 = VECTOR ( 'NONE', #15342, 1000.000000000000000 ) ;
#19288 = ORIENTED_EDGE ( 'NONE', *, *, #8641, .T. ) ;
#19289 = CARTESIAN_POINT ( 'NONE',  ( 105.6631189606246295, 105.8855032339526758, -53.20000000000000284 ) ) ;
#19290 = DIRECTION ( 'NONE',  ( -0.000000000000000000, -1.000000000000000000, -0.000000000000000000 ) ) ;
#19291 = CARTESIAN_POINT ( 'NONE',  ( 120.4011555911795455, 34.05468750216788010, 9.598844408820459861 ) ) ;
#19292 =( BOUNDED_CURVE ( )  B_SPLINE_CURVE ( 2, ( #1206, #1480, #1758, #27283, #16571, #19131, #16715, #12135, #6029 ),
 .UNSPECIFIED., .F., .F. ) 
 B_SPLINE_CURVE_WITH_KNOTS ( ( 3, 2, 2, 2, 3 ),
 ( 0.2291666666666665741, 0.2395833333333332316, 0.2499999999999998335, 0.2604166666666665186, 0.2708333333333330928 ),
 .UNSPECIFIED. ) 
 CURVE ( )  GEOMETRIC_REPRESENTATION_ITEM ( )  RATIONAL_B_SPLINE_CURVE ( ( 1.000000000000000666, 0.9238795325112861834, 1.000000000000000000, 0.9238795325112867385, 1.000000000000000000, 0.9238795325112867385, 1.000000000000000000, 0.9238795325112884038, 0.9999999999999983347 ) ) 
 REPRESENTATION_ITEM ( '' )  );
#19293 = CARTESIAN_POINT ( 'NONE',  ( 65.00000000000000000, 40.55351562608393579, -13.14518615778179544 ) ) ;
#19294 = ADVANCED_FACE ( 'NONE', ( #10529, #10245 ), #14393, .F. ) ;
#19295 = CARTESIAN_POINT ( 'NONE',  ( 204.2950502721270425, 33.31054687608394005, -9.295050272127046043 ) ) ;
#19296 = ORIENTED_EDGE ( 'NONE', *, *, #25878, .T. ) ;
#19297 = EDGE_LOOP ( 'NONE', ( #3978, #7116, #7578, #1828 ) ) ;
#19298 = CARTESIAN_POINT ( 'NONE',  ( -5.444914386472299306, 38.51953125108393294, 13.14518615778179722 ) ) ;
#19299 =( NAMED_UNIT ( * ) PLANE_ANGLE_UNIT ( ) SI_UNIT ( $, .RADIAN. ) );
#19300 = CARTESIAN_POINT ( 'NONE',  ( 96.46446609406721961, 84.12500000000000000, 3.535533905932727539 ) ) ;
#19301 = CARTESIAN_POINT ( 'NONE',  ( 5.622872871577780707, 38.37070312499999858, -13.57481594606313990 ) ) ;
#19302 = CARTESIAN_POINT ( 'NONE',  ( 104.4587341249999781, 80.87500000136560629, 1.846868145590721655 ) ) ;
#19303 = DIRECTION ( 'NONE',  ( -0.000000000000000000, 1.000000000000000000, -0.000000000000000000 ) ) ;
#19304 = CARTESIAN_POINT ( 'NONE',  ( -13.14518615778179544, 40.75195312608393294, 0.000000000000000000 ) ) ;
#19305 = DIRECTION ( 'NONE',  ( 0.000000000000000000, 0.000000000000000000, -1.000000000000000000 ) ) ;
#19306 = DIRECTION ( 'NONE',  ( -0.000000000000000000, -0.000000000000000000, -1.000000000000000000 ) ) ;
#19307 = CARTESIAN_POINT ( 'NONE',  ( 195.0000000000000000, 39.75976562608394005, -13.14518615778179544 ) ) ;
#19308 = CARTESIAN_POINT ( 'NONE',  ( 130.0000000000000000, 32.07031249999999289, -13.57481594606304576 ) ) ;
#19309 = ORIENTED_EDGE ( 'NONE', *, *, #24151, .T. ) ;
#19310 = CARTESIAN_POINT ( 'NONE',  ( 13.57481594606304576, 36.63437499999999858, -1.662435489736055892E-15 ) ) ;
#19311 = CARTESIAN_POINT ( 'NONE',  ( 2.414731522848535132E-15, 36.78320312608393294, 13.14518615778179544 ) ) ;
#19312 = CARTESIAN_POINT ( 'NONE',  ( 104.9999999999999574, -2.071067811865462627, 1.562500002731185056 ) ) ;
#19313 = CARTESIAN_POINT ( 'NONE',  ( 130.0000000000000000, 37.37851562608393863, -13.14518615778179544 ) ) ;
#19314 = CARTESIAN_POINT ( 'NONE',  ( 78.14518615778179367, 36.18789062608393436, -1.609821015232357215E-15 ) ) ;
#19315 = CARTESIAN_POINT ( 'NONE',  ( 204.2950502721270425, 32.11992187608393579, 9.295050272127046043 ) ) ;
#19316 = CARTESIAN_POINT ( 'NONE',  ( 0.000000000000000000, 10.00000000000000000, 0.000000000000000000 ) ) ;
#19317 = CARTESIAN_POINT ( 'NONE',  ( 13.14518615778179900, 35.44375000108393436, -5.444914386472297529 ) ) ;
#19318 = CARTESIAN_POINT ( 'NONE',  ( 123.1264917564389236, 51.14166184780616931, -15.00000000000458300 ) ) ;
#19319 = CARTESIAN_POINT ( 'NONE',  ( 187.9316343120018189, 35.99999999999998579, 11.09140360074139586 ) ) ;
#19320 = CARTESIAN_POINT ( 'NONE',  ( 104.9999999999999716, 1.449011120738813565E-14, 4.625000002731185944 ) ) ;
#19321 = CARTESIAN_POINT ( 'NONE',  ( 9.295050272127046043, 39.46210937608393010, -9.295050272127046043 ) ) ;
#19322 = DIRECTION ( 'NONE',  ( -0.000000000000000000, 1.000000000000000000, -0.000000000000000000 ) ) ;
#19323 = CARTESIAN_POINT ( 'NONE',  ( 102.4999999999999858, 122.2906688189065818, 0.1932551333443592867 ) ) ;
#19324 = CARTESIAN_POINT ( 'NONE',  ( 62.83004341689117922, 49.99999999883938528, 13.43548448457802991 ) ) ;
#19325 = CARTESIAN_POINT ( 'NONE',  ( 98.15313185440925281, -4.458734124999987891, 8.625000001365593860 ) ) ;
#19326 = CARTESIAN_POINT ( 'NONE',  ( 78.40642364673431075, 35.99999999999999289, 1.227293221036817483 ) ) ;
#19327 = VERTEX_POINT ( 'NONE', #8540 ) ;
#19328 = CARTESIAN_POINT ( 'NONE',  ( 105.6631189606246295, 105.8855032339526758, -53.20000000000000284 ) ) ;
#19329 = CARTESIAN_POINT ( 'NONE',  ( 98.15313185440925281, 4.458734125000016313, 10.25000000136559386 ) ) ;
#19330 = CARTESIAN_POINT ( 'NONE',  ( 5.444914386472297529, 33.16171875108393152, -13.14518615778179722 ) ) ;
#19331 = CARTESIAN_POINT ( 'NONE',  ( -8.049105076161786076E-16, 38.76757812608393294, -13.14518615778179544 ) ) ;
#19332 = CARTESIAN_POINT ( 'NONE',  ( 107.0000000000000000, 110.0000000000000000, -45.00000000000000711 ) ) ;
#19333 = CARTESIAN_POINT ( 'NONE',  ( 96.84719886470459471, 82.56250000136559208, -3.152801135295383084 ) ) ;
#19334 = CARTESIAN_POINT ( 'NONE',  ( 55.70494972787295751, 37.67617187608393436, 9.295050272127047819 ) ) ;
#19335 =( BOUNDED_CURVE ( )  B_SPLINE_CURVE ( 2, ( #24769, #18356, #11920, #16632, #27063, #27208, #20641, #22923, #7513 ),
 .UNSPECIFIED., .F., .F. ) 
 B_SPLINE_CURVE_WITH_KNOTS ( ( 3, 2, 2, 2, 3 ),
 ( 0.1458333333333336757, 0.1562500000000002776, 0.1666666666666669072, 0.1770833333333335369, 0.1875000000000001388 ),
 .UNSPECIFIED. ) 
 CURVE ( )  GEOMETRIC_REPRESENTATION_ITEM ( )  RATIONAL_B_SPLINE_CURVE ( ( 0.9999999999999975575, 0.9238795325112891810, 1.000000000000000000, 0.9238795325112867385, 1.000000000000000000, 0.9238795325112867385, 1.000000000000000000, 0.9238795325112857393, 1.000000000000001110 ) ) 
 REPRESENTATION_ITEM ( '' )  );
#19336 = CARTESIAN_POINT ( 'NONE',  ( 99.99999999999998579, 101.5015231886685854, -50.62500000273119838 ) ) ;
#19337 = DIRECTION ( 'NONE',  ( 5.782411586589358625E-17, -0.000000000000000000, 1.000000000000000000 ) ) ;
#19338 = CARTESIAN_POINT ( 'NONE',  ( 91.91746824999998466, 110.0000000000000000, -55.87499999726882294 ) ) ;
#19339 = CARTESIAN_POINT ( 'NONE',  ( 94.99999999999995737, -2.071067811865475949, 11.18750000273118417 ) ) ;
#19340 = CARTESIAN_POINT ( 'NONE',  ( 102.1631189606246153, 116.6573956140660897, -49.09999999453764019 ) ) ;
#19341 = CARTESIAN_POINT ( 'NONE',  ( 135.4449143864723055, 32.56640625108394005, -13.14518615778179900 ) ) ;
#19342 = ORIENTED_EDGE ( 'NONE', *, *, #23880, .F. ) ;
#19343 = FACE_OUTER_BOUND ( 'NONE', #2917, .T. ) ;
#19344 = ADVANCED_FACE ( 'NONE', ( #27802 ), #4134, .F. ) ;
#19345 = CARTESIAN_POINT ( 'NONE',  ( -13.14518615778179900, 40.70234375108393721, -5.444914386472297529 ) ) ;
#19346 = CARTESIAN_POINT ( 'NONE',  ( 95.54126587499995082, 80.37500000136562051, -1.846868145590750077 ) ) ;
#19347 = CARTESIAN_POINT ( 'NONE',  ( 135.4449143864723055, 37.92421875108392726, -13.14518615778179900 ) ) ;
#19348 = CARTESIAN_POINT ( 'NONE',  ( 65.00000000000000000, 37.72578125216787726, -13.57481594606304576 ) ) ;
#19349 = VECTOR ( 'NONE', #5111, 1000.000000000000000 ) ;
#19350 = CARTESIAN_POINT ( 'NONE',  ( 12.53142549111940518, 36.00000000000000711, -5.200562670744389493 ) ) ;
#19351 = CARTESIAN_POINT ( 'NONE',  ( 13.57481594606304576, 36.73359375216787015, -1.662435489736055892E-15 ) ) ;
#19352 = CARTESIAN_POINT ( 'NONE',  ( 94.99999999999995737, 1.387778780781445676E-14, 6.999999999999999112 ) ) ;
#19353 = CARTESIAN_POINT ( 'NONE',  ( 96.46446609406721961, 3.535533905932755072, 1.875000000000000000 ) ) ;
#19354 = CARTESIAN_POINT ( 'NONE',  ( 189.5550856135277229, 38.81718750108393579, -13.14518615778179900 ) ) ;
#19355 = VECTOR ( 'NONE', #12105, 1000.000000000000000 ) ;
#19356 = CARTESIAN_POINT ( 'NONE',  ( 0.000000000000000000, 40.99999999999999289, 0.000000000000000000 ) ) ;
#19357 = ORIENTED_EDGE ( 'NONE', *, *, #8563, .T. ) ;
#19358 = DIRECTION ( 'NONE',  ( -0.000000000000000000, 1.000000000000000000, -0.000000000000000000 ) ) ;
#19359 = CARTESIAN_POINT ( 'NONE',  ( 104.9999999999999716, 1.449011120738813565E-14, 10.62500000273118594 ) ) ;
#19360 = CARTESIAN_POINT ( 'NONE',  ( 208.5748159460630688, 39.06523437716786873, 5.622872871577868636 ) ) ;
#19361 = CARTESIAN_POINT ( 'NONE',  ( 92.99999999999998579, 110.0000000000000000, -49.00000000000001421 ) ) ;
#19362 = CARTESIAN_POINT ( 'NONE',  ( -13.14518615778179900, 36.73359375108393010, -5.444914386472297529 ) ) ;
#19363 = CARTESIAN_POINT ( 'NONE',  ( -8.049105076161786076E-16, 37.97382812608393721, -13.14518615778179544 ) ) ;
#19364 = CARTESIAN_POINT ( 'NONE',  ( 189.3771271284221314, 39.26367187499999289, -13.57481594606304753 ) ) ;
#19365 = CARTESIAN_POINT ( 'NONE',  ( 97.50236033167492167, 117.6869444889999841, -47.77500000273119696 ) ) ;
#19366 = CARTESIAN_POINT ( 'NONE',  ( 103.1528011352953342, -3.152801135295355106, 2.062500001365591640 ) ) ;
#19367 = CARTESIAN_POINT ( 'NONE',  ( 74.29505027212704249, 39.46210937608393010, -9.295050272127046043 ) ) ;
#19368 = CIRCLE ( 'NONE', #5444, 5.000000000000004441 ) ;
#19369 = CARTESIAN_POINT ( 'NONE',  ( 98.15313185440923860, -4.458734124999987891, 6.625000001365592084 ) ) ;
#19370 = CARTESIAN_POINT ( 'NONE',  ( 107.0000000000000142, 110.0000000000000000, -45.50000000546238255 ) ) ;
#19371 = CARTESIAN_POINT ( 'NONE',  ( 101.8468681455907330, 93.12499999863439371, 4.458734124999979898 ) ) ;
#19372 = CARTESIAN_POINT ( 'NONE',  ( -7.068365687998217517, 35.99999999999998579, 11.09140360074136211 ) ) ;
#19373 = CARTESIAN_POINT ( 'NONE',  ( 13.57481594606304753, 38.27148437500000711, -5.622872871577873077 ) ) ;
#19374 = CARTESIAN_POINT ( 'NONE',  ( 135.4449143864723055, 39.71015625108393010, -13.14518615778179900 ) ) ;
#19375 = ORIENTED_EDGE ( 'NONE', *, *, #20938, .F. ) ;
#19376 = CARTESIAN_POINT ( 'NONE',  ( 99.99999999999995737, 83.75000000000000000, -5.000000000000018652 ) ) ;
#19377 = CIRCLE ( 'NONE', #11608, 4.999999999999989342 ) ;
#19378 = CARTESIAN_POINT ( 'NONE',  ( 95.54126587499999346, 94.87499999863440792, 1.846868145590722543 ) ) ;
#19379 = ORIENTED_EDGE ( 'NONE', *, *, #2921, .F. ) ;
#19380 = FACE_OUTER_BOUND ( 'NONE', #16956, .T. ) ;
#19381 = CARTESIAN_POINT ( 'NONE',  ( 51.85481384221820633, 33.60820312608393579, 0.000000000000000000 ) ) ;
#19382 = VERTEX_POINT ( 'NONE', #6130 ) ;
#19383 = CARTESIAN_POINT ( 'NONE',  ( 5.622872871577733633, 32.81445312500000000, -13.57481594606318254 ) ) ;
#19384 = CARTESIAN_POINT ( 'NONE',  ( 104.4587341249999781, -1.846868145590721655, 1.125000001365592750 ) ) ;
#19385 = ORIENTED_EDGE ( 'NONE', *, *, #8274, .F. ) ;
#19386 = CARTESIAN_POINT ( 'NONE',  ( 94.99999999999995737, 82.12500000273119838, -1.387778780781445676E-14 ) ) ;
#19387 = CARTESIAN_POINT ( 'NONE',  ( -5.444914386472297529, 38.22187500108393010, -13.14518615778179900 ) ) ;
#19388 = CARTESIAN_POINT ( 'NONE',  ( 185.4011555911795313, 37.82500000216787583, -9.598844408820458085 ) ) ;
#19389 = CARTESIAN_POINT ( 'NONE',  ( -9.295050272127044266, 35.89023437608393152, 9.295050272127047819 ) ) ;
#19390 = CARTESIAN_POINT ( 'NONE',  ( 74.59884440882045453, 36.03906250216787299, -9.598844408820458085 ) ) ;
#19391 = CARTESIAN_POINT ( 'NONE',  ( 107.0000000000000284, 107.7255621263696810, -51.10000000000000142 ) ) ;
#19392 = CARTESIAN_POINT ( 'NONE',  ( 130.0000000000000000, 40.55351562608393579, -13.14518615778179544 ) ) ;
#19393 = VERTEX_POINT ( 'NONE', #7984 ) ;
#19394 = CARTESIAN_POINT ( 'NONE',  ( -9.295050272127044266, 38.46992187608393721, 9.295050272127047819 ) ) ;
#19395 = CARTESIAN_POINT ( 'NONE',  ( 116.8548138422182063, 34.15390625108393863, -5.444914386472297529 ) ) ;
#19396 = CARTESIAN_POINT ( 'NONE',  ( 70.62287287157788285, 38.86679687499999858, 13.57481594606304576 ) ) ;
#19397 = DIRECTION ( 'NONE',  ( 0.000000000000000000, -0.8660254037844380415, 0.5000000000000009992 ) ) ;
#19398 = CARTESIAN_POINT ( 'NONE',  ( 95.54126587499995082, 1.846868145590750077, 14.62500000136559208 ) ) ;
#19399 = DIRECTION ( 'NONE',  ( 0.000000000000000000, 0.000000000000000000, 1.000000000000000000 ) ) ;
#19400 = EDGE_CURVE ( 'NONE', #24826, #7547, #16683, .T. ) ;
#19401 = CARTESIAN_POINT ( 'NONE',  ( 96.84719886470459471, -3.152801135295355994, 4.562500001365592084 ) ) ;
#19402 = CARTESIAN_POINT ( 'NONE',  ( 102.4976396683250925, 117.6869444889999841, -51.72500000273119980 ) ) ;
#19403 = DIRECTION ( 'NONE',  ( -0.000000000000000000, -1.000000000000000000, -0.000000000000000000 ) ) ;
#19404 = DIRECTION ( 'NONE',  ( -0.000000000000000000, -1.000000000000000000, -0.000000000000000000 ) ) ;
#19405 = CARTESIAN_POINT ( 'NONE',  ( -13.14518615778179900, 31.77265625108393365, -5.444914386472297529 ) ) ;
#19406 = CARTESIAN_POINT ( 'NONE',  ( 5.444914386472297529, 39.71015625108393010, -13.14518615778179900 ) ) ;
#19407 = FACE_OUTER_BOUND ( 'NONE', #27619, .T. ) ;
#19408 = ORIENTED_EDGE ( 'NONE', *, *, #13516, .F. ) ;
#19409 = CARTESIAN_POINT ( 'NONE',  ( 99.99999999999998579, 117.3602355696678643, -51.00000000546237544 ) ) ;
#19411 = EDGE_CURVE ( 'NONE', #19690, #20676, #15448, .T. ) ;
#19410 = CARTESIAN_POINT ( 'NONE',  ( 102.0669873000000081, 124.2000000010924623, -0.8561741729129508371 ) ) ;
#19412 = CARTESIAN_POINT ( 'NONE',  ( 99.84091028936038015, 123.0000000000000000, 2.314727449556549299 ) ) ;
#19413 = FACE_OUTER_BOUND ( 'NONE', #11649, .T. ) ;
#19414 = EDGE_CURVE ( 'NONE', #5734, #20470, #1452, .T. ) ;
#19415 = CARTESIAN_POINT ( 'NONE',  ( 204.2950502721270425, 37.87460937608393152, -9.295050272127046043 ) ) ;
#19416 = ORIENTED_EDGE ( 'NONE', *, *, #12410, .T. ) ;
#19417 = FACE_OUTER_BOUND ( 'NONE', #23436, .T. ) ;
#19418 = EDGE_CURVE ( 'NONE', #20971, #3596, #21110, .T. ) ;
#19419 = CARTESIAN_POINT ( 'NONE',  ( -15.00000000000000355, 80.00000000000000000, -10.00000000000000000 ) ) ;
#19420 = AXIS2_PLACEMENT_3D ( 'NONE', #14972, #19404, #23691 ) ;
#19421 = DIRECTION ( 'NONE',  ( -0.000000000000000000, -1.000000000000000000, -0.000000000000000000 ) ) ;
#19422 = VERTEX_POINT ( 'NONE', #23793 ) ;
#19423 = CARTESIAN_POINT ( 'NONE',  ( 102.1631189606246295, 103.3426043859339103, -51.40000000000000568 ) ) ;
#19424 = CARTESIAN_POINT ( 'NONE',  ( 9.598844408820456309, 33.65781250216787157, -9.598844408820458085 ) ) ;
#19425 = CARTESIAN_POINT ( 'NONE',  ( 97.93301270000000613, 124.7500000010924737, -9.540979117872439019E-15 ) ) ;
#19426 = EDGE_CURVE ( 'NONE', #210, #23799, #25458, .T. ) ;
#19427 = CARTESIAN_POINT ( 'NONE',  ( 139.5988444088204687, 33.45937500216787441, 9.598844408820456309 ) ) ;
#19428 = CARTESIAN_POINT ( 'NONE',  ( -13.57481594606304398, 33.90585937499999858, 5.622872871577880183 ) ) ;
#19429 = VECTOR ( 'NONE', #10142, 1000.000000000000000 ) ;
#19430 = CARTESIAN_POINT ( 'NONE',  ( 74.29505027212704249, 39.66054687608393436, -9.295050272127046043 ) ) ;
#19431 = FACE_OUTER_BOUND ( 'NONE', #3741, .T. ) ;
#19432 = CARTESIAN_POINT ( 'NONE',  ( 181.8548138422181921, 34.45156250108394147, 5.444914386472304635 ) ) ;
#19433 = ORIENTED_EDGE ( 'NONE', *, *, #27563, .F. ) ;
#19434 = ORIENTED_EDGE ( 'NONE', *, *, #13267, .F. ) ;
#19435 = CARTESIAN_POINT ( 'NONE',  ( 13.14518615778179900, 39.51171875108392584, 5.444914386472293977 ) ) ;
#19436 = PRESENTATION_STYLE_ASSIGNMENT (( #12575 ) ) ;
#19437 = CARTESIAN_POINT ( 'NONE',  ( 103.1528011352953342, 3.152801135295383084, 10.31250000136559208 ) ) ;
#19438 = CARTESIAN_POINT ( 'NONE',  ( 70.44491438647229131, 39.51171875108393294, -13.14518615778179722 ) ) ;
#19439 = EDGE_CURVE ( 'NONE', #5426, #15410, #19941, .T. ) ;
#19440 = CARTESIAN_POINT ( 'NONE',  ( 98.15313185440923860, 79.62500000136560629, 4.458734124999987891 ) ) ;
#19441 = CARTESIAN_POINT ( 'NONE',  ( 208.1451861577818079, 39.31328125108392868, 5.444914386472293977 ) ) ;
#19442 = CARTESIAN_POINT ( 'NONE',  ( 107.0000000000000142, 110.0000000000000000, -45.00000000000000711 ) ) ;
#19443 = CARTESIAN_POINT ( 'NONE',  ( 101.7677669529663547, 123.0999999999999943, -1.767766952966370209 ) ) ;
#19444 = CARTESIAN_POINT ( 'NONE',  ( 65.00000000000000000, -7.395377635281828788, -7.517135062566165128E-15 ) ) ;
#19445 = CARTESIAN_POINT ( 'NONE',  ( 204.2950502721270425, 40.45429687608393721, -9.295050272127046043 ) ) ;
#19446 = CARTESIAN_POINT ( 'NONE',  ( 102.4976396683250783, 117.6869444889999841, -52.22499999726882436 ) ) ;
#19447 = VERTEX_POINT ( 'NONE', #15360 ) ;
#19448 = EDGE_CURVE ( 'NONE', #15488, #2621, #13786, .T. ) ;
#19449 = CARTESIAN_POINT ( 'NONE',  ( 5.622872871577871301, 36.78320312499999289, -13.57481594606304753 ) ) ;
#19450 = CARTESIAN_POINT ( 'NONE',  ( -13.14518615778179900, 35.74140625108393721, -5.444914386472297529 ) ) ;
#19451 = CARTESIAN_POINT ( 'NONE',  ( 94.99999999999995737, -2.071067811865466624, 1.187500002731184390 ) ) ;
#19452 = CARTESIAN_POINT ( 'NONE',  ( 139.2950502721270425, 36.28710937608393294, 9.295050272127046043 ) ) ;
#19453 = TOROIDAL_SURFACE ( 'NONE', #26822, 23.26794919243112503, 1.000000000000000000 ) ;
#19454 = CARTESIAN_POINT ( 'NONE',  ( 51.85481384221820633, 32.61601562608393579, 0.000000000000000000 ) ) ;
#19455 = EDGE_CURVE ( 'NONE', #26410, #11953, #17511, .T. ) ;
#19456 = CARTESIAN_POINT ( 'NONE',  ( 200.4449143864723055, 37.82500000108392868, 13.14518615778179189 ) ) ;
#19457 = CARTESIAN_POINT ( 'NONE',  ( 104.3262379212492590, 104.0454443415356991, -45.80000000546237970 ) ) ;
#19458 = CARTESIAN_POINT ( 'NONE',  ( 2.414731522848535132E-15, 33.60820312608392868, 13.14518615778179544 ) ) ;
#19459 = CARTESIAN_POINT ( 'NONE',  ( 136.1610621748488938, 51.27996893916987631, -15.00000000000069278 ) ) ;
#19460 =( BOUNDED_CURVE ( )  B_SPLINE_CURVE ( 2, ( #20554, #27391, #23245, #27114, #7711, #7850, #1307, #23108, #16404 ),
 .UNSPECIFIED., .F., .F. ) 
 B_SPLINE_CURVE_WITH_KNOTS ( ( 3, 2, 2, 2, 3 ),
 ( 0.7500000000000000000, 0.7589285714285713969, 0.7678571428571429047, 0.7767857142857143016, 0.7857142857142856984 ),
 .UNSPECIFIED. ) 
 CURVE ( )  GEOMETRIC_REPRESENTATION_ITEM ( )  RATIONAL_B_SPLINE_CURVE ( ( 1.000000000000000000, 0.9238795325112867385, 1.000000000000000000, 0.9238795325112867385, 1.000000000000000000, 0.9238795325112867385, 1.000000000000000000, 0.9238795325112867385, 1.000000000000000000 ) ) 
 REPRESENTATION_ITEM ( '' )  );
#19461 = CARTESIAN_POINT ( 'NONE',  ( 0.000000000000000000, 40.99999999999999289, 0.000000000000000000 ) ) ;
#19462 = CARTESIAN_POINT ( 'NONE',  ( -13.14518615778179544, 34.40195312608393152, 0.000000000000000000 ) ) ;
#19463 = CARTESIAN_POINT ( 'NONE',  ( 104.9952793366501709, 116.8754121666685393, -51.82500000273120122 ) ) ;
#19464 = CARTESIAN_POINT ( 'NONE',  ( 13.14518615778179544, 37.77539062608393294, -1.609821015232357215E-15 ) ) ;
#19465 = CARTESIAN_POINT ( 'NONE',  ( -5.622872871577964560, 34.50117187499998295, -13.57481594606295339 ) ) ;
#19466 = CARTESIAN_POINT ( 'NONE',  ( 102.4999999999999716, 123.9500000021849502, -1.035533905932742638 ) ) ;
#19467 = CARTESIAN_POINT ( 'NONE',  ( -5.622872871577736298, 36.18789062716787441, -13.57481594606318254 ) ) ;
#19468 = DIRECTION ( 'NONE',  ( -0.000000000000000000, -1.000000000000000000, -0.000000000000000000 ) ) ;
#19469 = CARTESIAN_POINT ( 'NONE',  ( 99.99999999999995737, 4.458734125000016313, 9.187500001365592084 ) ) ;
#19470 = CARTESIAN_POINT ( 'NONE',  ( 93.00000000000000000, 110.0000000000000000, -54.00000000000000711 ) ) ;
#19471 = CARTESIAN_POINT ( 'NONE',  ( 104.4587341249999781, 1.846868145590750299, 14.00000000136559208 ) ) ;
#19472 = CARTESIAN_POINT ( 'NONE',  ( 59.37712712842216689, 38.07304687716787583, 13.57481594606308128 ) ) ;
#19473 = CARTESIAN_POINT ( 'NONE',  ( 9.295050272127046043, 38.66835937608393436, -9.295050272127046043 ) ) ;
#19474 = CARTESIAN_POINT ( 'NONE',  ( 124.3771271284219893, 38.86679687716787868, 13.57481594606290720 ) ) ;
#19475 = CARTESIAN_POINT ( 'NONE',  ( 99.99999999999995737, 80.43750000136559208, -4.458734125000016313 ) ) ;
#19476 = CARTESIAN_POINT ( 'NONE',  ( 70.44491438647230552, 35.44375000108393436, 13.14518615778179189 ) ) ;
#19477 = CARTESIAN_POINT ( 'NONE',  ( 108.0825317500000153, 110.0000000000000000, -50.12500000273119127 ) ) ;
#19478 = CARTESIAN_POINT ( 'NONE',  ( 13.14518615778179722, 39.41250000108393436, -5.444914386472297529 ) ) ;
#19479 = ORIENTED_EDGE ( 'NONE', *, *, #19944, .T. ) ;
#19480 = DIRECTION ( 'NONE',  ( 5.782411586589358625E-17, -0.000000000000000000, 1.000000000000000000 ) ) ;
#19481 = CARTESIAN_POINT ( 'NONE',  ( 94.99999999999995737, 1.387778780781445676E-14, 0.9999999999999991118 ) ) ;
#19482 = CARTESIAN_POINT ( 'NONE',  ( 102.0710678118654045, 82.31250000000002842, 5.000000000000019540 ) ) ;
#19483 = CARTESIAN_POINT ( 'NONE',  ( 130.0000000000000000, 39.21406249999999716, -13.57481594606304576 ) ) ;
#19484 = ORIENTED_EDGE ( 'NONE', *, *, #6021, .F. ) ;
#19485 = EDGE_CURVE ( 'NONE', #11153, #2183, #8450, .T. ) ;
#19486 = CARTESIAN_POINT ( 'NONE',  ( 0.000000000000000000, 40.99999999999999289, -13.57481594606304576 ) ) ;
#19487 = CARTESIAN_POINT ( 'NONE',  ( 9.295050272127047819, 36.28710937608393294, 9.295050272127046043 ) ) ;
#19488 = CARTESIAN_POINT ( 'NONE',  ( -9.598844408820458085, 37.82500000216787583, -9.598844408820458085 ) ) ;
#19489 = CARTESIAN_POINT ( 'NONE',  ( 124.5550856135277087, 35.93984375108392726, 13.14518615778179722 ) ) ;
#19490 = CARTESIAN_POINT ( 'NONE',  ( 59.37712712842213136, 32.51679687716787726, 13.57481594606304753 ) ) ;
#19491 = CARTESIAN_POINT ( 'NONE',  ( 104.9999999999999716, 83.43750000000001421, 2.071067811865462627 ) ) ;
#19492 = CARTESIAN_POINT ( 'NONE',  ( -9.598844408820454532, 35.64218750216787868, 9.598844408820459861 ) ) ;
#19493 = CIRCLE ( 'NONE', #5392, 7.000000000000006217 ) ;
#19494 = CARTESIAN_POINT ( 'NONE',  ( 99.99999999999995737, -4.999999999999990230, 5.249999999999999112 ) ) ;
#19495 = ORIENTED_EDGE ( 'NONE', *, *, #18902, .F. ) ;
#19496 = AXIS2_PLACEMENT_3D ( 'NONE', #27246, #24138, #4615 ) ;
#19497 = CARTESIAN_POINT ( 'NONE',  ( 181.8548138422182205, 38.96601562608393721, 0.000000000000000000 ) ) ;
#19498 = CARTESIAN_POINT ( 'NONE',  ( -13.57481594606304753, 38.56914062499999574, -5.622872871577872189 ) ) ;
#19499 = CARTESIAN_POINT ( 'NONE',  ( 135.9085077471930276, 36.04503594658366694, 12.68159279706107334 ) ) ;
#19500 = CARTESIAN_POINT ( 'NONE',  ( 101.7677669209684552, 123.0000000000000000, 1.767766984964258992 ) ) ;
#19501 =( BOUNDED_CURVE ( )  B_SPLINE_CURVE ( 2, ( #5787, #5368, #18614, #18333, #27040, #24746, #20616, #25158, #27320 ),
 .UNSPECIFIED., .F., .F. ) 
 B_SPLINE_CURVE_WITH_KNOTS ( ( 3, 2, 2, 2, 3 ),
 ( 0.2291666666666665741, 0.2395833333333332316, 0.2499999999999998335, 0.2604166666666665186, 0.2708333333333330928 ),
 .UNSPECIFIED. ) 
 CURVE ( )  GEOMETRIC_REPRESENTATION_ITEM ( )  RATIONAL_B_SPLINE_CURVE ( ( 1.000000000000000666, 0.9238795325112861834, 1.000000000000000000, 0.9238795325112867385, 1.000000000000000000, 0.9238795325112867385, 1.000000000000000000, 0.9238795325112884038, 0.9999999999999983347 ) ) 
 REPRESENTATION_ITEM ( '' )  );
#19502 = CARTESIAN_POINT ( 'NONE',  ( 55.81982418635200105, 55.00000000000014211, -9.999999999999998224 ) ) ;
#19503 = CARTESIAN_POINT ( 'NONE',  ( 99.99999999999997158, 102.6397644303321215, -47.99999999453763877 ) ) ;
#19504 = CARTESIAN_POINT ( 'NONE',  ( 13.57481594606304753, 35.89023437499999858, -5.622872871577873077 ) ) ;
#19505 = CARTESIAN_POINT ( 'NONE',  ( 195.0000000000000000, 38.42031249999999432, -13.57481594606304576 ) ) ;
#19506 = CARTESIAN_POINT ( 'NONE',  ( -9.295050272127044266, 36.08867187608393579, 9.295050272127047819 ) ) ;
#19507 = CARTESIAN_POINT ( 'NONE',  ( -13.14518615778179900, 39.71015625108393010, -5.444914386472297529 ) ) ;
#19508 = CARTESIAN_POINT ( 'NONE',  ( 189.3771271284221314, 36.08867187500000284, -13.57481594606304753 ) ) ;
#19509 = CARTESIAN_POINT ( 'NONE',  ( 55.40115559117954547, 40.10703124999999147, -9.598844408820458085 ) ) ;
#19510 = LINE ( 'NONE', #14074, #14667 ) ;
#19511 = CARTESIAN_POINT ( 'NONE',  ( 55.70494972787295751, 39.66054687608393436, -9.295050272127046043 ) ) ;
#19512 = CARTESIAN_POINT ( 'NONE',  ( 95.54126587499996504, -1.846868145590724986, 3.500000001365591196 ) ) ;
#19513 = DIRECTION ( 'NONE',  ( 0.000000000000000000, 0.000000000000000000, 1.000000000000000000 ) ) ;
#19514 = CARTESIAN_POINT ( 'NONE',  ( 103.1528011352953484, 93.18749999863440792, 3.152801135295352886 ) ) ;
#19515 = CARTESIAN_POINT ( 'NONE',  ( 96.46446609406726225, 93.49999999726881583, 3.535533905932723986 ) ) ;
#19516 = CARTESIAN_POINT ( 'NONE',  ( -13.57481594606304576, 37.08085937499999574, 5.622872871577880183 ) ) ;
#19517 = CARTESIAN_POINT ( 'NONE',  ( 116.8548138422182063, 40.70234375108393721, -5.444914386472297529 ) ) ;
#19518 = CIRCLE ( 'NONE', #23166, 5.000000000000000888 ) ;
#19519 = VERTEX_POINT ( 'NONE', #420 ) ;
#19520 = CARTESIAN_POINT ( 'NONE',  ( 94.99999999999995737, 84.93750000000001421, -2.071067811865491048 ) ) ;
#19521 = AXIS2_PLACEMENT_3D ( 'NONE', #9093, #22495, #18214 ) ;
#19522 = CARTESIAN_POINT ( 'NONE',  ( 103.1528011352953484, 93.18749999863440792, 3.152801135295352886 ) ) ;
#19523 = EDGE_LOOP ( 'NONE', ( #22738, #22410, #13372, #17733 ) ) ;
#19524 = CARTESIAN_POINT ( 'NONE',  ( 93.00000000000000000, 107.7255621263696526, -48.90000000000001279 ) ) ;
#19525 = CARTESIAN_POINT ( 'NONE',  ( 70.44491438647230552, 35.74140625108393721, -13.14518615778179900 ) ) ;
#19526 = ORIENTED_EDGE ( 'NONE', *, *, #19426, .T. ) ;
#19527 = DIRECTION ( 'NONE',  ( -0.000000000000000000, 1.000000000000000000, -0.000000000000000000 ) ) ;
#19528 = CARTESIAN_POINT ( 'NONE',  ( 104.4587341249999781, 1.846868145590750299, 2.250000001365591640 ) ) ;
#19529 = ORIENTED_EDGE ( 'NONE', *, *, #13642, .T. ) ;
#19530 = CARTESIAN_POINT ( 'NONE',  ( -5.444914386472297529, 34.25312500108393721, -13.14518615778179722 ) ) ;
#19531 = CARTESIAN_POINT ( 'NONE',  ( -9.295050272127046043, 39.85898437608393152, -9.295050272127046043 ) ) ;
#19532 = CARTESIAN_POINT ( 'NONE',  ( 189.3771271284221314, 38.86679687716788578, 13.57481594606304753 ) ) ;
#19533 = CARTESIAN_POINT ( 'NONE',  ( -8.049105076161786076E-16, 36.38632812608393152, -13.14518615778179544 ) ) ;
#19534 = CARTESIAN_POINT ( 'NONE',  ( -9.180175813647991845, 55.00000000000000000, -14.99999999999999822 ) ) ;
#19535 = CARTESIAN_POINT ( 'NONE',  ( 193.0526740779191357, 51.47162402671692405, 15.00000000000193090 ) ) ;
#19536 = CARTESIAN_POINT ( 'NONE',  ( 120.7049497278729575, 36.68398437608393436, -9.295050272127046043 ) ) ;
#19537 = ORIENTED_EDGE ( 'NONE', *, *, #3913, .F. ) ;
#19538 = CARTESIAN_POINT ( 'NONE',  ( 13.14518615778179900, 38.71796875108393721, 5.444914386472293977 ) ) ;
#19539 = EDGE_CURVE ( 'NONE', #210, #11286, #2562, .T. ) ;
#19540 = CARTESIAN_POINT ( 'NONE',  ( 120.7049497278729575, 33.31054687608393294, -9.295050272127046043 ) ) ;
#19541 = CARTESIAN_POINT ( 'NONE',  ( 65.00000000000000000, 34.05468749999999289, 13.57481594606304576 ) ) ;
#19542 = CARTESIAN_POINT ( 'NONE',  ( 5.622872871577912157, 38.17226562716787441, 13.57481594606301023 ) ) ;
#19543 = AXIS2_PLACEMENT_3D ( 'NONE', #4730, #10833, #17543 ) ;
#19544 = CARTESIAN_POINT ( 'NONE',  ( 96.84719886470459471, -3.152801135295355994, 9.812500001365593860 ) ) ;
#19545 = CARTESIAN_POINT ( 'NONE',  ( 99.99999999999995737, 83.87500000273119838, -5.000000000000018652 ) ) ;
#19546 = CARTESIAN_POINT ( 'NONE',  ( 101.8468681455907046, -4.458734124999987891, 12.75000000136559208 ) ) ;
#19547 = CARTESIAN_POINT ( 'NONE',  ( 104.9952793366501851, 103.1245878333314323, -50.42500000273119554 ) ) ;
#19548 = CARTESIAN_POINT ( 'NONE',  ( 99.99999999999995737, 85.00000000000000000, -1.387778780781445676E-14 ) ) ;
#19549 = DIRECTION ( 'NONE',  ( 0.000000000000000000, 0.000000000000000000, -1.000000000000000000 ) ) ;
#19550 = CARTESIAN_POINT ( 'NONE',  ( 97.50236033167490746, 102.3130555110000159, -51.22499999726882436 ) ) ;
#19551 = CARTESIAN_POINT ( 'NONE',  ( 13.14518615778179900, 38.02343750108395426, -5.444914386472297529 ) ) ;
#19552 = CARTESIAN_POINT ( 'NONE',  ( 99.99999999999997158, 118.4984768113314004, -48.37499999726881583 ) ) ;
#19553 = ORIENTED_EDGE ( 'NONE', *, *, #17680, .F. ) ;
#19554 = CARTESIAN_POINT ( 'NONE',  ( 100.8561741729129437, 123.4000000010924509, 2.066987299999979655 ) ) ;
#19555 = CARTESIAN_POINT ( 'NONE',  ( 116.4251840539369596, 37.08085937716787583, -5.622872871577872189 ) ) ;
#19556 = DIRECTION ( 'NONE',  ( -0.000000000000000000, -1.000000000000000000, -0.000000000000000000 ) ) ;
#19557 = CARTESIAN_POINT ( 'NONE',  ( 185.7049497278729575, 40.45429687608393721, -9.295050272127046043 ) ) ;
#19558 = ORIENTED_EDGE ( 'NONE', *, *, #1871, .T. ) ;
#19559 = CARTESIAN_POINT ( 'NONE',  ( 104.9999999999999716, 1.449011120738813565E-14, 7.625000002731185056 ) ) ;
#19560 = CARTESIAN_POINT ( 'NONE',  ( 102.1631189606246295, 103.3426043859339103, -54.40000000000001279 ) ) ;
#19561 = CARTESIAN_POINT ( 'NONE',  ( 95.54126587499996504, 1.387778780781445676E-14, 14.68750000136559208 ) ) ;
#19562 = ORIENTED_EDGE ( 'NONE', *, *, #12437, .F. ) ;
#19563 = CARTESIAN_POINT ( 'NONE',  ( 104.3262379212492590, 104.0454443415356991, -51.29999999999999716 ) ) ;
#19564 = CARTESIAN_POINT ( 'NONE',  ( -13.14518615778179544, 40.55351562608393579, 0.000000000000000000 ) ) ;
#19565 = CIRCLE ( 'NONE', #25033, 9.000000000000007105 ) ;
#19566 = CARTESIAN_POINT ( 'NONE',  ( 143.1451861577818079, 39.36289062608393152, -1.609821015232357215E-15 ) ) ;
#19567 = CARTESIAN_POINT ( 'NONE',  ( -13.14518615778179544, 40.75195312608393294, 0.000000000000000000 ) ) ;
#19568 = CARTESIAN_POINT ( 'NONE',  ( 95.00000000000000000, 94.37499999726881583, -7.551217303480904118E-15 ) ) ;
#19569 = CARTESIAN_POINT ( 'NONE',  ( 99.99999999999995737, 81.87500000273119838, -5.000000000000018652 ) ) ;
#19570 = EDGE_CURVE ( 'NONE', #26178, #6416, #8682, .T. ) ;
#19571 = SPHERICAL_SURFACE ( 'NONE', #10441, 5.000000000000000000 ) ;
#19572 = CARTESIAN_POINT ( 'NONE',  ( 200.4449143864723055, 34.15390625108393863, -13.14518615778179900 ) ) ;
#19573 = ORIENTED_EDGE ( 'NONE', *, *, #20104, .T. ) ;
#19574 = EDGE_CURVE ( 'NONE', #896, #7211, #10866, .T. ) ;
#19575 = ORIENTED_EDGE ( 'NONE', *, *, #618, .F. ) ;
#19576 = CARTESIAN_POINT ( 'NONE',  ( -13.14518615778179900, 39.90859375108394147, -5.444914386472297529 ) ) ;
#19577 = CARTESIAN_POINT ( 'NONE',  ( 101.8468681455907046, 4.458734125000016313, 10.37500000136559208 ) ) ;
#19578 = CARTESIAN_POINT ( 'NONE',  ( 51.85481384221821344, 39.01562500108393294, 5.444914386472304635 ) ) ;
#19579 = CARTESIAN_POINT ( 'NONE',  ( 95.54126587499996504, 80.37500000136563472, -1.846868145590750077 ) ) ;
#19580 = CARTESIAN_POINT ( 'NONE',  ( 204.2950502721270425, 40.05742187608392868, 9.295050272127046043 ) ) ;
#19581 = AXIS2_PLACEMENT_3D ( 'NONE', #20399, #884, #4871 ) ;
#19582 = CARTESIAN_POINT ( 'NONE',  ( -13.14518615778179544, 36.78320312608393294, 0.000000000000000000 ) ) ;
#19583 = CARTESIAN_POINT ( 'NONE',  ( -13.57481594606304398, 39.56132812716787583, 5.622872871577880183 ) ) ;
#19584 = DIRECTION ( 'NONE',  ( -0.000000000000000000, -1.000000000000000000, -0.000000000000000000 ) ) ;
#19585 = CARTESIAN_POINT ( 'NONE',  ( 105.6631189606246295, 105.8855032339526758, -49.20000000000000995 ) ) ;
#19586 = CARTESIAN_POINT ( 'NONE',  ( 95.00472066334982912, 103.1245878333314323, -53.32499999726881157 ) ) ;
#19587 = EDGE_CURVE ( 'NONE', #5192, #12549, #7989, .T. ) ;
#19588 = VERTEX_POINT ( 'NONE', #8964 ) ;
#19589 = CARTESIAN_POINT ( 'NONE',  ( -9.598844408820458085, 37.72578124999999005, -9.598844408820458085 ) ) ;
#19590 = CARTESIAN_POINT ( 'NONE',  ( 13.14518615778179544, 38.56914062608393579, -1.609821015232357215E-15 ) ) ;
#19591 = CARTESIAN_POINT ( 'NONE',  ( 94.99999999999995737, 1.387778780781445676E-14, 3.125000002731185944 ) ) ;
#19592 = CARTESIAN_POINT ( 'NONE',  ( 130.0000000000000000, 34.99726562608393721, -13.14518615778179544 ) ) ;
#19593 = CARTESIAN_POINT ( 'NONE',  ( 65.00000000000000000, 32.81445312608393294, 13.14518615778179544 ) ) ;
#19594 = CARTESIAN_POINT ( 'NONE',  ( 208.1451861577817795, 37.13046875108393863, 5.444914386472293977 ) ) ;
#19595 = CARTESIAN_POINT ( 'NONE',  ( 107.0000000000000142, 110.0000000000000000, -45.50000000546238255 ) ) ;
#19596 = CARTESIAN_POINT ( 'NONE',  ( 126.9553905430760636, 53.89089363584123049, -14.99999999999999822 ) ) ;
#19597 = CARTESIAN_POINT ( 'NONE',  ( 195.0000000000000000, 39.71015625216787015, 13.57481594606304576 ) ) ;
#19598 = EDGE_CURVE ( 'NONE', #6493, #10914, #27575, .T. ) ;
#19599 = DIRECTION ( 'NONE',  ( 0.000000000000000000, -1.000000000000000000, 0.000000000000000000 ) ) ;
#19600 = CARTESIAN_POINT ( 'NONE',  ( 104.9952793366501709, 103.1245878333314465, -52.42500000273119554 ) ) ;
#19601 = CARTESIAN_POINT ( 'NONE',  ( 13.14518615778179900, 33.85625000108393579, -5.444914386472297529 ) ) ;
#19602 = CARTESIAN_POINT ( 'NONE',  ( 99.99999999999995737, 82.75000000000000000, -5.000000000000018652 ) ) ;
#19603 = CARTESIAN_POINT ( 'NONE',  ( 99.99999999999995737, 79.87500000273119838, -5.000000000000018652 ) ) ;
#19604 = DIRECTION ( 'NONE',  ( -5.782411586589357392E-17, 0.000000000000000000, -1.000000000000000000 ) ) ;
#19605 = EDGE_LOOP ( 'NONE', ( #4792, #9773, #5342, #1844 ) ) ;
#19606 = CARTESIAN_POINT ( 'NONE',  ( 103.1528011352953342, -3.152801135295355106, 7.812500001365592084 ) ) ;
#19607 = ORIENTED_EDGE ( 'NONE', *, *, #3410, .T. ) ;
#19608 = CARTESIAN_POINT ( 'NONE',  ( 102.0669872999999939, 122.6000000010924964, -0.8561741729129507261 ) ) ;
#19609 = CARTESIAN_POINT ( 'NONE',  ( 96.84719886470459471, -3.152801135295355994, 13.56250000136559208 ) ) ;
#19610 = CARTESIAN_POINT ( 'NONE',  ( 51.42518405393695957, 37.92421875216787441, 0.000000000000000000 ) ) ;
#19611 = EDGE_CURVE ( 'NONE', #9045, #3560, #23462, .T. ) ;
#19612 = CARTESIAN_POINT ( 'NONE',  ( -5.444914386472297529, 38.02343750108394005, -13.14518615778179900 ) ) ;
#19613 = DIRECTION ( 'NONE',  ( -1.000000000000000000, 0.000000000000000000, 5.782411586589357392E-17 ) ) ;
#19614 = CARTESIAN_POINT ( 'NONE',  ( 104.4587341249999781, 80.25000000136559208, -1.846868145590750299 ) ) ;
#19615 = CARTESIAN_POINT ( 'NONE',  ( 70.44491438647230552, 34.15390625108393863, -13.14518615778179900 ) ) ;
#19616 = CARTESIAN_POINT ( 'NONE',  ( 97.50236033167492167, 102.3130555110000159, -52.72500000273119980 ) ) ;
#19617 = DIRECTION ( 'NONE',  ( -0.000000000000000000, 1.000000000000000000, -0.000000000000000000 ) ) ;
#19618 = VERTEX_POINT ( 'NONE', #708 ) ;
#19619 = DIRECTION ( 'NONE',  ( -1.000000000000000000, 0.000000000000000000, 0.000000000000000000 ) ) ;
#19620 = DIRECTION ( 'NONE',  ( 0.8660254037844418162, 0.4999999999999947264, -0.000000000000000000 ) ) ;
#19621 = LINE ( 'NONE', #9211, #15125 ) ;
#19622 = CARTESIAN_POINT ( 'NONE',  ( 116.4251840539369596, 37.03124999999999289, 0.000000000000000000 ) ) ;
#19623 = CONICAL_SURFACE ( 'NONE', #22358, 25.00000000000001066, 0.9599310885968833640 ) ;
#19624 = VERTEX_POINT ( 'NONE', #11794 ) ;
#19625 = CARTESIAN_POINT ( 'NONE',  ( 99.99999999999998579, 125.0000000000000000, -2.500000000000004885 ) ) ;
#19626 = CARTESIAN_POINT ( 'NONE',  ( -9.295050272127046043, 37.47773437608393010, -9.295050272127046043 ) ) ;
#19627 = CARTESIAN_POINT ( 'NONE',  ( 2.493653234604083739E-15, 36.53515625216787299, 13.57481594606304576 ) ) ;
#19628 =( BOUNDED_CURVE ( )  B_SPLINE_CURVE ( 2, ( #6783, #26174, #15468, #4378, #12895, #2101, #4660, #13322, #2523 ),
 .UNSPECIFIED., .F., .F. ) 
 B_SPLINE_CURVE_WITH_KNOTS ( ( 3, 2, 2, 2, 3 ),
 ( 0.1458333333333336757, 0.1562500000000002776, 0.1666666666666669072, 0.1770833333333335369, 0.1875000000000001388 ),
 .UNSPECIFIED. ) 
 CURVE ( )  GEOMETRIC_REPRESENTATION_ITEM ( )  RATIONAL_B_SPLINE_CURVE ( ( 0.9999999999999975575, 0.9238795325112891810, 1.000000000000000000, 0.9238795325112867385, 1.000000000000000000, 0.9238795325112867385, 1.000000000000000000, 0.9238795325112857393, 1.000000000000001110 ) ) 
 REPRESENTATION_ITEM ( '' )  );
#19629 = CARTESIAN_POINT ( 'NONE',  ( 124.5550856135277087, 35.64218750108392442, -13.14518615778179900 ) ) ;
#19630 = CARTESIAN_POINT ( 'NONE',  ( 59.37712712842213136, 33.31054687716787299, 13.57481594606304753 ) ) ;
#19631 = CARTESIAN_POINT ( 'NONE',  ( 3.829562757992932998, 36.00000000000000000, 12.63428651647562795 ) ) ;
#19632 = CARTESIAN_POINT ( 'NONE',  ( -9.598844408820454532, 32.46718750216787441, 9.598844408820459861 ) ) ;
#19633 = CARTESIAN_POINT ( 'NONE',  ( 94.99999999999995737, 1.387778780781445676E-14, 4.999999999999999112 ) ) ;
#19634 = DIRECTION ( 'NONE',  ( -1.000000000000000000, 0.000000000000000000, 0.000000000000000000 ) ) ;
#19635 = CARTESIAN_POINT ( 'NONE',  ( 208.1451861577817795, 35.34453125108392868, 5.444914386472293977 ) ) ;
#19636 = CARTESIAN_POINT ( 'NONE',  ( -5.622872871577964560, 33.80664062716787299, -13.57481594606295339 ) ) ;
#19637 = CARTESIAN_POINT ( 'NONE',  ( 102.0710678118654897, 92.81249999999998579, 4.999999999999953815 ) ) ;
#19638 = CARTESIAN_POINT ( 'NONE',  ( 101.0355339059327235, 122.4500000021849502, -2.499999999999997780 ) ) ;
#19639 = DIRECTION ( 'NONE',  ( 0.000000000000000000, 0.000000000000000000, 1.000000000000000000 ) ) ;
#19640 = CARTESIAN_POINT ( 'NONE',  ( 137.6165253254808363, 54.91574374957785665, 14.99999999999996447 ) ) ;
#19641 = CARTESIAN_POINT ( 'NONE',  ( 9.598844408820456309, 38.32109374999999574, -9.598844408820458085 ) ) ;
#19642 = CARTESIAN_POINT ( 'NONE',  ( 143.5748159460630688, 38.17226562499999432, 5.622872871577868636 ) ) ;
#19643 = CARTESIAN_POINT ( 'NONE',  ( 13.14518615778179544, 38.76757812608393294, -1.609821015232357215E-15 ) ) ;
#19644 = CARTESIAN_POINT ( 'NONE',  ( 9.295050272127047819, 36.08867187608392868, 9.295050272127046043 ) ) ;
#19645 = CARTESIAN_POINT ( 'NONE',  ( 181.4251840539369596, 35.39414062499999147, -5.622872871577873077 ) ) ;
#19646 = EDGE_CURVE ( 'NONE', #21223, #11873, #16718, .T. ) ;
#19647 = CARTESIAN_POINT ( 'NONE',  ( 95.00472066334981491, 103.1245878333314465, -45.07500000273119412 ) ) ;
#19648 = CARTESIAN_POINT ( 'NONE',  ( 107.0000000000000142, 112.2744378736303190, -45.40000000546237402 ) ) ;
#19649 = CARTESIAN_POINT ( 'NONE',  ( 51.85481384221819923, 35.74140625108393721, -5.444914386472297529 ) ) ;
#19650 = CARTESIAN_POINT ( 'NONE',  ( 99.99999999999998579, 90.00000000000000000, 4.999999999999983125 ) ) ;
#19651 = CARTESIAN_POINT ( 'NONE',  ( 94.33688103937537051, 105.8855032339526758, -44.30000000546237970 ) ) ;
#19652 = CARTESIAN_POINT ( 'NONE',  ( 95.54126587499999346, 94.74999999863440792, -1.846868145590737864 ) ) ;
#19653 = CARTESIAN_POINT ( 'NONE',  ( 98.03825896092904202, 123.0000000000000142, -0.6650219646036082954 ) ) ;
#19654 = CARTESIAN_POINT ( 'NONE',  ( 13.57481594606304753, 35.09648437499998863, -5.622872871577873077 ) ) ;
#19655 = CARTESIAN_POINT ( 'NONE',  ( 130.0000000000000000, 37.37851562608393863, -13.14518615778179544 ) ) ;
#19656 = EDGE_LOOP ( 'NONE', ( #15472, #22443, #23576 ) ) ;
#19657 = ORIENTED_EDGE ( 'NONE', *, *, #19238, .F. ) ;
#19658 = CARTESIAN_POINT ( 'NONE',  ( 98.15313185440925281, 79.87500000136559208, 4.458734124999987891 ) ) ;
#19659 = CARTESIAN_POINT ( 'NONE',  ( 94.99999999999995737, 84.12500000273119838, -1.387778780781445676E-14 ) ) ;
#19660 = CARTESIAN_POINT ( 'NONE',  ( 104.4587341249999923, 92.37499999863440792, -1.846868145590737198 ) ) ;
#19661 = CARTESIAN_POINT ( 'NONE',  ( 63.72886122875935655, 36.00000000000000000, -13.43002483374384504 ) ) ;
#19662 = ORIENTED_EDGE ( 'NONE', *, *, #3875, .T. ) ;
#19663 = CARTESIAN_POINT ( 'NONE',  ( 104.3262379212492448, 104.0454443415356991, -52.30000000000001847 ) ) ;
#19664 = CARTESIAN_POINT ( 'NONE',  ( 51.85481384221820633, 35.98945312608393721, 0.000000000000000000 ) ) ;
#19665 = VERTEX_POINT ( 'NONE', #16224 ) ;
#19666 = CARTESIAN_POINT ( 'NONE',  ( 97.92893218813448186, 95.18749999726880162, -4.999999999999948486 ) ) ;
#19667 = CARTESIAN_POINT ( 'NONE',  ( 104.4587341249999781, -1.846868145590721655, 3.125000001365592528 ) ) ;
#19668 = ORIENTED_EDGE ( 'NONE', *, *, #27980, .F. ) ;
#19669 = CARTESIAN_POINT ( 'NONE',  ( 13.14518615778179722, 35.64218750108393863, -5.444914386472297529 ) ) ;
#19670 =( BOUNDED_SURFACE ( )  B_SPLINE_SURFACE ( 3, 2, ( 
 ( #13280, #19863, #15288 ),
 ( #26138, #19720, #206 ),
 ( #8890, #350, #12995 ),
 ( #66, #21735, #8748 ),
 ( #6604, #24006, #4483 ),
 ( #13139, #3872, #2159 ),
 ( #10548, #4291, #12950 ),
 ( #6149, #19535, #24340 ),
 ( #15094, #23399, #16838 ),
 ( #8144, #21684, #25535 ),
 ( #26091, #10820, #8559 ),
 ( #6015, #8701, #12534 ),
 ( #28096, #14678, #17250 ),
 ( #27823, #21262, #17 ),
 ( #27957, #8413, #25667 ),
 ( #1744, #10409, #12681 ),
 ( #6943, #19257, #19116 ),
 ( #17392, #15639, #14814 ),
 ( #13486, #17103, #8277 ),
 ( #16968, #23539, #4015 ) ),
 .UNSPECIFIED., .F., .F., .F. ) 
 B_SPLINE_SURFACE_WITH_KNOTS ( ( 4, 2, 2, 2, 2, 2, 2, 2, 2, 4 ),
 ( 3, 3 ),
 ( 0.009073803551359451228, 0.01139250602759180747, 0.01371120850382416198, 0.01602991098005651649, 0.01834861345628887100, 0.01950796469440504999, 0.02066731593252122551, 0.02298601840875358349, 0.02530472088498593800, 0.02762342336121829250 ),
 ( 0.000000000000000000, 1.000000000000000000 ),
 .UNSPECIFIED. ) 
 GEOMETRIC_REPRESENTATION_ITEM ( )  RATIONAL_B_SPLINE_SURFACE ( (
 ( 1.000000000000000000, 0.7071067811865473507, 1.000000000000000000),
 ( 1.000000000000000000, 0.7344871497831124696, 1.000000000000000000),
 ( 1.000000000000000000, 0.7612510203315875357, 1.000000000000000000),
 ( 1.000000000000000000, 0.8116663633846998849, 1.000000000000000000),
 ( 1.000000000000000000, 0.8353358059748190456, 1.000000000000000000),
 ( 1.000000000000000000, 0.8764699612589672562, 1.000000000000000000),
 ( 1.000000000000000000, 0.8939017358720030559, 1.000000000000000000),
 ( 1.000000000000000000, 0.9185314935646274881, 1.000000000000000000),
 ( 1.000000000000000000, 0.9256439951239916475, 1.000000000000000000),
 ( 1.000000000000000000, 0.9261623622476302664, 1.000000000000000000),
 ( 1.000000000000000000, 0.9246301385979290854, 1.000000000000000000),
 ( 1.000000000000000000, 0.9183304321347592891, 1.000000000000000000),
 ( 1.000000000000000000, 0.9135987334167980922, 1.000000000000000000),
 ( 1.000000000000000000, 0.8954110486040549599, 1.000000000000000000),
 ( 1.000000000000000000, 0.8779877431160497681, 1.000000000000000000),
 ( 1.000000000000000000, 0.8366182664713029959, 1.000000000000000000),
 ( 1.000000000000000000, 0.8126941604021775678, 1.000000000000000000),
 ( 1.000000000000000000, 0.7617527316299470552, 1.000000000000000000),
 ( 1.000000000000000000, 0.7347103785796862407, 1.000000000000000000),
 ( 1.000000000000000000, 0.7071067811865470176, 1.000000000000000000) ) ) 
 REPRESENTATION_ITEM ( '' )  SURFACE ( )  );
#19671 = CARTESIAN_POINT ( 'NONE',  ( 5.444914386472302859, 39.41250000108393436, 13.14518615778179189 ) ) ;
#19672 = CARTESIAN_POINT ( 'NONE',  ( 208.5748159460630120, 35.98945312716787015, -5.622872871577873077 ) ) ;
#19673 = CARTESIAN_POINT ( 'NONE',  ( 13.14518615778179722, 36.93203125108394147, 5.444914386472293977 ) ) ;
#19674 = CARTESIAN_POINT ( 'NONE',  ( 51.63999894807758295, 40.87597656304196647, 0.000000000000000000 ) ) ;
#19675 = CARTESIAN_POINT ( 'NONE',  ( 143.1451861577818363, 37.22968750108394431, -5.444914386472297529 ) ) ;
#19676 = ORIENTED_EDGE ( 'NONE', *, *, #14713, .F. ) ;
#19677 = CARTESIAN_POINT ( 'NONE',  ( -8.049105076161786076E-16, 38.96601562608393721, -13.14518615778179544 ) ) ;
#19678 = CARTESIAN_POINT ( 'NONE',  ( 139.2950502721270425, 35.49335937608393010, -9.295050272127046043 ) ) ;
#19679 = CARTESIAN_POINT ( 'NONE',  ( 65.00000000000000000, 33.65781249999999147, -13.57481594606304576 ) ) ;
#19680 = CARTESIAN_POINT ( 'NONE',  ( 13.57481594606304753, 38.37070312716787157, -5.622872871577873966 ) ) ;
#19681 = CARTESIAN_POINT ( 'NONE',  ( 104.4587341249999781, 1.846868145590750299, 10.25000000136559386 ) ) ;
#19682 = DIRECTION ( 'NONE',  ( 0.000000000000000000, -1.000000000000000000, 0.000000000000000000 ) ) ;
#19683 = CARTESIAN_POINT ( 'NONE',  ( 96.84719886470459471, 3.152801135295383084, 12.31250000136559208 ) ) ;
#19684 = CARTESIAN_POINT ( 'NONE',  ( 97.50236033167492167, 117.6869444889999841, -51.52500000273119696 ) ) ;
#19685 = CARTESIAN_POINT ( 'NONE',  ( 96.84719886470459471, -3.152801135295355994, 0.8125000013655924169 ) ) ;
#19686 = CARTESIAN_POINT ( 'NONE',  ( 99.99999999999995737, 79.93750000136559208, 4.458734124999988779 ) ) ;
#19687 = CARTESIAN_POINT ( 'NONE',  ( 108.0825317499999869, 107.3738262389971680, -46.72499999726881015 ) ) ;
#19688 = CARTESIAN_POINT ( 'NONE',  ( -9.295050272127046043, 37.47773437608393010, -9.295050272127046043 ) ) ;
#19689 = CARTESIAN_POINT ( 'NONE',  ( 99.99999999999997158, 118.4984768113314004, -50.37499999726881583 ) ) ;
#19690 = VERTEX_POINT ( 'NONE', #22937 ) ;
#19691 = CARTESIAN_POINT ( 'NONE',  ( 100.8561741729129295, 123.7000000010924765, -2.066987299999998751 ) ) ;
#19692 = LINE ( 'NONE', #179, #20730 ) ;
#19693 = CARTESIAN_POINT ( 'NONE',  ( 99.99999999999998579, 90.00000000000000000, -6.938893903907228378E-15 ) ) ;
#19694 = ADVANCED_FACE ( 'NONE', ( #27076 ), #18515, .F. ) ;
#19695 = CARTESIAN_POINT ( 'NONE',  ( 195.0000000000000000, 38.76757812608393294, -13.14518615778179544 ) ) ;
#19696 = ORIENTED_EDGE ( 'NONE', *, *, #27140, .T. ) ;
#19697 = CARTESIAN_POINT ( 'NONE',  ( 139.1801758136479918, 55.00000000000000000, 14.99999999999996270 ) ) ;
#19698 = CARTESIAN_POINT ( 'NONE',  ( 99.99999999999995737, 1.387778780781445676E-14, 34.79898987322334136 ) ) ;
#19699 = CARTESIAN_POINT ( 'NONE',  ( 95.54126587499995082, 1.846868145590750077, 14.62500000136559208 ) ) ;
#19700 = ORIENTED_EDGE ( 'NONE', *, *, #14844, .F. ) ;
#19701 = CARTESIAN_POINT ( 'NONE',  ( 99.99999999999998579, 117.3602355696678501, -48.50000000000000000 ) ) ;
#19702 = CARTESIAN_POINT ( 'NONE',  ( 13.14518615778179900, 39.41250000108393436, -5.444914386472297529 ) ) ;
#19703 = CYLINDRICAL_SURFACE ( 'NONE', #24462, 7.000000000000006217 ) ;
#19704 = CIRCLE ( 'NONE', #23360, 9.000000000000007105 ) ;
#19705 = CARTESIAN_POINT ( 'NONE',  ( 116.4251840539369596, 31.62382812716787228, 5.622872871577880183 ) ) ;
#19706 = CARTESIAN_POINT ( 'NONE',  ( 5.444914386472297529, 39.71015625108393010, -13.14518615778179722 ) ) ;
#19707 =( BOUNDED_CURVE ( )  B_SPLINE_CURVE ( 2, ( #17926, #409, #20503, #9369, #11780, #9654, #696, #2826, #5109 ),
 .UNSPECIFIED., .F., .F. ) 
 B_SPLINE_CURVE_WITH_KNOTS ( ( 3, 2, 2, 2, 3 ),
 ( 0.5625000000000004441, 0.5729166666666669627, 0.5833333333333337034, 0.5937500000000002220, 0.6041666666666668517 ),
 .UNSPECIFIED. ) 
 CURVE ( )  GEOMETRIC_REPRESENTATION_ITEM ( )  RATIONAL_B_SPLINE_CURVE ( ( 0.9999999999999967804, 0.9238795325112899581, 1.000000000000000000, 0.9238795325112867385, 1.000000000000000000, 0.9238795325112867385, 1.000000000000000000, 0.9238795325112850731, 1.000000000000001554 ) ) 
 REPRESENTATION_ITEM ( '' )  );
#19708 = CARTESIAN_POINT ( 'NONE',  ( 104.9999999999999716, 91.81249999726880162, 2.071067811865467956 ) ) ;
#19709 = CARTESIAN_POINT ( 'NONE',  ( 78.14518615778179367, 37.92421875108392726, 5.444914386472293977 ) ) ;
#19710 = CARTESIAN_POINT ( 'NONE',  ( 1.662435489736055892E-15, 31.00000000000000000, 13.57481594606304576 ) ) ;
#19711 = CARTESIAN_POINT ( 'NONE',  ( 189.5550856135277229, 35.34453125108393579, 13.14518615778179722 ) ) ;
#19712 = ORIENTED_EDGE ( 'NONE', *, *, #1669, .T. ) ;
#19713 = ORIENTED_EDGE ( 'NONE', *, *, #24515, .F. ) ;
#19714 = CARTESIAN_POINT ( 'NONE',  ( -13.14518615778179189, 40.00781250108393294, 5.444914386472304635 ) ) ;
#19715 = CARTESIAN_POINT ( 'NONE',  ( 95.54126587499996504, -1.846868145590724986, 10.75000000136559208 ) ) ;
#19716 = CARTESIAN_POINT ( 'NONE',  ( 78.14518615778180788, 40.20625000108393010, -5.444914386472297529 ) ) ;
#19717 = CARTESIAN_POINT ( 'NONE',  ( 103.1528011352953342, 80.06250000136559208, -3.152801135295383084 ) ) ;
#19718 = CARTESIAN_POINT ( 'NONE',  ( 195.0000000000000000, 38.76757812608393294, -13.14518615778179544 ) ) ;
#19719 = CARTESIAN_POINT ( 'NONE',  ( 13.14518615778179722, 37.22968750108394431, -5.444914386472297529 ) ) ;
#19720 = CARTESIAN_POINT ( 'NONE',  ( 186.2273907538555591, 50.37415326815735028, 15.00000000000776978 ) ) ;
#19721 = CARTESIAN_POINT ( 'NONE',  ( 104.9999999999999716, -2.071067811865467956, 12.43749999999999645 ) ) ;
#19722 = CARTESIAN_POINT ( 'NONE',  ( 204.2950502721270425, 40.25585937608393294, 9.295050272127046043 ) ) ;
#19723 = CARTESIAN_POINT ( 'NONE',  ( 108.0825317500000011, 110.0000000000000000, -50.62499999726882294 ) ) ;
#19724 = ORIENTED_EDGE ( 'NONE', *, *, #14702, .F. ) ;
#19725 = AXIS2_PLACEMENT_3D ( 'NONE', #9366, #18060, #26775 ) ;
#19726 = CARTESIAN_POINT ( 'NONE',  ( 13.57481594606304576, 37.42812499999999432, -1.662435489736055892E-15 ) ) ;
#19727 = CARTESIAN_POINT ( 'NONE',  ( -13.14518615778179544, 38.17226562608393436, 0.000000000000000000 ) ) ;
#19728 = ORIENTED_EDGE ( 'NONE', *, *, #5382, .F. ) ;
#19729 = CARTESIAN_POINT ( 'NONE',  ( 116.8548138422182063, 36.83281250108393579, 5.444914386472304635 ) ) ;
#19730 = CARTESIAN_POINT ( 'NONE',  ( 65.00000000000000000, 34.40195312608393152, 13.14518615778179544 ) ) ;
#19731 = CARTESIAN_POINT ( 'NONE',  ( 208.1451861577818079, 37.97382812608393721, -1.609821015232357215E-15 ) ) ;
#19732 = ADVANCED_FACE ( 'NONE', ( #22366 ), #24373, .F. ) ;
#19733 = EDGE_LOOP ( 'NONE', ( #2776, #27996, #13943, #25706 ) ) ;
#19734 = CARTESIAN_POINT ( 'NONE',  ( 64.40674429744949236, 36.00000000000001421, 13.13889047851772851 ) ) ;
#19735 = CARTESIAN_POINT ( 'NONE',  ( -5.444914386472299306, 32.76484375108393010, 13.14518615778179722 ) ) ;
#19736 = CARTESIAN_POINT ( 'NONE',  ( 129.2761280619777153, 53.51529642094997286, -15.00000000000000000 ) ) ;
#19737 = CARTESIAN_POINT ( 'NONE',  ( -20.00000000000000000, 55.00000000000000000, 10.00000000000000178 ) ) ;
#19738 = CARTESIAN_POINT ( 'NONE',  ( 120.4011555911795455, 39.61093750216787868, 9.598844408820459861 ) ) ;
#19739 = CARTESIAN_POINT ( 'NONE',  ( 108.0825317500000153, 110.0000000000000000, -54.12500000273119838 ) ) ;
#19740 = CARTESIAN_POINT ( 'NONE',  ( 197.1298106584279992, 36.02027164734404607, -13.57481594606306174 ) ) ;
#19741 = CARTESIAN_POINT ( 'NONE',  ( 99.99999999999998579, 95.00000000000000000, -6.938893903907228378E-15 ) ) ;
#19742 = CARTESIAN_POINT ( 'NONE',  ( 61.13607473487752486, 54.10645156200381223, 14.99999999999998401 ) ) ;
#19743 =( NAMED_UNIT ( * ) PLANE_ANGLE_UNIT ( ) SI_UNIT ( $, .RADIAN. ) );
#19744 = ORIENTED_EDGE ( 'NONE', *, *, #19439, .F. ) ;
#19745 = CARTESIAN_POINT ( 'NONE',  ( 96.84719886470459471, -3.152801135295355994, 10.56250000136559208 ) ) ;
#19746 = VERTEX_POINT ( 'NONE', #12351 ) ;
#19747 = CARTESIAN_POINT ( 'NONE',  ( 97.93301269999999192, 123.0000000010925163, 0.8561741729129329626 ) ) ;
#19748 = CARTESIAN_POINT ( 'NONE',  ( 104.4587341249999639, 1.442382525525748735E-14, 12.93750000136559208 ) ) ;
#19749 = CARTESIAN_POINT ( 'NONE',  ( 132.0246277255328664, 50.00000000050972915, 13.43320860980955089 ) ) ;
#19750 = CARTESIAN_POINT ( 'NONE',  ( -13.14518615778179900, 38.91640625108393436, -5.444914386472297529 ) ) ;
#19751 = DIRECTION ( 'NONE',  ( 1.000000000000000000, 0.000000000000000000, -2.385244779468110248E-16 ) ) ;
#19752 = CARTESIAN_POINT ( 'NONE',  ( 95.54126587499996504, 81.68750000136559208, -1.387778780781445676E-14 ) ) ;
#19753 = CARTESIAN_POINT ( 'NONE',  ( 59.55508561352770158, 36.63437500108393152, -13.14518615778179900 ) ) ;
#19754 = EDGE_CURVE ( 'NONE', #2330, #16552, #2990, .T. ) ;
#19755 = CARTESIAN_POINT ( 'NONE',  ( 108.0825317500000153, 110.0000000000000000, -54.12500000273119838 ) ) ;
#19756 = CARTESIAN_POINT ( 'NONE',  ( -13.14518615778179189, 37.42812500108393436, 5.444914386472304635 ) ) ;
#19757 = CARTESIAN_POINT ( 'NONE',  ( 0.000000000000000000, 0.4999999999999970024, 0.000000000000000000 ) ) ;
#19758 = CARTESIAN_POINT ( 'NONE',  ( 116.4251840539369596, 36.23749999999999005, 0.000000000000000000 ) ) ;
#19759 = CARTESIAN_POINT ( 'NONE',  ( 103.5355339059327093, 82.62500000000000000, -3.535533905932755072 ) ) ;
#19760 = CARTESIAN_POINT ( 'NONE',  ( 135.6228728715778971, 36.48554687499999716, 13.57481594606304576 ) ) ;
#19761 = ORIENTED_EDGE ( 'NONE', *, *, #4466, .T. ) ;
#19762 = CARTESIAN_POINT ( 'NONE',  ( 2.493653234604083739E-15, 31.77265625216787370, 13.57481594606304576 ) ) ;
#19763 = CARTESIAN_POINT ( 'NONE',  ( -13.14518615778179189, 38.42031250108393436, 5.444914386472304635 ) ) ;
#19764 = CARTESIAN_POINT ( 'NONE',  ( 5.622872871577871301, 36.88242187716787157, -13.57481594606304753 ) ) ;
#19765 = CARTESIAN_POINT ( 'NONE',  ( 130.0000000000000000, 37.18007812608393436, -13.14518615778179544 ) ) ;
#19766 = EDGE_CURVE ( 'NONE', #7806, #3638, #1635, .T. ) ;
#19767 = CARTESIAN_POINT ( 'NONE',  ( 59.37712712842213136, 35.39414062716787157, -13.57481594606304753 ) ) ;
#19768 = EDGE_CURVE ( 'NONE', #22244, #27294, #3964, .T. ) ;
#19769 = ORIENTED_EDGE ( 'NONE', *, *, #7425, .F. ) ;
#19770 = CARTESIAN_POINT ( 'NONE',  ( 5.364947964715831574, 35.99999999999997158, 12.09311862596023701 ) ) ;
#19771 = CARTESIAN_POINT ( 'NONE',  ( -13.57481594606304753, 33.11210937716786873, -5.622872871577873077 ) ) ;
#19772 = ADVANCED_FACE ( 'NONE', ( #23212 ), #21069, .F. ) ;
#19773 = CARTESIAN_POINT ( 'NONE',  ( 104.9999999999999574, -2.071067811865462627, 1.437499999999999778 ) ) ;
#19774 = CARTESIAN_POINT ( 'NONE',  ( 93.46109445667489979, 114.7507929638356785, -48.07499999726882578 ) ) ;
#19775 = CARTESIAN_POINT ( 'NONE',  ( 185.7049497278729575, 34.30273437608393294, 9.295050272127047819 ) ) ;
#19776 = CARTESIAN_POINT ( 'NONE',  ( -9.598844408820458085, 33.85625000216787583, -9.598844408820458085 ) ) ;
#19777 = EDGE_CURVE ( 'NONE', #15169, #22062, #14821, .T. ) ;
#19778 =( NAMED_UNIT ( * ) SI_UNIT ( $, .STERADIAN. ) SOLID_ANGLE_UNIT ( ) );
#19780 = ORIENTED_EDGE ( 'NONE', *, *, #20172, .F. ) ;
#19779 = CARTESIAN_POINT ( 'NONE',  ( 195.0000000000000000, 38.81718749999999574, 13.57481594606304576 ) ) ;
#19781 = CARTESIAN_POINT ( 'NONE',  ( 104.9999999999999716, 1.449011120738813565E-14, 6.499999999999999112 ) ) ;
#19782 = CARTESIAN_POINT ( 'NONE',  ( -8.312177448680279460E-16, 36.03906250000000000, -13.57481594606304576 ) ) ;
#19783 = CARTESIAN_POINT ( 'NONE',  ( -13.57481594606304576, 37.08085937499999574, 5.622872871577880183 ) ) ;
#19784 =( BOUNDED_CURVE ( )  B_SPLINE_CURVE ( 2, ( #14217, #22654, #27218, #26936, #15927, #17937, #5552, #7380, #9527 ),
 .UNSPECIFIED., .F., .F. ) 
 B_SPLINE_CURVE_WITH_KNOTS ( ( 3, 2, 2, 2, 3 ),
 ( 0.05000000000000004441, 0.07500000000000006661, 0.1000000000000000888, 0.1250000000000001110, 0.1500000000000001332 ),
 .UNSPECIFIED. ) 
 CURVE ( )  GEOMETRIC_REPRESENTATION_ITEM ( )  RATIONAL_B_SPLINE_CURVE ( ( 0.9999999999999998890, 0.9238795325112868495, 1.000000000000000000, 0.9238795325112867385, 1.000000000000000000, 0.9238795325112867385, 1.000000000000000000, 0.9238795325112862944, 1.000000000000000444 ) ) 
 REPRESENTATION_ITEM ( '' )  );
#19785 = CARTESIAN_POINT ( 'NONE',  ( 105.6631189606246153, 114.1144967660473242, -45.80000000000001137 ) ) ;
#19786 = CARTESIAN_POINT ( 'NONE',  ( 5.444914386472297529, 38.12265625108393152, -13.14518615778179900 ) ) ;
#19787 = CARTESIAN_POINT ( 'NONE',  ( 9.295050272127046043, 35.49335937608393010, -9.295050272127046043 ) ) ;
#19788 = CARTESIAN_POINT ( 'NONE',  ( 208.5748159460630688, 35.04687499999999289, -1.662435489736055892E-15 ) ) ;
#19789 = DIRECTION ( 'NONE',  ( -0.000000000000000000, 1.000000000000000000, -0.000000000000000000 ) ) ;
#19790 = CYLINDRICAL_SURFACE ( 'NONE', #1499, 13.57481594606304576 ) ;
#19791 = CARTESIAN_POINT ( 'NONE',  ( 51.85481384221820633, 35.84062500108394289, 5.444914386472304635 ) ) ;
#19792 = CARTESIAN_POINT ( 'NONE',  ( 96.84719886470459471, -3.152801135295355994, 3.562500001365591196 ) ) ;
#19793 = CARTESIAN_POINT ( 'NONE',  ( 100.2089334463084072, 123.0000000000000142, -2.507929215363408293 ) ) ;
#19794 = DIRECTION ( 'NONE',  ( 0.000000000000000000, 0.000000000000000000, -1.000000000000000000 ) ) ;
#19795 = CARTESIAN_POINT ( 'NONE',  ( -5.622872871577873077, 36.38632812499999858, 13.57481594606304753 ) ) ;
#19796 = CARTESIAN_POINT ( 'NONE',  ( 143.1451861577818079, 36.33671875108394289, 5.444914386472293977 ) ) ;
#19797 = EDGE_LOOP ( 'NONE', ( #26617, #26809, #23116, #4006 ) ) ;
#19798 = ORIENTED_EDGE ( 'NONE', *, *, #19414, .T. ) ;
#19799 = CARTESIAN_POINT ( 'NONE',  ( 95.54126587499995082, 80.62500000136559208, -1.846868145590750077 ) ) ;
#19800 = VECTOR ( 'NONE', #18890, 1000.000000000000000 ) ;
#19801 = CARTESIAN_POINT ( 'NONE',  ( 102.0710678118654329, 80.43750000273119838, 4.999999999999989342 ) ) ;
#19802 = CARTESIAN_POINT ( 'NONE',  ( 97.92893218813452449, 90.31250000000001421, -4.999999999999997335 ) ) ;
#19803 = CARTESIAN_POINT ( 'NONE',  ( 51.89752917827804168, 36.00000000000001421, -1.608626461598229085 ) ) ;
#19804 = ADVANCED_FACE ( 'NONE', ( #240 ), #2248, .F. ) ;
#19805 = CARTESIAN_POINT ( 'NONE',  ( 93.00000000000000000, 107.7255621263696526, -52.90000000000001990 ) ) ;
#19806 = CARTESIAN_POINT ( 'NONE',  ( 59.55508561352770158, 32.96328125108393436, 13.14518615778179722 ) ) ;
#19807 = EDGE_LOOP ( 'NONE', ( #10127, #6003, #21592, #12987 ) ) ;
#19808 = DIRECTION ( 'NONE',  ( 0.000000000000000000, 0.000000000000000000, 1.000000000000000000 ) ) ;
#19809 = ADVANCED_FACE ( 'NONE', ( #1964 ), #8926, .F. ) ;
#19810 = CARTESIAN_POINT ( 'NONE',  ( 99.99999999999995737, 4.458734125000016313, 3.437500001365592972 ) ) ;
#19811 = VERTEX_POINT ( 'NONE', #10769 ) ;
#19812 = CARTESIAN_POINT ( 'NONE',  ( -5.444914386472299306, 32.96328125108393436, 13.14518615778179722 ) ) ;
#19813 = CARTESIAN_POINT ( 'NONE',  ( -9.295050272127044266, 40.05742187608393579, 9.295050272127047819 ) ) ;
#19814 = UNCERTAINTY_MEASURE_WITH_UNIT (LENGTH_MEASURE( 1.000000000000000082E-05 ), #13163, 'distance_accuracy_value', 'NONE');
#19815 = CARTESIAN_POINT ( 'NONE',  ( 185.4011555911795313, 35.44375000216787441, -9.598844408820458085 ) ) ;
#19816 = ORIENTED_EDGE ( 'NONE', *, *, #6824, .F. ) ;
#19817 = CARTESIAN_POINT ( 'NONE',  ( 5.444914386472297529, 36.33671875108393579, -13.14518615778179722 ) ) ;
#19818 = CARTESIAN_POINT ( 'NONE',  ( 2.493653234604083739E-15, 36.53515625216787299, 13.57481594606304576 ) ) ;
#19819 = CARTESIAN_POINT ( 'NONE',  ( 143.1451861577818079, 37.18007812608393436, -1.609821015232357215E-15 ) ) ;
#19820 = CARTESIAN_POINT ( 'NONE',  ( -9.295050272127046043, 35.09648437608393579, -9.295050272127046043 ) ) ;
#19821 = CARTESIAN_POINT ( 'NONE',  ( 143.1451861577818079, 36.13828125108393863, 5.444914386472293977 ) ) ;
#19822 = CARTESIAN_POINT ( 'NONE',  ( 78.57481594606304043, 35.79101562499999289, 5.622872871577869525 ) ) ;
#19823 = CARTESIAN_POINT ( 'NONE',  ( -8.312177448680279460E-16, 34.45156249999999432, -13.57481594606304576 ) ) ;
#19824 = CARTESIAN_POINT ( 'NONE',  ( 99.99999999999995737, 4.458734125000016313, 10.43750000136559208 ) ) ;
#19825 = DIRECTION ( 'NONE',  ( -0.000000000000000000, 1.000000000000000000, -0.000000000000000000 ) ) ;
#19826 = CARTESIAN_POINT ( 'NONE',  ( 102.0710678118654329, 5.000000000000018652, 3.812500002731185056 ) ) ;
#19827 = CARTESIAN_POINT ( 'NONE',  ( 0.000000000000000000, 40.99999999999999289, -13.57481594606304576 ) ) ;
#19828 = AXIS2_PLACEMENT_3D ( 'NONE', #11345, #11628, #22637 ) ;
#19829 = CARTESIAN_POINT ( 'NONE',  ( 0.000000000000000000, 1.500000000000001332, 24.13397459621556607 ) ) ;
#19830 = CARTESIAN_POINT ( 'NONE',  ( 93.46109445667489979, 114.7507929638356785, -47.82499999726882578 ) ) ;
#19831 = CARTESIAN_POINT ( 'NONE',  ( 9.295050272127046043, 38.07304687608393579, -9.295050272127046043 ) ) ;
#19832 = CARTESIAN_POINT ( 'NONE',  ( 95.00472066334982912, 116.8754121666685393, -52.17499999726881299 ) ) ;
#19833 = ORIENTED_EDGE ( 'NONE', *, *, #16267, .T. ) ;
#19834 = CARTESIAN_POINT ( 'NONE',  ( 93.00000000000000000, 110.0000000000000000, -50.50000000546237544 ) ) ;
#19835 = CARTESIAN_POINT ( 'NONE',  ( 104.9999999999999858, -2.071067811865457298, 12.56250000273118594 ) ) ;
#19836 = CARTESIAN_POINT ( 'NONE',  ( 99.99999999999998579, 136.0000000000000000, -10.50000000000002132 ) ) ;
#19837 =( BOUNDED_CURVE ( )  B_SPLINE_CURVE ( 2, ( #18608, #7770, #18179, #24882, #18326, #22752, #13884, #664, #18031 ),
 .UNSPECIFIED., .F., .F. ) 
 B_SPLINE_CURVE_WITH_KNOTS ( ( 3, 2, 2, 2, 3 ),
 ( 0.4791666666666667962, 0.4895833333333333703, 0.5000000000000000000, 0.5104166666666665186, 0.5208333333333332593 ),
 .UNSPECIFIED. ) 
 CURVE ( )  GEOMETRIC_REPRESENTATION_ITEM ( )  RATIONAL_B_SPLINE_CURVE ( ( 0.9999999999999992228, 0.9238795325112875156, 1.000000000000000000, 0.9238795325112867385, 1.000000000000000000, 0.9238795325112867385, 1.000000000000000000, 0.9238795325112875156, 0.9999999999999992228 ) ) 
 REPRESENTATION_ITEM ( '' )  );
#19838 = CARTESIAN_POINT ( 'NONE',  ( 208.1451861577818079, 39.36289062608393152, -1.609821015232357215E-15 ) ) ;
#19839 = VERTEX_POINT ( 'NONE', #24041 ) ;
#19840 = CARTESIAN_POINT ( 'NONE',  ( 9.598844408820456309, 40.00781250216787299, -9.598844408820458085 ) ) ;
#19841 = CARTESIAN_POINT ( 'NONE',  ( 104.4587341249999639, 1.442382525525748735E-14, 13.18750000136559208 ) ) ;
#19842 = ORIENTED_EDGE ( 'NONE', *, *, #14023, .T. ) ;
#19843 = CARTESIAN_POINT ( 'NONE',  ( 97.50236033167492167, 117.6869444889999841, -51.77500000273119696 ) ) ;
#19844 = CARTESIAN_POINT ( 'NONE',  ( 5.444914386472297529, 38.71796875108393721, -13.14518615778179900 ) ) ;
#19845 = VECTOR ( 'NONE', #24147, 1000.000000000000000 ) ;
#19846 = CARTESIAN_POINT ( 'NONE',  ( 101.7677669529663547, 123.7000000000000028, 1.767766952966350891 ) ) ;
#19847 = CARTESIAN_POINT ( 'NONE',  ( 143.5748159460630688, 31.97109375216787441, -1.662435489736055892E-15 ) ) ;
#19848 = DIRECTION ( 'NONE',  ( 1.000000000000000000, 0.000000000000000000, 0.000000000000000000 ) ) ;
#19849 = CARTESIAN_POINT ( 'NONE',  ( 95.00000000000000000, 94.43749999726878741, 2.071067811865463959 ) ) ;
#19850 = CARTESIAN_POINT ( 'NONE',  ( 65.00000000000000000, 36.58476562608393579, -13.14518615778179544 ) ) ;
#19851 = CARTESIAN_POINT ( 'NONE',  ( 66.13876811710015602, 50.00000000043813486, -13.56816686242498982 ) ) ;
#19852 = CARTESIAN_POINT ( 'NONE',  ( 195.0000000000000000, 40.80156249999999574, -13.57481594606304576 ) ) ;
#19853 = CARTESIAN_POINT ( 'NONE',  ( 75.56308295035979938, 36.00000000000000000, 8.196709705857863071 ) ) ;
#19854 = ORIENTED_EDGE ( 'NONE', *, *, #6701, .F. ) ;
#19855 = ORIENTED_EDGE ( 'NONE', *, *, #1318, .F. ) ;
#19856 = CARTESIAN_POINT ( 'NONE',  ( 5.444914386472302859, 40.20625000108394431, 13.14518615778179189 ) ) ;
#19857 = PRODUCT_CONTEXT ( 'NONE', #4974, 'mechanical' ) ;
#19858 = CARTESIAN_POINT ( 'NONE',  ( 104.4587341249999781, -1.846868145590721655, 9.125000001365592084 ) ) ;
#19859 = CARTESIAN_POINT ( 'NONE',  ( 59.55508561352770158, 39.90859375108392726, 13.14518615778179722 ) ) ;
#19860 = CARTESIAN_POINT ( 'NONE',  ( 65.00000000000000000, 36.53515625216787299, 13.57481594606304576 ) ) ;
#19861 = CARTESIAN_POINT ( 'NONE',  ( 195.0000000000000000, 39.16445312608392726, 13.14518615778179544 ) ) ;
#19862 = CARTESIAN_POINT ( 'NONE',  ( -5.444914386472299306, 37.72578125108394431, 13.14518615778179722 ) ) ;
#19863 = CARTESIAN_POINT ( 'NONE',  ( 185.8198241863519797, 50.00000000000000711, 14.99999999999995204 ) ) ;
#19864 = AXIS2_PLACEMENT_3D ( 'NONE', #22444, #3761, #6172 ) ;
#19865 = CARTESIAN_POINT ( 'NONE',  ( 0.000000000000000000, 80.00000000000000000, 0.000000000000000000 ) ) ;
#19866 = CARTESIAN_POINT ( 'NONE',  ( 70.62287287157774074, 39.66054687500000142, 13.57481594606318076 ) ) ;
#19867 = CARTESIAN_POINT ( 'NONE',  ( 95.00472066334982912, 116.8754121666685393, -49.92499999726880588 ) ) ;
#19868 = ORIENTED_EDGE ( 'NONE', *, *, #7208, .T. ) ;
#19869 = EDGE_LOOP ( 'NONE', ( #25743, #17375, #14231, #21422, #20238, #21760 ) ) ;
#19870 = CARTESIAN_POINT ( 'NONE',  ( -9.598844408820454532, 37.92421874999999432, 9.598844408820459861 ) ) ;
#19871 = CARTESIAN_POINT ( 'NONE',  ( -13.14518615778179544, 37.37851562608393863, 0.000000000000000000 ) ) ;
#19872 = VERTEX_POINT ( 'NONE', #13175 ) ;
#19873 = CARTESIAN_POINT ( 'NONE',  ( 116.8548138422182063, 32.86406250108393579, 5.444914386472304635 ) ) ;
#19874 = CARTESIAN_POINT ( 'NONE',  ( 78.14518615778179367, 34.65000000108393152, -5.444914386472297529 ) ) ;
#19875 = CARTESIAN_POINT ( 'NONE',  ( 204.2950502721270425, 38.86679687608393863, -9.295050272127046043 ) ) ;
#19876 = VERTEX_POINT ( 'NONE', #28042 ) ;
#19877 = CARTESIAN_POINT ( 'NONE',  ( 99.99999999999995737, 1.387778780781445676E-14, 34.79898987322334136 ) ) ;
#19878 = SHAPE_REPRESENTATION ( 'suction cup mounting thread', ( #26844 ), #9975 ) ;
#19879 = CARTESIAN_POINT ( 'NONE',  ( 13.14518615778179900, 32.16953125108393152, 5.444914386472293977 ) ) ;
#19880 = CARTESIAN_POINT ( 'NONE',  ( 96.46446609406721961, -3.535533905932727539, 1.250000002731184390 ) ) ;
#19881 = AXIS2_PLACEMENT_3D ( 'NONE', #14142, #11716, #5049 ) ;
#19882 = CARTESIAN_POINT ( 'NONE',  ( -8.312177448680279460E-16, 32.96328125216787441, -13.57481594606304576 ) ) ;
#19883 = CARTESIAN_POINT ( 'NONE',  ( 139.5988444088204687, 39.80937500216786873, 9.598844408820456309 ) ) ;
#19884 = CARTESIAN_POINT ( 'NONE',  ( 99.99999999999998579, 124.7999999999999972, -2.499999999999997780 ) ) ;
#19885 = DIRECTION ( 'NONE',  ( -0.000000000000000000, -0.000000000000000000, -1.000000000000000000 ) ) ;
#19886 = CARTESIAN_POINT ( 'NONE',  ( 0.000000000000000000, 29.95886589889650509, 11.57481594606304576 ) ) ;
#19887 = CARTESIAN_POINT ( 'NONE',  ( 56.73140267161080885, 50.00000000054374993, 10.78867689284317066 ) ) ;
#19888 = PRODUCT_RELATED_PRODUCT_CATEGORY ( 'part', '', ( #11245 ) ) ;
#19889 = EDGE_CURVE ( 'NONE', #444, #10089, #22134, .T. ) ;
#19890 = FILL_AREA_STYLE ('',( #24735 ) ) ;
#19891 = CARTESIAN_POINT ( 'NONE',  ( 101.8468681455906903, -4.458734124999987891, 7.750000001365592084 ) ) ;
#19892 = ORIENTED_EDGE ( 'NONE', *, *, #13459, .T. ) ;
#19893 = CARTESIAN_POINT ( 'NONE',  ( 99.99999999999998579, 122.5000000021849615, -2.499999999999997780 ) ) ;
#19894 = CARTESIAN_POINT ( 'NONE',  ( 99.99999999999995737, -4.458734124999988779, 8.687500001365592084 ) ) ;
#19895 = CARTESIAN_POINT ( 'NONE',  ( 127.8300434168938580, 49.99999999883939950, 13.43548448457867828 ) ) ;
#19896 = CARTESIAN_POINT ( 'NONE',  ( -5.444914386472299306, 39.11484375108394573, 13.14518615778179722 ) ) ;
#19897 = CARTESIAN_POINT ( 'NONE',  ( 219.9999999999999716, 55.00000000000000000, 14.99999999999994316 ) ) ;
#19898 = CARTESIAN_POINT ( 'NONE',  ( 101.8468681455906903, 82.37500000136562051, -4.458734125000016313 ) ) ;
#19899 = CARTESIAN_POINT ( 'NONE',  ( 78.14518615778179367, 36.38632812608393863, -1.609821015232357215E-15 ) ) ;
#19900 = CARTESIAN_POINT ( 'NONE',  ( 106.5389055433251002, 114.7507929638356785, -53.92500000273119554 ) ) ;
#19901 = CARTESIAN_POINT ( 'NONE',  ( 5.444914386472297529, 36.33671875108393579, -13.14518615778179722 ) ) ;
#19902 = ADVANCED_BREP_SHAPE_REPRESENTATION ( '', ( #17619, #26844 ), #4064 ) ;
#19903 = AXIS2_PLACEMENT_3D ( 'NONE', #14884, #14473, #21468 ) ;
#19904 = CARTESIAN_POINT ( 'NONE',  ( 114.9999999999999858, 120.0000000000000000, -15.00000000000000711 ) ) ;
#19905 = CARTESIAN_POINT ( 'NONE',  ( 102.0710678118654329, -4.999999999999989342, 11.43750000273118772 ) ) ;
#19906 = CARTESIAN_POINT ( 'NONE',  ( 102.1631189606246153, 116.6573956140660897, -49.60000000000001563 ) ) ;
#19907 = CARTESIAN_POINT ( 'NONE',  ( 120.4011555911795455, 38.51953124999999289, -9.598844408820458085 ) ) ;
#19908 = VERTEX_POINT ( 'NONE', #19338 ) ;
#19909 = ORIENTED_EDGE ( 'NONE', *, *, #22744, .T. ) ;
#19910 = CARTESIAN_POINT ( 'NONE',  ( -8.312177448680279460E-16, 40.10703125216787157, -13.57481594606304576 ) ) ;
#19911 = CARTESIAN_POINT ( 'NONE',  ( 9.295050272127047819, 37.08085937608393579, 9.295050272127046043 ) ) ;
#19912 = CARTESIAN_POINT ( 'NONE',  ( -9.598844408820454532, 36.43593750216787441, 9.598844408820459861 ) ) ;
#19913 = CARTESIAN_POINT ( 'NONE',  ( 103.5355339059327093, 3.535533905932755072, 10.75000000273118594 ) ) ;
#19914 = CARTESIAN_POINT ( 'NONE',  ( 143.1451861577818079, 35.39414062608393152, -1.609821015232357215E-15 ) ) ;
#19915 = CARTESIAN_POINT ( 'NONE',  ( 51.42518405393695957, 33.21132812716787441, 5.622872871577880183 ) ) ;
#19916 = CARTESIAN_POINT ( 'NONE',  ( 7.754123975995396378, 35.99999999999999289, 10.77549638133713472 ) ) ;
#19917 = CARTESIAN_POINT ( 'NONE',  ( 5.622872871577878406, 32.61601562716786873, 13.57481594606304576 ) ) ;
#19918 = CARTESIAN_POINT ( 'NONE',  ( 94.99999999999995737, 2.071067811865491048, 1.937500000000000000 ) ) ;
#19919 = CARTESIAN_POINT ( 'NONE',  ( 95.00472066334981491, 116.8754121666685393, -46.17499999726882720 ) ) ;
#19920 = ADVANCED_FACE ( 'NONE', ( #15180 ), #17192, .F. ) ;
#19921 = CARTESIAN_POINT ( 'NONE',  ( 181.8548138422181921, 34.94765625108392726, -5.444914386472297529 ) ) ;
#19922 = DIRECTION ( 'NONE',  ( -0.000000000000000000, -1.000000000000000000, -0.000000000000000000 ) ) ;
#19923 = CARTESIAN_POINT ( 'NONE',  ( 99.99999999999995737, 81.75000000000000000, -5.000000000000018652 ) ) ;
#19924 = ORIENTED_EDGE ( 'NONE', *, *, #20278, .T. ) ;
#19925 = CARTESIAN_POINT ( 'NONE',  ( 189.3771271284221029, 40.35507812499999147, 13.57481594606302444 ) ) ;
#19926 = CARTESIAN_POINT ( 'NONE',  ( 120.4011555911795455, 36.23750000216787726, -9.598844408820458085 ) ) ;
#19927 = CARTESIAN_POINT ( 'NONE',  ( -8.312177448680279460E-16, 32.16953125216787157, -13.57481594606304576 ) ) ;
#19928 = CARTESIAN_POINT ( 'NONE',  ( 9.598844408820456309, 35.93984374999999432, -9.598844408820458085 ) ) ;
#19929 = CARTESIAN_POINT ( 'NONE',  ( 99.99999999999997158, 117.3602355696678643, -45.50000000000001421 ) ) ;
#19930 = CARTESIAN_POINT ( 'NONE',  ( 5.444914386472302859, 37.03125000108393294, 13.14518615778179189 ) ) ;
#19931 = CARTESIAN_POINT ( 'NONE',  ( -5.444914386472299306, 37.52734375108393294, 13.14518615778179722 ) ) ;
#19932 = EDGE_CURVE ( 'NONE', #21429, #12537, #25300, .T. ) ;
#19933 = CARTESIAN_POINT ( 'NONE',  ( 189.3771271284221314, 33.21132812499999432, 13.57481594606304753 ) ) ;
#19934 = CONTEXT_DEPENDENT_SHAPE_REPRESENTATION ( #25190, #21023 ) ;
#19935 = CARTESIAN_POINT ( 'NONE',  ( 59.37712712842210294, 40.35507812499999147, 13.57481594606302444 ) ) ;
#19936 = DIRECTION ( 'NONE',  ( -0.000000000000000000, -1.000000000000000000, -0.000000000000000000 ) ) ;
#19937 = CARTESIAN_POINT ( 'NONE',  ( 65.00000000000000000, 36.38632812608393152, -13.14518615778179544 ) ) ;
#19938 = ADVANCED_FACE ( 'NONE', ( #23899 ), #15616, .T. ) ;
#19939 = CARTESIAN_POINT ( 'NONE',  ( 101.8468681455907046, 4.458734125000016313, 4.125000001365592084 ) ) ;
#19940 = CARTESIAN_POINT ( 'NONE',  ( 97.53586499902618812, 122.9999999999999716, 0.4483706153950356987 ) ) ;
#19941 = LINE ( 'NONE', #6537, #721 ) ;
#19942 = CARTESIAN_POINT ( 'NONE',  ( -9.598844408820454532, 36.33671874999999574, 9.598844408820459861 ) ) ;
#19943 = CARTESIAN_POINT ( 'NONE',  ( 135.4449143864723055, 38.91640625108393436, -13.14518615778179900 ) ) ;
#19944 = EDGE_CURVE ( 'NONE', #16728, #19746, #19628, .T. ) ;
#19945 = VERTEX_POINT ( 'NONE', #6641 ) ;
#19946 = CARTESIAN_POINT ( 'NONE',  ( 99.99999999999995737, 82.75000000000000000, -5.000000000000018652 ) ) ;
#19947 = LINE ( 'NONE', #425, #23034 ) ;
#19948 = CARTESIAN_POINT ( 'NONE',  ( 99.99999999999995737, 83.87500000273119838, -5.000000000000018652 ) ) ;
#19949 = CARTESIAN_POINT ( 'NONE',  ( 104.4587341249999781, 92.31249999863440792, -6.938893903907228378E-15 ) ) ;
#19950 = DIRECTION ( 'NONE',  ( 0.000000000000000000, 0.000000000000000000, 1.000000000000000000 ) ) ;
#19951 = VECTOR ( 'NONE', #20859, 1000.000000000000000 ) ;
#19952 = EDGE_CURVE ( 'NONE', #25694, #17550, #11048, .T. ) ;
#19953 = CARTESIAN_POINT ( 'NONE',  ( 107.0000000000000000, 107.7255621263696668, -48.10000000000000142 ) ) ;
#19954 = CARTESIAN_POINT ( 'NONE',  ( 59.55508561352770158, 31.87187500108393223, -13.14518615778179900 ) ) ;
#19955 = PRODUCT_DEFINITION_FORMATION_WITH_SPECIFIED_SOURCE ( 'ANY', '', #20393, .NOT_KNOWN. ) ;
#19956 = ORIENTED_EDGE ( 'NONE', *, *, #19075, .F. ) ;
#19957 = LINE ( 'NONE', #20239, #22256 ) ;
#19958 = CARTESIAN_POINT ( 'NONE',  ( 97.92893218813451028, -4.999999999999989342, 13.18749999999999822 ) ) ;
#19959 = ORIENTED_EDGE ( 'NONE', *, *, #17331, .F. ) ;
#19960 = CARTESIAN_POINT ( 'NONE',  ( -9.295050272127046043, 36.68398437608393436, -9.295050272127046043 ) ) ;
#19961 = CARTESIAN_POINT ( 'NONE',  ( 181.4251840539369596, 34.69960937716787441, -5.622872871577873077 ) ) ;
#19962 =( BOUNDED_CURVE ( )  B_SPLINE_CURVE ( 2, ( #25105, #26835, #9849, #12110, #11546, #16409, #14116, #18556, #20838 ),
 .UNSPECIFIED., .F., .T. ) 
 B_SPLINE_CURVE_WITH_KNOTS ( ( 3, 2, 2, 2, 3 ),
 ( 0.3125000000000002220, 0.3229166666666668517, 0.3333333333333334259, 0.3437500000000000555, 0.3541666666666666852 ),
 .UNSPECIFIED. ) 
 CURVE ( )  GEOMETRIC_REPRESENTATION_ITEM ( )  RATIONAL_B_SPLINE_CURVE ( ( 0.9999999999999983347, 0.9238795325112884038, 1.000000000000000000, 0.9238795325112867385, 1.000000000000000000, 0.9238795325112867385, 1.000000000000000000, 0.9238795325112867385, 1.000000000000000000 ) ) 
 REPRESENTATION_ITEM ( '' )  );
#19963 = CARTESIAN_POINT ( 'NONE',  ( 13.14518615778179722, 33.06250000108393294, -5.444914386472297529 ) ) ;
#19964 = CARTESIAN_POINT ( 'NONE',  ( -8.312177448680279460E-16, 40.80156249999999574, -13.57481594606304576 ) ) ;
#19965 = EDGE_CURVE ( 'NONE', #11839, #8168, #11185, .T. ) ;
#19966 = CARTESIAN_POINT ( 'NONE',  ( 124.5550856135277087, 37.72578125108394431, 13.14518615778179722 ) ) ;
#19967 = CARTESIAN_POINT ( 'NONE',  ( 5.444914386472302859, 34.65000000108393863, 13.14518615778179189 ) ) ;
#19968 = CARTESIAN_POINT ( 'NONE',  ( 124.5550856135277087, 32.76484375108393010, 13.14518615778179722 ) ) ;
#19969 = CARTESIAN_POINT ( 'NONE',  ( 70.62287287157786864, 35.19570312499999432, -13.57481594606304753 ) ) ;
#19970 = DIRECTION ( 'NONE',  ( -0.000000000000000000, -1.000000000000000000, -0.000000000000000000 ) ) ;
#19971 = AXIS2_PLACEMENT_3D ( 'NONE', #19202, #3549, #25615 ) ;
#19972 = VECTOR ( 'NONE', #24869, 1000.000000000000000 ) ;
#19973 = CARTESIAN_POINT ( 'NONE',  ( 98.15313185440925281, 4.458734125000016313, 11.50000000136559208 ) ) ;
#19974 = DIRECTION ( 'NONE',  ( -1.000000000000000000, 0.000000000000000000, 7.228014483236696740E-18 ) ) ;
#19975 = CARTESIAN_POINT ( 'NONE',  ( 99.99999999999995737, 4.458734125000016313, 1.187500001365592750 ) ) ;
#19976 = CARTESIAN_POINT ( 'NONE',  ( 102.4976396683250925, 117.6869444889999841, -47.72500000273119269 ) ) ;
#19977 = VECTOR ( 'NONE', #7839, 1000.000000000000000 ) ;
#19978 = CARTESIAN_POINT ( 'NONE',  ( 104.9999999999999716, 1.449011120738813565E-14, 12.62500000273118594 ) ) ;
#19979 = CARTESIAN_POINT ( 'NONE',  ( 65.00000000000000000, 50.00000000000000000, -7.517135062566165128E-15 ) ) ;
#19980 = CARTESIAN_POINT ( 'NONE',  ( 91.91746824999998466, 110.0000000000000000, -49.62499999726882294 ) ) ;
#19981 = CARTESIAN_POINT ( 'NONE',  ( 13.14518615778179544, 35.59257812608393579, -1.609821015232357215E-15 ) ) ;
#19982 = EDGE_CURVE ( 'NONE', #2100, #12289, #6716, .T. ) ;
#19983 = CARTESIAN_POINT ( 'NONE',  ( 93.00000000000000000, 107.7255621263696526, -48.39999999453763024 ) ) ;
#19984 = VERTEX_POINT ( 'NONE', #21770 ) ;
#19985 = CARTESIAN_POINT ( 'NONE',  ( 99.14382582708708469, 124.6000000010924822, -2.066987299999998751 ) ) ;
#19986 = CARTESIAN_POINT ( 'NONE',  ( 102.0669873000000081, 122.6000000010924822, -0.8561741729129508371 ) ) ;
#19987 = CYLINDRICAL_SURFACE ( 'NONE', #11213, 13.57481594606304576 ) ;
#19988 = CARTESIAN_POINT ( 'NONE',  ( 189.5550856135277229, 36.43593750108392726, -13.14518615778179900 ) ) ;
#19989 = VERTEX_POINT ( 'NONE', #20189 ) ;
#19990 = CARTESIAN_POINT ( 'NONE',  ( 105.6631189606246153, 114.1144967660473242, -49.29999999453763593 ) ) ;
#19991 = CARTESIAN_POINT ( 'NONE',  ( 95.54126587499995082, -1.846868145590724986, 10.75000000136559208 ) ) ;
#19992 = ORIENTED_EDGE ( 'NONE', *, *, #12726, .F. ) ;
#19993 = CARTESIAN_POINT ( 'NONE',  ( 107.0000000000000142, 110.0000000000000000, -45.00000000000000711 ) ) ;
#19994 = CARTESIAN_POINT ( 'NONE',  ( -9.295050272127044266, 39.85898437608393152, 9.295050272127047819 ) ) ;
#19995 = PRESENTATION_LAYER_ASSIGNMENT (  '', '', ( #14962 ) ) ;
#19996 = CARTESIAN_POINT ( 'NONE',  ( 98.96446609406727646, 123.2500000000000000, -2.499999999999997780 ) ) ;
#19997 = VECTOR ( 'NONE', #11258, 1000.000000000000000 ) ;
#19998 = CARTESIAN_POINT ( 'NONE',  ( 143.5748159460630404, 32.02070312716787015, -5.622872871577873077 ) ) ;
#19999 = DIRECTION ( 'NONE',  ( 0.000000000000000000, 0.000000000000000000, 1.000000000000000000 ) ) ;
#20000 = CARTESIAN_POINT ( 'NONE',  ( 102.0710678118654613, 94.68749999726883004, 4.999999999999983125 ) ) ;
#20001 = CARTESIAN_POINT ( 'NONE',  ( 59.55508561352770158, 36.63437500108393152, -13.14518615778179900 ) ) ;
#20002 = CARTESIAN_POINT ( 'NONE',  ( 73.75833439235653088, 50.00000000000000000, -10.38725784494184445 ) ) ;
#20003 = CARTESIAN_POINT ( 'NONE',  ( 106.5389055433251002, 114.7507929638356785, -54.17500000273119554 ) ) ;
#20004 = CARTESIAN_POINT ( 'NONE',  ( 181.8548138422182205, 32.02070312608393010, 0.000000000000000000 ) ) ;
#20005 = ADVANCED_FACE ( 'NONE', ( #27041 ), #13892, .T. ) ;
#20006 = FACE_OUTER_BOUND ( 'NONE', #15743, .T. ) ;
#20007 = EDGE_LOOP ( 'NONE', ( #11119, #12636, #18620, #25305, #9323, #6868, #24517, #9491, #21123, #7238, #14709, #8789, #7611, #22855, #26709, #17003, #9463, #14950, #11598, #10214, #19992, #19553, #15279, #18129, #17235, #4913, #14681, #26687, #10087, #2705, #20091 ) ) ;
#20008 = CARTESIAN_POINT ( 'NONE',  ( 5.444914386472302859, 36.23750000108393721, 13.14518615778179189 ) ) ;
#20009 = CARTESIAN_POINT ( 'NONE',  ( 99.99999999999995737, -4.458734124999988779, 11.93750000136559208 ) ) ;
#20010 = FACE_OUTER_BOUND ( 'NONE', #857, .T. ) ;
#20011 = CARTESIAN_POINT ( 'NONE',  ( 84.99999999999998579, 95.00000000000000000, -15.00000000000000533 ) ) ;
#20012 = CARTESIAN_POINT ( 'NONE',  ( 208.1451861577818079, 39.36289062608393152, -1.609821015232357215E-15 ) ) ;
#20013 = ORIENTED_EDGE ( 'NONE', *, *, #5180, .F. ) ;
#20014 = CARTESIAN_POINT ( 'NONE',  ( -13.14518615778179544, 37.57695312608393579, 0.000000000000000000 ) ) ;
#20015 =( BOUNDED_SURFACE ( )  B_SPLINE_SURFACE ( 1, 2, ( 
 ( #3159, #11829, #20120, #26830, #27113, #11401, #24680, #7563, #22262, #16111, #13964, #598, #16257, #24957, #9278, #892, #14110, #20406, #17974, #7416, #9562, #26682, #7130, #22834, #5157, #3300, #9416, #18265, #15827, #5018, #11540, #13683, #22400, #24816, #5299, #27801, #10106, #18687, #27526, #3721, #1306, #14659, #3996, #7982, #27390, #12659, #21101, #1176, #8257, #7849, #5725, #9841, #3852, #14529, #12383, #20967, #25379, #25645, #1723, #12513, #23244, #18548, #27252, #16944, #1589, #9976, #14390, #10244, #27661, #14251, #16544, #25101, #23380, #21241, #18819, #16680, #25234, #7710, #12102, #20829, #3581 ),
 ( #23107, #1450, #8123, #16403, #5586, #10385, #22972, #5859, #16818, #18952, #25515, #12239, #5994, #19092, #6129, #14794, #23517, #3436, #12928, #26067, #26211, #21660, #6673, #10801, #28074, #2282, #4945, #26751, #17371, #25930, #9343, #10663, #13607, #24606, #23657, #11467, #20186, #8681, #670, #1996, #27935, #5084, #6536, #22329, #18038, #19371, #19514, #2136, #15214, #8539, #21385, #15359, #23933, #17225, #10940, #4412, #7193, #13067, #6405, #15890, #15074, #2800, #1863, #4133, #10528, #19234, #21804, #8394, #23792, #17083, #25785, #19652, #6263, #14936, #4269, #134, #8820, #17509, #24074, #12797, #21517 ) ),
 .UNSPECIFIED., .F., .F., .F. ) 
 B_SPLINE_SURFACE_WITH_KNOTS ( ( 2, 2 ),
 ( 3, 2, 2, 2, 2, 2, 2, 2, 2, 2, 2, 2, 2, 2, 2, 2, 2, 2, 2, 2, 2, 2, 2, 2, 2, 2, 2, 2, 2, 2, 2, 2, 2, 2, 2, 2, 2, 2, 2, 2, 3 ),
 ( 0.000000000000000000, 1.000000000000000000 ),
 ( 0.000000000000000000, 0.02500000000000000139, 0.05000000000000000278, 0.07499999999999999722, 0.1000000000000000056, 0.1250000000000000000, 0.1499999999999999944, 0.1749999999999999889, 0.2000000000000000111, 0.2250000000000000056, 0.2500000000000000000, 0.2750000000000000222, 0.2999999999999999889, 0.3250000000000000111, 0.3499999999999999778, 0.3750000000000000000, 0.4000000000000000222, 0.4249999999999999889, 0.4500000000000000111, 0.4749999999999999778, 0.5000000000000000000, 0.5250000000000000222, 0.5500000000000000444, 0.5749999999999999556, 0.5999999999999999778, 0.6250000000000000000, 0.6500000000000000222, 0.6750000000000000444, 0.6999999999999999556, 0.7249999999999999778, 0.7500000000000000000, 0.7750000000000000222, 0.8000000000000000444, 0.8249999999999999556, 0.8499999999999999778, 0.8750000000000000000, 0.9000000000000000222, 0.9250000000000000444, 0.9499999999999999556, 0.9749999999999999778, 1.000000000000000000 ),
 .UNSPECIFIED. ) 
 GEOMETRIC_REPRESENTATION_ITEM ( )  RATIONAL_B_SPLINE_SURFACE ( (
 ( 1.000000000000000000, 0.9238795325112867385, 1.000000000000000000, 0.9238795325112867385, 1.000000000000000000, 0.9238795325112867385, 1.000000000000000000, 0.9238795325112867385, 1.000000000000000000, 0.9238795325112867385, 1.000000000000000000, 0.9238795325112867385, 1.000000000000000000, 0.9238795325112867385, 1.000000000000000000, 0.9238795325112867385, 1.000000000000000000, 0.9238795325112867385, 1.000000000000000000, 0.9238795325112867385, 1.000000000000000000, 0.9238795325112867385, 1.000000000000000000, 0.9238795325112867385, 1.000000000000000000, 0.9238795325112867385, 1.000000000000000000, 0.9238795325112867385, 1.000000000000000000, 0.9238795325112867385, 1.000000000000000000, 0.9238795325112867385, 1.000000000000000000, 0.9238795325112867385, 1.000000000000000000, 0.9238795325112867385, 1.000000000000000000, 0.9238795325112867385, 1.000000000000000000, 0.9238795325112867385, 1.000000000000000000, 0.9238795325112867385, 1.000000000000000000, 0.9238795325112867385, 1.000000000000000000, 0.9238795325112867385, 1.000000000000000000, 0.9238795325112867385, 1.000000000000000000, 0.9238795325112867385, 1.000000000000000000, 0.9238795325112867385, 1.000000000000000000, 0.9238795325112867385, 1.000000000000000000, 0.9238795325112867385, 1.000000000000000000, 0.9238795325112867385, 1.000000000000000000, 0.9238795325112867385, 1.000000000000000000, 0.9238795325112867385, 1.000000000000000000, 0.9238795325112867385, 1.000000000000000000, 0.9238795325112867385, 1.000000000000000000, 0.9238795325112867385, 1.000000000000000000, 0.9238795325112867385, 1.000000000000000000, 0.9238795325112867385, 1.000000000000000000, 0.9238795325112867385, 1.000000000000000000, 0.9238795325112867385, 1.000000000000000000, 0.9238795325112867385, 1.000000000000000000, 0.9238795325112867385, 1.000000000000000000),
 ( 1.000000000000000000, 0.9238795325112867385, 1.000000000000000000, 0.9238795325112867385, 1.000000000000000000, 0.9238795325112867385, 1.000000000000000000, 0.9238795325112867385, 1.000000000000000000, 0.9238795325112867385, 1.000000000000000000, 0.9238795325112867385, 1.000000000000000000, 0.9238795325112867385, 1.000000000000000000, 0.9238795325112867385, 1.000000000000000000, 0.9238795325112867385, 1.000000000000000000, 0.9238795325112867385, 1.000000000000000000, 0.9238795325112867385, 1.000000000000000000, 0.9238795325112867385, 1.000000000000000000, 0.9238795325112867385, 1.000000000000000000, 0.9238795325112867385, 1.000000000000000000, 0.9238795325112867385, 1.000000000000000000, 0.9238795325112867385, 1.000000000000000000, 0.9238795325112867385, 1.000000000000000000, 0.9238795325112867385, 1.000000000000000000, 0.9238795325112867385, 1.000000000000000000, 0.9238795325112867385, 1.000000000000000000, 0.9238795325112867385, 1.000000000000000000, 0.9238795325112867385, 1.000000000000000000, 0.9238795325112867385, 1.000000000000000000, 0.9238795325112867385, 1.000000000000000000, 0.9238795325112867385, 1.000000000000000000, 0.9238795325112867385, 1.000000000000000000, 0.9238795325112867385, 1.000000000000000000, 0.9238795325112867385, 1.000000000000000000, 0.9238795325112867385, 1.000000000000000000, 0.9238795325112867385, 1.000000000000000000, 0.9238795325112867385, 1.000000000000000000, 0.9238795325112867385, 1.000000000000000000, 0.9238795325112867385, 1.000000000000000000, 0.9238795325112867385, 1.000000000000000000, 0.9238795325112867385, 1.000000000000000000, 0.9238795325112867385, 1.000000000000000000, 0.9238795325112867385, 1.000000000000000000, 0.9238795325112867385, 1.000000000000000000, 0.9238795325112867385, 1.000000000000000000, 0.9238795325112867385, 1.000000000000000000) ) ) 
 REPRESENTATION_ITEM ( '' )  SURFACE ( )  );
#20016 =( GEOMETRIC_REPRESENTATION_CONTEXT ( 3 ) GLOBAL_UNCERTAINTY_ASSIGNED_CONTEXT ( ( #8982 ) ) GLOBAL_UNIT_ASSIGNED_CONTEXT ( ( #9848, #24538, #22839 ) ) REPRESENTATION_CONTEXT ( 'NONE', 'WORKASPACE' ) );
#20017 = CARTESIAN_POINT ( 'NONE',  ( 195.0000000000000000, 36.58476562608393579, -13.14518615778179544 ) ) ;
#20018 = CARTESIAN_POINT ( 'NONE',  ( 95.00472066334982912, 103.1245878333314323, -55.32499999726881157 ) ) ;
#20019 = ORIENTED_EDGE ( 'NONE', *, *, #2565, .F. ) ;
#20020 = CARTESIAN_POINT ( 'NONE',  ( -5.622872871577873077, 33.70742187500000142, -13.57481594606304753 ) ) ;
#20021 = CARTESIAN_POINT ( 'NONE',  ( -13.14518615778179189, 33.45937500108392726, 5.444914386472304635 ) ) ;
#20022 = ORIENTED_EDGE ( 'NONE', *, *, #7333, .F. ) ;
#20023 = CARTESIAN_POINT ( 'NONE',  ( 143.1451861577818079, 32.46718750108393436, -5.444914386472297529 ) ) ;
#20024 = CARTESIAN_POINT ( 'NONE',  ( 70.44491438647230552, 32.86406250108392868, 13.14518615778179189 ) ) ;
#20025 = AXIS2_PLACEMENT_3D ( 'NONE', #14287, #7606, #5900 ) ;
#20026 = CARTESIAN_POINT ( 'NONE',  ( 195.0000000000000000, 36.18789062608393436, 13.14518615778179544 ) ) ;
#20027 = ORIENTED_EDGE ( 'NONE', *, *, #16815, .T. ) ;
#20028 = CARTESIAN_POINT ( 'NONE',  ( 97.92893218813451028, 5.000000000000018652, 10.93750000273118417 ) ) ;
#20029 = CARTESIAN_POINT ( 'NONE',  ( -5.444914386472297529, 33.26093750108393721, -13.14518615778179900 ) ) ;
#20030 = CARTESIAN_POINT ( 'NONE',  ( 121.2451010467541010, 50.00000000000000000, -10.39041163855918981 ) ) ;
#20031 = CARTESIAN_POINT ( 'NONE',  ( 135.6228728715778971, 39.75976562716787299, 13.57481594606304576 ) ) ;
#20032 = CARTESIAN_POINT ( 'NONE',  ( 102.4976396683250925, 102.3130555110000159, -52.52500000273119696 ) ) ;
#20033 = CARTESIAN_POINT ( 'NONE',  ( 99.99999999999995737, -4.999999999999990230, 2.375000002731185500 ) ) ;
#20034 = CARTESIAN_POINT ( 'NONE',  ( -13.57481594606304398, 34.79882812716788010, 5.622872871577880183 ) ) ;
#20035 = CARTESIAN_POINT ( 'NONE',  ( 204.2950502721270425, 39.66054687608393436, -9.295050272127046043 ) ) ;
#20036 = AXIS2_PLACEMENT_3D ( 'NONE', #17011, #25998, #25714 ) ;
#20037 = ORIENTED_EDGE ( 'NONE', *, *, #3443, .T. ) ;
#20038 = CARTESIAN_POINT ( 'NONE',  ( 98.15313185440925281, 4.458734125000016313, 6.250000001365592084 ) ) ;
#20039 = EDGE_LOOP ( 'NONE', ( #16688, #2709 ) ) ;
#20040 = CARTESIAN_POINT ( 'NONE',  ( 97.93301269999999192, 123.7000000010924765, -0.8561741729129505041 ) ) ;
#20041 = CARTESIAN_POINT ( 'NONE',  ( 95.54126587499995082, -1.846868145590724986, 8.500000001365592084 ) ) ;
#20042 = CARTESIAN_POINT ( 'NONE',  ( 138.7548989532463395, 50.00000000000000000, 10.39041163855194050 ) ) ;
#20043 = CARTESIAN_POINT ( 'NONE',  ( -13.14518615778179189, 35.84062500108394289, 5.444914386472304635 ) ) ;
#20044 = CARTESIAN_POINT ( 'NONE',  ( -5.622872871578011633, 38.86679687716787868, 13.57481594606290720 ) ) ;
#20045 = CARTESIAN_POINT ( 'NONE',  ( -12.37587840034927744, 36.00000000000000000, 4.513979326318477980 ) ) ;
#20046 = CARTESIAN_POINT ( 'NONE',  ( 74.29505027212704249, 35.49335937608393721, 9.295050272127046043 ) ) ;
#20047 = CARTESIAN_POINT ( 'NONE',  ( 181.4251840539369596, 37.77539062499998579, -5.622872871577872189 ) ) ;
#20048 = CARTESIAN_POINT ( 'NONE',  ( 13.14518615778179544, 39.36289062608393152, -1.609821015232357215E-15 ) ) ;
#20049 =( BOUNDED_CURVE ( )  B_SPLINE_CURVE ( 2, ( #25091, #5435, #18256, #24948, #20398, #26964, #24672, #14102, #11821, #20684, #2863, #15820, #3426, #1167, #7408, #5578, #13955, #14243, #20544, #735, #24808, #24526, #16102, #11531, #5291, #22964, #20248, #5011, #9407, #12093, #16393, #3152, #18107, #15957, #5149, #27104, #13813, #1026, #9697, #7555, #14784, #12229, #18810, #1853, #8247, #10098, #12502, #8112, #1579, #3572, #23369, #25635, #1714, #20957, #19082, #1440, #5715, #3711, #21505, #18679, #27517, #7972, #14381, #21374, #16807, #25774, #16534, #14650, #23506, #21230, #27652, #10516, #10375, #27788, #19224, #16935, #23097, #25505, #12787, #21091, #27381 ),
 .UNSPECIFIED., .F., .F. ) 
 B_SPLINE_CURVE_WITH_KNOTS ( ( 3, 2, 2, 2, 2, 2, 2, 2, 2, 2, 2, 2, 2, 2, 2, 2, 2, 2, 2, 2, 2, 2, 2, 2, 2, 2, 2, 2, 2, 2, 2, 2, 2, 2, 2, 2, 2, 2, 2, 2, 3 ),
 ( 0.000000000000000000, 0.02500000000000000139, 0.05000000000000000278, 0.07499999999999999722, 0.1000000000000000056, 0.1250000000000000000, 0.1499999999999999944, 0.1749999999999999889, 0.2000000000000000111, 0.2250000000000000056, 0.2500000000000000000, 0.2750000000000000222, 0.2999999999999999889, 0.3250000000000000111, 0.3499999999999999778, 0.3750000000000000000, 0.4000000000000000222, 0.4249999999999999889, 0.4500000000000000111, 0.4749999999999999778, 0.5000000000000000000, 0.5250000000000000222, 0.5500000000000000444, 0.5749999999999999556, 0.5999999999999999778, 0.6250000000000000000, 0.6500000000000000222, 0.6750000000000000444, 0.6999999999999999556, 0.7249999999999999778, 0.7500000000000000000, 0.7750000000000000222, 0.8000000000000000444, 0.8249999999999999556, 0.8499999999999999778, 0.8750000000000000000, 0.9000000000000000222, 0.9250000000000000444, 0.9499999999999999556, 0.9749999999999999778, 1.000000000000000000 ),
 .UNSPECIFIED. ) 
 CURVE ( )  GEOMETRIC_REPRESENTATION_ITEM ( )  RATIONAL_B_SPLINE_CURVE ( ( 1.000000000000000000, 0.9238795325112867385, 1.000000000000000000, 0.9238795325112867385, 1.000000000000000000, 0.9238795325112867385, 1.000000000000000000, 0.9238795325112867385, 1.000000000000000000, 0.9238795325112867385, 1.000000000000000000, 0.9238795325112867385, 1.000000000000000000, 0.9238795325112867385, 1.000000000000000000, 0.9238795325112867385, 1.000000000000000000, 0.9238795325112867385, 1.000000000000000000, 0.9238795325112867385, 1.000000000000000000, 0.9238795325112867385, 1.000000000000000000, 0.9238795325112867385, 1.000000000000000000, 0.9238795325112867385, 1.000000000000000000, 0.9238795325112867385, 1.000000000000000000, 0.9238795325112867385, 1.000000000000000000, 0.9238795325112867385, 1.000000000000000000, 0.9238795325112867385, 1.000000000000000000, 0.9238795325112867385, 1.000000000000000000, 0.9238795325112867385, 1.000000000000000000, 0.9238795325112867385, 1.000000000000000000, 0.9238795325112867385, 1.000000000000000000, 0.9238795325112867385, 1.000000000000000000, 0.9238795325112867385, 1.000000000000000000, 0.9238795325112867385, 1.000000000000000000, 0.9238795325112867385, 1.000000000000000000, 0.9238795325112867385, 1.000000000000000000, 0.9238795325112867385, 1.000000000000000000, 0.9238795325112867385, 1.000000000000000000, 0.9238795325112867385, 1.000000000000000000, 0.9238795325112867385, 1.000000000000000000, 0.9238795325112867385, 1.000000000000000000, 0.9238795325112867385, 1.000000000000000000, 0.9238795325112867385, 1.000000000000000000, 0.9238795325112867385, 1.000000000000000000, 0.9238795325112867385, 1.000000000000000000, 0.9238795325112867385, 1.000000000000000000, 0.9238795325112867385, 1.000000000000000000, 0.9238795325112867385, 1.000000000000000000, 0.9238795325112867385, 1.000000000000000000, 0.9238795325112867385, 1.000000000000000000 ) ) 
 REPRESENTATION_ITEM ( '' )  );
#20050 = CARTESIAN_POINT ( 'NONE',  ( 99.99999999999997158, 117.3602355696678643, -52.99999999453763166 ) ) ;
#20051 = CARTESIAN_POINT ( 'NONE',  ( 3.636496246807550126, 51.46815297079190543, 14.99999999999999467 ) ) ;
#20052 = DIRECTION ( 'NONE',  ( 0.000000000000000000, 0.000000000000000000, 1.000000000000000000 ) ) ;
#20053 = CARTESIAN_POINT ( 'NONE',  ( 116.4251840539369596, 37.87460937499999147, 5.622872871577880183 ) ) ;
#20054 = ORIENTED_EDGE ( 'NONE', *, *, #11427, .T. ) ;
#20055 = DIRECTION ( 'NONE',  ( 1.000000000000000000, 0.000000000000000000, -1.156482317317871478E-16 ) ) ;
#20056 = CARTESIAN_POINT ( 'NONE',  ( 9.295050272127047819, 35.49335937608393721, 9.295050272127046043 ) ) ;
#20057 = CARTESIAN_POINT ( 'NONE',  ( -9.598844408820454532, 38.02343750216788010, 9.598844408820459861 ) ) ;
#20058 = CARTESIAN_POINT ( 'NONE',  ( 104.9999999999999574, -2.071067811865462627, 8.562500002731184168 ) ) ;
#20059 = CARTESIAN_POINT ( 'NONE',  ( 120.7049497278729575, 31.92148437608393508, 9.295050272127047819 ) ) ;
#20060 = CARTESIAN_POINT ( 'NONE',  ( 55.40115559117954547, 34.05468750216788010, 9.598844408820459861 ) ) ;
#20061 = AXIS2_PLACEMENT_3D ( 'NONE', #25256, #5746, #20991 ) ;
#20062 = EDGE_CURVE ( 'NONE', #3615, #2259, #20775, .T. ) ;
#20063 = CARTESIAN_POINT ( 'NONE',  ( 55.40115559117954547, 37.22968750216787726, 9.598844408820459861 ) ) ;
#20064 = CARTESIAN_POINT ( 'NONE',  ( 2.493653234604083739E-15, 33.36015625216786873, 13.57481594606304576 ) ) ;
#20065 = DIRECTION ( 'NONE',  ( -0.000000000000000000, -1.000000000000000000, -0.000000000000000000 ) ) ;
#20066 = CARTESIAN_POINT ( 'NONE',  ( 97.92893218813449607, 84.81250000000000000, -5.000000000000020428 ) ) ;
#20067 = AXIS2_PLACEMENT_3D ( 'NONE', #3947, #14613, #20778 ) ;
#20068 = CARTESIAN_POINT ( 'NONE',  ( -9.598844408820458085, 40.20625000216787726, -9.598844408820458085 ) ) ;
#20069 = CARTESIAN_POINT ( 'NONE',  ( 204.2950502721270425, 32.91367187608393152, 9.295050272127046043 ) ) ;
#20070 = DIRECTION ( 'NONE',  ( 0.000000000000000000, 0.000000000000000000, 1.000000000000000000 ) ) ;
#20071 = CARTESIAN_POINT ( 'NONE',  ( 101.7677669529663547, 124.7069999999781515, -1.767766952966370209 ) ) ;
#20072 =( LENGTH_UNIT ( ) NAMED_UNIT ( * ) SI_UNIT ( .MILLI., .METRE. ) );
#20073 = DIRECTION ( 'NONE',  ( -0.000000000000000000, 1.000000000000000000, -0.000000000000000000 ) ) ;
#20074 = CARTESIAN_POINT ( 'NONE',  ( 104.9999999999999716, 1.449011120738813565E-14, 15.00000000000000000 ) ) ;
#20075 = CARTESIAN_POINT ( 'NONE',  ( -8.312177448680279460E-16, 36.03906250000000000, -13.57481594606304576 ) ) ;
#20076 = APPLICATION_CONTEXT ( 'automotive_design' ) ;
#20077 = CARTESIAN_POINT ( 'NONE',  ( 65.00000000000000000, -7.395377635281828788, 11.57481594606303688 ) ) ;
#20078 = CARTESIAN_POINT ( 'NONE',  ( 2.414731522848535132E-15, 33.01289062608393721, 13.14518615778179544 ) ) ;
#20079 = CARTESIAN_POINT ( 'NONE',  ( 13.14518615778179900, 35.34453125108392868, 5.444914386472293977 ) ) ;
#20080 = CARTESIAN_POINT ( 'NONE',  ( 189.3771271284221314, 34.00507812499999716, 13.57481594606304753 ) ) ;
#20081 = VECTOR ( 'NONE', #19358, 1000.000000000000000 ) ;
#20082 = CARTESIAN_POINT ( 'NONE',  ( -9.598844408820458085, 36.23750000216787726, -9.598844408820458085 ) ) ;
#20083 = CARTESIAN_POINT ( 'NONE',  ( 91.00000000000000000, 110.0000000000000000, -55.00000000000000711 ) ) ;
#20084 = CARTESIAN_POINT ( 'NONE',  ( 107.0000000000000142, 110.0000000000000000, -45.50000000546238255 ) ) ;
#20085 = CARTESIAN_POINT ( 'NONE',  ( 65.00000000000000000, 36.78320312608393294, 13.14518615778179544 ) ) ;
#20086 = CARTESIAN_POINT ( 'NONE',  ( -13.57481594606304753, 35.49335937716787726, -5.622872871577872189 ) ) ;
#20087 = EDGE_LOOP ( 'NONE', ( #23853, #22981, #14167, #11897 ) ) ;
#20088 = CARTESIAN_POINT ( 'NONE',  ( 98.44193425395140196, 123.0000000000000711, -1.364916718493922820 ) ) ;
#20089 = CARTESIAN_POINT ( 'NONE',  ( -13.57481594606304576, 35.44374999999999432, 0.000000000000000000 ) ) ;
#20090 = CARTESIAN_POINT ( 'NONE',  ( 124.5550856135277087, 37.72578125108395142, 13.14518615778179722 ) ) ;
#20091 = ORIENTED_EDGE ( 'NONE', *, *, #4310, .F. ) ;
#20092 = CARTESIAN_POINT ( 'NONE',  ( 102.0710678118654329, 80.68750000000001421, -5.000000000000018652 ) ) ;
#20093 = AXIS2_PLACEMENT_3D ( 'NONE', #10722, #23850, #15420 ) ;
#20094 = CARTESIAN_POINT ( 'NONE',  ( 2.493653234604083739E-15, 34.84843749999999574, 13.57481594606304576 ) ) ;
#20095 = CARTESIAN_POINT ( 'NONE',  ( 103.5355339059327093, 81.75000000273119838, -3.535533905932755072 ) ) ;
#20096 = CARTESIAN_POINT ( 'NONE',  ( 103.5355339059327235, 93.12500000000000000, -3.535533905932738197 ) ) ;
#20097 = CARTESIAN_POINT ( 'NONE',  ( 104.4587341249999923, 94.49999999863442213, 1.846868145590726318 ) ) ;
#20098 =( BOUNDED_CURVE ( )  B_SPLINE_CURVE ( 2, ( #17744, #2786, #14018, #26445, #509, #9611, #19880, #13441, #24729 ),
 .UNSPECIFIED., .F., .T. ) 
 B_SPLINE_CURVE_WITH_KNOTS ( ( 3, 2, 2, 2, 3 ),
 ( 0.8928571428571427937, 0.9017857142857141906, 0.9107142857142855874, 0.9196428571428569843, 0.9285714285714284921 ),
 .UNSPECIFIED. ) 
 CURVE ( )  GEOMETRIC_REPRESENTATION_ITEM ( )  RATIONAL_B_SPLINE_CURVE ( ( 1.000000000000000888, 0.9238795325112857393, 1.000000000000000000, 0.9238795325112867385, 1.000000000000000000, 0.9238795325112867385, 1.000000000000000000, 0.9238795325112877377, 0.9999999999999990008 ) ) 
 REPRESENTATION_ITEM ( '' )  );
#20099 = CARTESIAN_POINT ( 'NONE',  ( 102.1631189606246295, 103.3426043859339103, -50.40000000000001279 ) ) ;
#20100 = CARTESIAN_POINT ( 'NONE',  ( 78.14518615778179367, 32.41757812608393863, -1.609821015232357215E-15 ) ) ;
#20101 = VERTEX_POINT ( 'NONE', #20332 ) ;
#20102 = DIRECTION ( 'NONE',  ( -0.000000000000000000, 1.000000000000000000, -0.000000000000000000 ) ) ;
#20103 = CARTESIAN_POINT ( 'NONE',  ( 99.99999999999995737, 5.000000000000018652, 12.75000000000000000 ) ) ;
#20104 = EDGE_CURVE ( 'NONE', #27809, #9474, #13749, .T. ) ;
#20105 = EDGE_LOOP ( 'NONE', ( #19020, #14196 ) ) ;
#20106 = CARTESIAN_POINT ( 'NONE',  ( 13.14518615778179900, 35.54296875108394715, 5.444914386472293977 ) ) ;
#20107 = CARTESIAN_POINT ( 'NONE',  ( 181.4251840539369596, 33.11210937716786873, -5.622872871577873077 ) ) ;
#20108 = EDGE_LOOP ( 'NONE', ( #6042, #4475, #10838, #3901 ) ) ;
#20109 = CARTESIAN_POINT ( 'NONE',  ( 13.14518615778179722, 32.96328125108393436, 5.444914386472293977 ) ) ;
#20110 = CARTESIAN_POINT ( 'NONE',  ( 114.9999999999999858, 125.0000000000000000, 14.99999999999998934 ) ) ;
#20111 = CARTESIAN_POINT ( 'NONE',  ( 0.000000000000000000, -7.395377635281828788, 13.57481594606304398 ) ) ;
#20112 = CARTESIAN_POINT ( 'NONE',  ( -13.14518615778179189, 33.65781250108393152, 5.444914386472304635 ) ) ;
#20113 = CARTESIAN_POINT ( 'NONE',  ( 135.4449143864723055, 32.07031250108393294, 13.14518615778179189 ) ) ;
#20114 = CARTESIAN_POINT ( 'NONE',  ( 70.62287287157788285, 33.31054687499999289, 13.57481594606304576 ) ) ;
#20115 = CARTESIAN_POINT ( 'NONE',  ( -20.00000000000000355, 80.00000000000000000, -14.99999999999999822 ) ) ;
#20116 = CARTESIAN_POINT ( 'NONE',  ( 103.1528011352953342, 3.152801135295383084, 12.31250000136559208 ) ) ;
#20117 = CARTESIAN_POINT ( 'NONE',  ( 95.54126587499996504, 84.43750000136560629, -1.387778780781445676E-14 ) ) ;
#20118 = CARTESIAN_POINT ( 'NONE',  ( 96.84719886470459471, 3.152801135295383084, 14.31250000136559208 ) ) ;
#20119 = CARTESIAN_POINT ( 'NONE',  ( 95.00472066334982912, 103.1245878333314323, -48.82500000273118701 ) ) ;
#20120 = CARTESIAN_POINT ( 'NONE',  ( 103.1528011352953484, 90.68749999863440792, -3.152801135295366208 ) ) ;
#20121 = CYLINDRICAL_SURFACE ( 'NONE', #12519, 5.000000000000004441 ) ;
#20122 = CARTESIAN_POINT ( 'NONE',  ( 102.4976396683250783, 102.3130555110000159, -51.02499999726882152 ) ) ;
#20123 = CARTESIAN_POINT ( 'NONE',  ( -13.14518615778179544, 36.78320312608393294, 0.000000000000000000 ) ) ;
#20124 = ORIENTED_EDGE ( 'NONE', *, *, #26766, .F. ) ;
#20125 = DIRECTION ( 'NONE',  ( -0.000000000000000000, -0.000000000000000000, 1.000000000000000000 ) ) ;
#20126 = CARTESIAN_POINT ( 'NONE',  ( 96.46446615806316061, 80.00000000000000000, -3.535533969928681852 ) ) ;
#20127 = DIRECTION ( 'NONE',  ( -0.000000000000000000, -1.000000000000000000, -0.000000000000000000 ) ) ;
#20128 = CARTESIAN_POINT ( 'NONE',  ( 200.4449143864723055, 36.03906250108394005, 13.14518615778179189 ) ) ;
#20129 =( BOUNDED_CURVE ( )  B_SPLINE_CURVE ( 2, ( #15244, #12405, #17112, #25816, #1751, #3880, #23823, #10829, #14823, #2166, #6291 ),
 .UNSPECIFIED., .F., .T. ) 
 B_SPLINE_CURVE_WITH_KNOTS ( ( 3, 2, 2, 2, 2, 3 ),
 ( 0.8000000000000000444, 0.8199999999999999512, 0.8399999999999999689, 0.8599999999999999867, 0.8800000000000000044, 0.9000000000000000222 ),
 .UNSPECIFIED. ) 
 CURVE ( )  GEOMETRIC_REPRESENTATION_ITEM ( )  RATIONAL_B_SPLINE_CURVE ( ( 1.000000000000000000, 0.9510565162951535312, 1.000000000000000000, 0.9510565162951535312, 1.000000000000000000, 0.9510565162951535312, 1.000000000000000000, 0.9510565162951535312, 1.000000000000000000, 0.9510565162951535312, 1.000000000000000000 ) ) 
 REPRESENTATION_ITEM ( '' )  );
#20130 = EDGE_LOOP ( 'NONE', ( #21284, #3677, #17460, #13071 ) ) ;
#20131 = EDGE_CURVE ( 'NONE', #13199, #20976, #7636, .T. ) ;
#20132 = CARTESIAN_POINT ( 'NONE',  ( 185.8198241863519513, 55.00000000000000000, -15.00000000000000000 ) ) ;
#20133 = CARTESIAN_POINT ( 'NONE',  ( 95.54126587499995082, 1.846868145590750077, 9.625000001365593860 ) ) ;
#20134 = VERTEX_POINT ( 'NONE', #819 ) ;
#20135 = CARTESIAN_POINT ( 'NONE',  ( 106.5389055433251002, 114.7507929638356785, -54.17500000273119554 ) ) ;
#20136 = CARTESIAN_POINT ( 'NONE',  ( -5.444914386472297529, 37.22968750108393721, -13.14518615778179900 ) ) ;
#20137 = CARTESIAN_POINT ( 'NONE',  ( 98.96446609406727646, 124.8500000000000085, -2.499999999999997780 ) ) ;
#20138 = EDGE_CURVE ( 'NONE', #9857, #19876, #2803, .T. ) ;
#20139 = CARTESIAN_POINT ( 'NONE',  ( 139.2950502721270425, 36.88242187608393152, 9.295050272127046043 ) ) ;
#20140 = CARTESIAN_POINT ( 'NONE',  ( 84.99999999999998579, 125.0000000000000000, -15.00000000000000888 ) ) ;
#20141 = CARTESIAN_POINT ( 'NONE',  ( -13.14518615778179900, 36.53515625108392584, -5.444914386472297529 ) ) ;
#20142 = CARTESIAN_POINT ( 'NONE',  ( 95.00000000000000000, 95.43749999726880162, 2.071067811865463959 ) ) ;
#20143 = CARTESIAN_POINT ( 'NONE',  ( 70.44491438647230552, 38.12265625108393152, -13.14518615778179900 ) ) ;
#20144 = CARTESIAN_POINT ( 'NONE',  ( 56.24510104675918853, 50.00000000000000000, -10.39041163855703864 ) ) ;
#20145 = CARTESIAN_POINT ( 'NONE',  ( 95.00472066334981491, 103.1245878333314465, -53.07500000273118701 ) ) ;
#20146 = VECTOR ( 'NONE', #27209, 1000.000000000000000 ) ;
#20147 = CARTESIAN_POINT ( 'NONE',  ( 204.2950502721270425, 32.51679687608393721, -9.295050272127046043 ) ) ;
#20148 = EDGE_CURVE ( 'NONE', #27429, #613, #16035, .T. ) ;
#20149 = CARTESIAN_POINT ( 'NONE',  ( 77.89215161363580364, 36.00000000000001421, -4.169510824906851987 ) ) ;
#20150 = CARTESIAN_POINT ( 'NONE',  ( 13.14518615778179900, 37.13046875108393863, 5.444914386472293977 ) ) ;
#20151 = CARTESIAN_POINT ( 'NONE',  ( 96.84719886470459471, 3.152801135295383084, 8.562500001365592084 ) ) ;
#20152 = CARTESIAN_POINT ( 'NONE',  ( 99.99999999999998579, 90.00000000000000000, -6.938893903907228378E-15 ) ) ;
#20153 = DIRECTION ( 'NONE',  ( -1.000000000000000000, 0.000000000000000000, 7.228014483236696740E-18 ) ) ;
#20154 = CARTESIAN_POINT ( 'NONE',  ( 94.99999999999995737, 1.387778780781445676E-14, 34.79898987322334136 ) ) ;
#20155 = ORIENTED_EDGE ( 'NONE', *, *, #20539, .T. ) ;
#20156 = CARTESIAN_POINT ( 'NONE',  ( 9.295050272127046043, 38.86679687608393863, -9.295050272127046043 ) ) ;
#20157 = CARTESIAN_POINT ( 'NONE',  ( 98.15313185440923860, 91.24999999863439371, 4.458734124999980786 ) ) ;
#20158 = CARTESIAN_POINT ( 'NONE',  ( 189.5550856135277229, 39.01562500108394005, -13.14518615778179722 ) ) ;
#20159 = CARTESIAN_POINT ( 'NONE',  ( 97.50236033167490746, 117.6869444889999841, -50.27499999726882152 ) ) ;
#20160 = VERTEX_POINT ( 'NONE', #9487 ) ;
#20161 = CARTESIAN_POINT ( 'NONE',  ( 13.57481594606304753, 33.50898437499999716, -5.622872871577873077 ) ) ;
#20162 = CARTESIAN_POINT ( 'NONE',  ( -9.295050272127046043, 33.31054687608393294, -9.295050272127046043 ) ) ;
#20163 = ORIENTED_EDGE ( 'NONE', *, *, #8912, .T. ) ;
#20164 = CARTESIAN_POINT ( 'NONE',  ( 143.1451861577818079, 34.05468750108394005, -5.444914386472297529 ) ) ;
#20165 = CARTESIAN_POINT ( 'NONE',  ( 59.55508561352770158, 31.67343750108393863, -13.14518615778179900 ) ) ;
#20166 = AXIS2_PLACEMENT_3D ( 'NONE', #3327, #12696, #25681 ) ;
#20167 = CARTESIAN_POINT ( 'NONE',  ( 200.4449143864723055, 33.85625000108393579, 13.14518615778179189 ) ) ;
#20168 = ORIENTED_EDGE ( 'NONE', *, *, #12792, .F. ) ;
#20169 = LINE ( 'NONE', #507, #227 ) ;
#20170 = CARTESIAN_POINT ( 'NONE',  ( 1.947325922083074978, 51.47162402671164472, -14.99999999999802114 ) ) ;
#20171 = CARTESIAN_POINT ( 'NONE',  ( 104.9999999999999716, -2.071067811865462627, 5.562500002731185056 ) ) ;
#20172 = EDGE_CURVE ( 'NONE', #789, #2926, #11617, .T. ) ;
#20173 = DIRECTION ( 'NONE',  ( 0.000000000000000000, 0.000000000000000000, -1.000000000000000000 ) ) ;
#20174 = CARTESIAN_POINT ( 'NONE',  ( 95.00472066334981491, 116.8754121666685393, -47.42500000273119554 ) ) ;
#20175 = CARTESIAN_POINT ( 'NONE',  ( 84.99999999999998579, 125.0000000000000000, -15.00000000000000888 ) ) ;
#20176 = CARTESIAN_POINT ( 'NONE',  ( 7.171391216998964424, 31.99955315621561525, -11.52591757658528948 ) ) ;
#20177 = EDGE_LOOP ( 'NONE', ( #23522, #18849, #26217, #18717 ) ) ;
#20178 = CARTESIAN_POINT ( 'NONE',  ( 103.1528011352953342, -3.152801135295355106, 5.812500001365591196 ) ) ;
#20179 = VERTEX_POINT ( 'NONE', #960 ) ;
#20180 = CARTESIAN_POINT ( 'NONE',  ( 101.0355339059327378, 122.9500000021849502, 2.499999999999977796 ) ) ;
#20181 = CARTESIAN_POINT ( 'NONE',  ( 103.1528011352953342, -3.152801135295355106, 7.812500001365592084 ) ) ;
#20182 = CARTESIAN_POINT ( 'NONE',  ( 195.0000000000000000, 39.31328125216787583, -13.57481594606304576 ) ) ;
#20183 = CARTESIAN_POINT ( 'NONE',  ( 13.14518615778179900, 35.44375000108393436, -5.444914386472297529 ) ) ;
#20184 = CARTESIAN_POINT ( 'NONE',  ( -12.05655202970026885, 36.00000000000000000, 5.307619621752119876 ) ) ;
#20185 = CYLINDRICAL_SURFACE ( 'NONE', #26257, 5.000000000000000000 ) ;
#20186 = CARTESIAN_POINT ( 'NONE',  ( 99.99999999999998579, 92.56249999863440792, -4.458734124999994997 ) ) ;
#20187 = CARTESIAN_POINT ( 'NONE',  ( 104.9952793366501851, 103.1245878333314323, -44.42500000273119554 ) ) ;
#20188 = CARTESIAN_POINT ( 'NONE',  ( 13.14518615778179722, 38.61875000108392442, -5.444914386472297529 ) ) ;
#20189 = CARTESIAN_POINT ( 'NONE',  ( 2.493653234604083739E-15, 34.05468749999999289, 13.57481594606304576 ) ) ;
#20190 = CARTESIAN_POINT ( 'NONE',  ( 195.0000000000000000, 39.61093749999999147, 13.57481594606304576 ) ) ;
#20191 = PLANE ( 'NONE',  #8777 ) ;
#20192 = CARTESIAN_POINT ( 'NONE',  ( 135.6228728715778686, 38.37070312499999147, -13.57481594606304753 ) ) ;
#20193 = ORIENTED_EDGE ( 'NONE', *, *, #15778, .T. ) ;
#20194 = CARTESIAN_POINT ( 'NONE',  ( 102.1631189606246153, 116.6573956140660897, -51.60000000000001563 ) ) ;
#20195 = CARTESIAN_POINT ( 'NONE',  ( -5.444914386472299306, 32.96328125108393436, 13.14518615778179722 ) ) ;
#20196 = CARTESIAN_POINT ( 'NONE',  ( 5.622872871577878406, 34.20351562716788862, 13.57481594606304576 ) ) ;
#20197 = CARTESIAN_POINT ( 'NONE',  ( 94.99999999999995737, 2.071067811865491048, 10.06250000273118417 ) ) ;
#20198 = CARTESIAN_POINT ( 'NONE',  ( 116.8548138422182063, 33.45937500108392726, 5.444914386472304635 ) ) ;
#20199 = CARTESIAN_POINT ( 'NONE',  ( 70.44491438647230552, 39.21406250108392300, 13.14518615778179189 ) ) ;
#20200 = CARTESIAN_POINT ( 'NONE',  ( 13.57481594606304576, 31.97109375216787441, -1.662435489736055892E-15 ) ) ;
#20201 = CARTESIAN_POINT ( 'NONE',  ( 104.4587341249999781, 95.43749999863440792, -6.938893903907228378E-15 ) ) ;
#20202 = CARTESIAN_POINT ( 'NONE',  ( 102.4976396683250783, 102.3130555110000159, -47.27499999726882152 ) ) ;
#20203 = CARTESIAN_POINT ( 'NONE',  ( 13.57481594606304931, 38.27148437716787299, 5.622872871577869525 ) ) ;
#20204 = CARTESIAN_POINT ( 'NONE',  ( 189.5550856135277229, 33.55859375108393294, 13.14518615778179722 ) ) ;
#20205 = CARTESIAN_POINT ( 'NONE',  ( 102.4999999999999858, 123.0000000000000000, -8.724596124144689908E-15 ) ) ;
#20206 = CARTESIAN_POINT ( 'NONE',  ( -5.622872871577965448, 33.31054687716787299, 13.57481594606295161 ) ) ;
#20207 = DIRECTION ( 'NONE',  ( -0.000000000000000000, -1.000000000000000000, -0.000000000000000000 ) ) ;
#20209 = EDGE_LOOP ( 'NONE', ( #7, #20013, #6307, #148 ) ) ;
#20208 = CARTESIAN_POINT ( 'NONE',  ( -15.00000000000000355, 55.00000000000000000, -9.999999999999998224 ) ) ;
#20210 = FACE_OUTER_BOUND ( 'NONE', #26858, .T. ) ;
#20211 = LINE ( 'NONE', #844, #119 ) ;
#20212 = CARTESIAN_POINT ( 'NONE',  ( 13.57481594606304931, 34.20351562499999432, 5.622872871577869525 ) ) ;
#20213 = CARTESIAN_POINT ( 'NONE',  ( 104.3262379212492590, 115.9545556584642867, -54.70000000000000284 ) ) ;
#20214 =( BOUNDED_CURVE ( )  B_SPLINE_CURVE ( 2, ( #27230, #7826, #5273, #18665, #23082, #9678, #11659, #18238, #9950 ),
 .UNSPECIFIED., .F., .F. ) 
 B_SPLINE_CURVE_WITH_KNOTS ( ( 3, 2, 2, 2, 3 ),
 ( 0.3541666666666666852, 0.3645833333333332593, 0.3749999999999998890, 0.3854166666666665741, 0.3958333333333331483 ),
 .UNSPECIFIED. ) 
 CURVE ( )  GEOMETRIC_REPRESENTATION_ITEM ( )  RATIONAL_B_SPLINE_CURVE ( ( 1.000000000000000000, 0.9238795325112867385, 1.000000000000000000, 0.9238795325112867385, 1.000000000000000000, 0.9238795325112867385, 1.000000000000000000, 0.9238795325112879597, 0.9999999999999987788 ) ) 
 REPRESENTATION_ITEM ( '' )  );
#20215 = CARTESIAN_POINT ( 'NONE',  ( 5.444914386472302859, 33.85625000108393579, 13.14518615778179189 ) ) ;
#20216 = CARTESIAN_POINT ( 'NONE',  ( -5.444914386472297529, 36.43593750108392726, -13.14518615778179900 ) ) ;
#20217 = CARTESIAN_POINT ( 'NONE',  ( -13.14518615778179189, 35.84062500108394289, 5.444914386472304635 ) ) ;
#20218 = CARTESIAN_POINT ( 'NONE',  ( 2.493653234604083739E-15, 34.94765625216787441, 13.57481594606304576 ) ) ;
#20219 = CARTESIAN_POINT ( 'NONE',  ( 9.598844408820456309, 36.73359374999999716, -9.598844408820458085 ) ) ;
#20220 = CARTESIAN_POINT ( 'NONE',  ( 104.4587341249999781, 83.87500000136560629, 1.846868145590721655 ) ) ;
#20221 = CARTESIAN_POINT ( 'NONE',  ( 55.70494972787295751, 33.31054687608393294, -9.295050272127046043 ) ) ;
#20222 = EDGE_CURVE ( 'NONE', #3364, #7953, #26200, .T. ) ;
#20223 = CARTESIAN_POINT ( 'NONE',  ( 104.9952793366501851, 103.1245878333314323, -52.67500000273119554 ) ) ;
#20224 = LINE ( 'NONE', #22364, #12724 ) ;
#20225 = ORIENTED_EDGE ( 'NONE', *, *, #14698, .F. ) ;
#20226 = CARTESIAN_POINT ( 'NONE',  ( 99.99999999999998579, 123.9500000010924765, 2.066987299999980099 ) ) ;
#20227 = SPHERICAL_SURFACE ( 'NONE', #1769, 5.000000000000000000 ) ;
#20228 = CARTESIAN_POINT ( 'NONE',  ( 120.7049497278729575, 36.88242187608393152, 9.295050272127047819 ) ) ;
#20229 = ORIENTED_EDGE ( 'NONE', *, *, #22032, .F. ) ;
#20230 = LINE ( 'NONE', #15935, #1372 ) ;
#20231 = CARTESIAN_POINT ( 'NONE',  ( 94.33688103937534208, 114.1144967660473242, -47.20000000000000995 ) ) ;
#20232 = CARTESIAN_POINT ( 'NONE',  ( 103.1528011352953342, 82.81250000136560629, 3.152801135295355106 ) ) ;
#20233 = CARTESIAN_POINT ( 'NONE',  ( 97.92893218813452449, 90.68749999999998579, 4.999999999999983125 ) ) ;
#20234 = CARTESIAN_POINT ( 'NONE',  ( 104.4587341249999781, 95.56249999863440792, -6.938893903907228378E-15 ) ) ;
#20235 = VECTOR ( 'NONE', #2605, 999.9999999999998863 ) ;
#20236 = CARTESIAN_POINT ( 'NONE',  ( 91.91746824999998466, 110.0000000000000000, -49.62499999726882294 ) ) ;
#20237 = CARTESIAN_POINT ( 'NONE',  ( 51.85481384221820633, 32.02070312608393010, 0.000000000000000000 ) ) ;
#20238 = ORIENTED_EDGE ( 'NONE', *, *, #1788, .T. ) ;
#20239 = CARTESIAN_POINT ( 'NONE',  ( 0.000000000000000000, -7.395377635281828788, 13.57481594606304398 ) ) ;
#20240 = CARTESIAN_POINT ( 'NONE',  ( 99.99999999999995737, -4.999999999999990230, 12.25000000000000000 ) ) ;
#20241 = EDGE_LOOP ( 'NONE', ( #15423, #20443, #24503, #16383, #15554, #2146, #14858, #362, #18519, #11269, #21642, #18870, #24377, #753 ) ) ;
#20242 = CARTESIAN_POINT ( 'NONE',  ( 5.444914386472302859, 35.44375000108393436, 13.14518615778179189 ) ) ;
#20243 = CARTESIAN_POINT ( 'NONE',  ( 195.0000000000000000, 34.55078125216787299, -13.57481594606304576 ) ) ;
#20244 = CARTESIAN_POINT ( 'NONE',  ( 9.295050272127047819, 32.91367187608393152, 9.295050272127046043 ) ) ;
#20245 = CARTESIAN_POINT ( 'NONE',  ( 95.27063293749995410, 1.387778780781445676E-14, 0.8437500006827957089 ) ) ;
#20246 = CARTESIAN_POINT ( 'NONE',  ( -13.14518615778179900, 33.55859375108393294, -5.444914386472297529 ) ) ;
#20247 = DIRECTION ( 'NONE',  ( -1.000000000000000000, 0.000000000000000000, 0.000000000000000000 ) ) ;
#20248 = CARTESIAN_POINT ( 'NONE',  ( 96.84719886470463734, 91.93749999863440792, 3.152801135295351997 ) ) ;
#20249 = FACE_OUTER_BOUND ( 'NONE', #12401, .T. ) ;
#20250 = DIRECTION ( 'NONE',  ( 1.000000000000000000, 0.000000000000000000, -0.000000000000000000 ) ) ;
#20251 = CARTESIAN_POINT ( 'NONE',  ( 99.99999999999995737, 4.458734125000016313, 6.437500001365592084 ) ) ;
#20252 = CARTESIAN_POINT ( 'NONE',  ( 195.0000000000000000, -7.395377635281828788, 13.57481594606302266 ) ) ;
#20253 = EDGE_CURVE ( 'NONE', #8168, #3810, #20617, .T. ) ;
#20254 = AXIS2_PLACEMENT_3D ( 'NONE', #14740, #7923, #14604 ) ;
#20255 = CARTESIAN_POINT ( 'NONE',  ( 104.4587341249999781, -1.846868145590721655, 11.87500000136559208 ) ) ;
#20256 = CARTESIAN_POINT ( 'NONE',  ( 93.00000000000001421, 112.2744378736303332, -52.60000000546237686 ) ) ;
#20257 = FACE_OUTER_BOUND ( 'NONE', #19656, .T. ) ;
#20258 = CARTESIAN_POINT ( 'NONE',  ( 99.99999999999998579, 110.0000000000000000, 15.00099999999999412 ) ) ;
#20259 = CARTESIAN_POINT ( 'NONE',  ( 97.50236033167490746, 117.6869444889999841, -54.02499999726882862 ) ) ;
#20260 = CARTESIAN_POINT ( 'NONE',  ( 5.444914386472302859, 34.65000000108393863, 13.14518615778179189 ) ) ;
#20261 = VERTEX_POINT ( 'NONE', #1102 ) ;
#20262 = CARTESIAN_POINT ( 'NONE',  ( 116.4251840539369596, 37.03124999999999289, 0.000000000000000000 ) ) ;
#20263 =( BOUNDED_CURVE ( )  B_SPLINE_CURVE ( 2, ( #10033, #16458, #10304, #5643, #25438, #27444, #14723, #27724, #23441 ),
 .UNSPECIFIED., .F., .F. ) 
 B_SPLINE_CURVE_WITH_KNOTS ( ( 3, 2, 2, 2, 3 ),
 ( 0.06250000000000004163, 0.07291666666666665741, 0.08333333333333325932, 0.09374999999999987510, 0.1041666666666664909 ),
 .UNSPECIFIED. ) 
 CURVE ( )  GEOMETRIC_REPRESENTATION_ITEM ( )  RATIONAL_B_SPLINE_CURVE ( ( 0.9999999999999996669, 0.9238795325112870716, 1.000000000000000000, 0.9238795325112867385, 1.000000000000000000, 0.9238795325112867385, 1.000000000000000000, 0.9238795325112880708, 0.9999999999999986677 ) ) 
 REPRESENTATION_ITEM ( '' )  );
#20264 = CARTESIAN_POINT ( 'NONE',  ( 0.000000000000000000, 1.000000000000000000, 23.26794919243112503 ) ) ;
#20265 = CYLINDRICAL_SURFACE ( 'NONE', #21593, 5.000000000000004441 ) ;
#20266 = CARTESIAN_POINT ( 'NONE',  ( 204.2950502721270425, 36.88242187608393152, 9.295050272127046043 ) ) ;
#20267 = VERTEX_POINT ( 'NONE', #27185 ) ;
#20268 = CARTESIAN_POINT ( 'NONE',  ( 107.0000000000000000, 110.0000000000000000, -49.49999999453764588 ) ) ;
#20269 = CARTESIAN_POINT ( 'NONE',  ( 95.54126587499995082, -1.846868145590724986, 11.75000000136559208 ) ) ;
#20270 = ORIENTED_EDGE ( 'NONE', *, *, #3693, .F. ) ;
#20271 = CARTESIAN_POINT ( 'NONE',  ( 99.99999999999998579, 101.5015231886685854, -52.87500000273119838 ) ) ;
#20272 = AXIS2_PLACEMENT_3D ( 'NONE', #28063, #4258, #12503 ) ;
#20273 = CARTESIAN_POINT ( 'NONE',  ( 13.14518615778179900, 37.82500000108392868, -5.444914386472297529 ) ) ;
#20274 = CARTESIAN_POINT ( 'NONE',  ( 97.50000000000000000, 124.2000000000000028, -9.540979117872439019E-15 ) ) ;
#20275 = CARTESIAN_POINT ( 'NONE',  ( 139.2950502721270425, 38.66835937608393436, -9.295050272127046043 ) ) ;
#20276 = CARTESIAN_POINT ( 'NONE',  ( -13.14518615778179544, 38.37070312608393152, 0.000000000000000000 ) ) ;
#20277 = CARTESIAN_POINT ( 'NONE',  ( 2.414731522848535132E-15, 34.40195312608393152, 13.14518615778179544 ) ) ;
#20278 = EDGE_CURVE ( 'NONE', #13933, #13505, #22333, .T. ) ;
#20279 = CARTESIAN_POINT ( 'NONE',  ( 98.15313185440925281, 91.87499999863439371, -4.458734124999994997 ) ) ;
#20280 = VECTOR ( 'NONE', #13212, 1000.000000000000000 ) ;
#20281 = CARTESIAN_POINT ( 'NONE',  ( 99.99999999999998579, 101.5015231886685712, -50.87500000273119127 ) ) ;
#20282 = CARTESIAN_POINT ( 'NONE',  ( 208.1451861577818079, 32.41757812608393863, -1.609821015232357215E-15 ) ) ;
#20283 = ORIENTED_EDGE ( 'NONE', *, *, #20675, .F. ) ;
#20284 = CARTESIAN_POINT ( 'NONE',  ( 67.23232715533710291, 35.99999999999999289, 12.98409812936893104 ) ) ;
#20285 = ORIENTED_EDGE ( 'NONE', *, *, #11083, .F. ) ;
#20286 = CARTESIAN_POINT ( 'NONE',  ( 9.295050272127046043, 35.69179687608394147, -9.295050272127046043 ) ) ;
#20287 = CARTESIAN_POINT ( 'NONE',  ( 95.54126587499996504, 1.387778780781445676E-14, 6.687500001365592084 ) ) ;
#20288 = EDGE_CURVE ( 'NONE', #19120, #756, #9638, .T. ) ;
#20289 = CARTESIAN_POINT ( 'NONE',  ( 59.55508561352770158, 37.52734375108393294, 13.14518615778179722 ) ) ;
#20290 = CARTESIAN_POINT ( 'NONE',  ( 103.5355339059327235, 90.99999999726880162, -3.535533905932738197 ) ) ;
#20291 = DIRECTION ( 'NONE',  ( -0.000000000000000000, -0.000000000000000000, -1.000000000000000000 ) ) ;
#20292 = ORIENTED_EDGE ( 'NONE', *, *, #3063, .T. ) ;
#20293 = EDGE_CURVE ( 'NONE', #4709, #26902, #4092, .T. ) ;
#20294 = CARTESIAN_POINT ( 'NONE',  ( 13.14518615778179544, 33.21132812608393436, -1.609821015232357215E-15 ) ) ;
#20295 = CARTESIAN_POINT ( 'NONE',  ( 100.8561741729129153, 123.5000000010924737, -2.066987299999999195 ) ) ;
#20296 = CARTESIAN_POINT ( 'NONE',  ( 96.84719886470463734, 91.93749999863440792, -3.152801135295366208 ) ) ;
#20297 = CARTESIAN_POINT ( 'NONE',  ( 208.1451861577818079, 37.18007812608393436, -1.609821015232357215E-15 ) ) ;
#20298 = CARTESIAN_POINT ( 'NONE',  ( 102.4976396683250783, 102.3130555110000159, -51.27499999726882152 ) ) ;
#20299 = ADVANCED_FACE ( 'NONE', ( #18751 ), #25159, .T. ) ;
#20300 = ORIENTED_EDGE ( 'NONE', *, *, #25878, .F. ) ;
#20301 = CARTESIAN_POINT ( 'NONE',  ( 13.57481594606304931, 33.40976562499999858, 5.622872871577869525 ) ) ;
#20302 = CARTESIAN_POINT ( 'NONE',  ( 13.14518615778179900, 35.44375000108393436, -5.444914386472297529 ) ) ;
#20303 = AXIS2_PLACEMENT_3D ( 'NONE', #5227, #14038, #3088 ) ;
#20304 = VERTEX_POINT ( 'NONE', #21032 ) ;
#20305 = CARTESIAN_POINT ( 'NONE',  ( 135.4449143864723055, 32.56640625108394005, -13.14518615778179900 ) ) ;
#20306 = ADVANCED_FACE ( 'NONE', ( #19164 ), #12539, .T. ) ;
#20307 = CARTESIAN_POINT ( 'NONE',  ( 181.8548138422181921, 33.55859375108393294, -5.444914386472297529 ) ) ;
#20308 = ORIENTED_EDGE ( 'NONE', *, *, #22404, .F. ) ;
#20309 = CARTESIAN_POINT ( 'NONE',  ( 99.14382582708708469, 123.9000000010924794, 2.066987299999979655 ) ) ;
#20310 = CARTESIAN_POINT ( 'NONE',  ( 99.99999999999998579, 91.62499999726880162, 4.999999999999984013 ) ) ;
#20311 = CARTESIAN_POINT ( 'NONE',  ( 94.99999999999995737, 1.387778780781445676E-14, 5.125000002731184168 ) ) ;
#20312 = CARTESIAN_POINT ( 'NONE',  ( 143.5748159460630404, 36.68398437716788152, 5.622872871577869525 ) ) ;
#20313 = CARTESIAN_POINT ( 'NONE',  ( 97.50236033167492167, 117.6869444889999841, -45.52500000273119696 ) ) ;
#20314 = CARTESIAN_POINT ( 'NONE',  ( 104.9999999999999716, 1.449011120738813565E-14, 2.625000002731185500 ) ) ;
#20315 = CARTESIAN_POINT ( 'NONE',  ( -9.598844408820458085, 33.85625000216787583, -9.598844408820458085 ) ) ;
#20316 = CARTESIAN_POINT ( 'NONE',  ( 74.18017581364802027, 55.00000000000001421, 14.99999999999997691 ) ) ;
#20317 = EDGE_CURVE ( 'NONE', #1074, #15490, #25579, .T. ) ;
#20318 = EDGE_LOOP ( 'NONE', ( #5868, #9387, #2671, #7475 ) ) ;
#20319 = CARTESIAN_POINT ( 'NONE',  ( 98.15313185440925281, 4.458734125000016313, 4.250000001365592084 ) ) ;
#20320 = AXIS2_PLACEMENT_3D ( 'NONE', #1912, #19421, #24262 ) ;
#20321 = ORIENTED_EDGE ( 'NONE', *, *, #13660, .F. ) ;
#20322 = CARTESIAN_POINT ( 'NONE',  ( 96.46446609406721961, 3.535533905932755072, 13.00000000273118417 ) ) ;
#20323 = CARTESIAN_POINT ( 'NONE',  ( 101.8468681455906903, -4.458734124999987891, 9.750000001365593860 ) ) ;
#20324 = CARTESIAN_POINT ( 'NONE',  ( 200.6228728715777834, 38.37070312499999858, -13.57481594606313990 ) ) ;
#20325 = CARTESIAN_POINT ( 'NONE',  ( 9.295050272127046043, 36.28710937608393294, -9.295050272127046043 ) ) ;
#20326 = LINE ( 'NONE', #11603, #16523 ) ;
#20327 = CARTESIAN_POINT ( 'NONE',  ( 68.75563991928589758, 31.78804746655075419, -13.14518615778179544 ) ) ;
#20328 = CARTESIAN_POINT ( 'NONE',  ( 96.46446609406721961, -3.535533905932727539, 5.124999999999999112 ) ) ;
#20329 = CARTESIAN_POINT ( 'NONE',  ( 108.0825317500000153, 110.0000000000000000, -44.12500000273119127 ) ) ;
#20330 = CARTESIAN_POINT ( 'NONE',  ( 2.414731522848535132E-15, 37.57695312608392868, 13.14518615778179544 ) ) ;
#20331 = EDGE_CURVE ( 'NONE', #14666, #22034, #26381, .T. ) ;
#20332 = CARTESIAN_POINT ( 'NONE',  ( 99.99999999999998579, 95.00000000000000000, -4.999999999999996447 ) ) ;
#20333 = CARTESIAN_POINT ( 'NONE',  ( -7.636241067998421173, 54.91786508990982441, 14.99999999999999822 ) ) ;
#20334 = CARTESIAN_POINT ( 'NONE',  ( 97.92893218813452449, 91.56249999726883004, 4.999999999999983125 ) ) ;
#20335 = CARTESIAN_POINT ( 'NONE',  ( 124.3771271284221314, 34.50117187499999005, -13.57481594606304753 ) ) ;
#20336 = VERTEX_POINT ( 'NONE', #10169 ) ;
#20337 = EDGE_CURVE ( 'NONE', #25472, #22143, #13911, .T. ) ;
#20338 = ORIENTED_EDGE ( 'NONE', *, *, #17196, .T. ) ;
#20339 = CARTESIAN_POINT ( 'NONE',  ( -5.622872871577767384, 40.15664062716787441, -13.57481594606315412 ) ) ;
#20340 = CARTESIAN_POINT ( 'NONE',  ( 13.14518615778179900, 33.26093750108393721, -5.444914386472297529 ) ) ;
#20341 = CARTESIAN_POINT ( 'NONE',  ( -5.622872871577873077, 33.01289062716787726, -13.57481594606304753 ) ) ;
#20342 = AXIS2_PLACEMENT_3D ( 'NONE', #17961, #4719, #879 ) ;
#20343 = CARTESIAN_POINT ( 'NONE',  ( 96.46446609406721961, -3.535533905932727539, 9.250000002731184168 ) ) ;
#20344 = CARTESIAN_POINT ( 'NONE',  ( 135.4449143864723055, 34.74921875108394431, -13.14518615778179900 ) ) ;
#20345 = CARTESIAN_POINT ( 'NONE',  ( 59.55508561352770158, 39.11484375108394573, 13.14518615778179722 ) ) ;
#20346 = CARTESIAN_POINT ( 'NONE',  ( 65.00000000000000000, 37.32890625216786873, 13.57481594606304576 ) ) ;
#20347 = CARTESIAN_POINT ( 'NONE',  ( 5.444914386472297529, 38.71796875108393721, -13.14518615778179900 ) ) ;
#20348 = AXIS2_PLACEMENT_3D ( 'NONE', #14128, #22027, #20711 ) ;
#20349 = CARTESIAN_POINT ( 'NONE',  ( -9.295050272127046043, 31.92148437608393508, -9.295050272127046043 ) ) ;
#20350 = CARTESIAN_POINT ( 'NONE',  ( 99.99999999999995737, 5.000000000000018652, 1.749999999999999778 ) ) ;
#20351 = CARTESIAN_POINT ( 'NONE',  ( 104.9952793366501567, 116.8754121666685393, -52.57499999726881867 ) ) ;
#20352 = CARTESIAN_POINT ( 'NONE',  ( 5.622872871577878406, 38.96601562716787015, 13.57481594606304576 ) ) ;
#20353 = CARTESIAN_POINT ( 'NONE',  ( 208.1451861577817795, 32.26875000108393721, -5.444914386472297529 ) ) ;
#20354 = CARTESIAN_POINT ( 'NONE',  ( 195.0000000000000000, -7.395377635281828788, -2.255140518769849538E-14 ) ) ;
#20355 = CARTESIAN_POINT ( 'NONE',  ( 99.99999999999998579, 124.4069999999781402, 2.499999999999978684 ) ) ;
#20356 = CARTESIAN_POINT ( 'NONE',  ( 200.6228728715779255, 38.86679687500001279, 13.57481594606301023 ) ) ;
#20357 = CARTESIAN_POINT ( 'NONE',  ( 116.4251840539369738, 36.38632812716788578, 5.622872871577880183 ) ) ;
#20358 = CARTESIAN_POINT ( 'NONE',  ( 101.7677669529663547, 123.2000000021849502, -1.767766952966370209 ) ) ;
#20359 = CARTESIAN_POINT ( 'NONE',  ( 13.57481594606304931, 32.61601562499999574, 5.622872871577869525 ) ) ;
#20360 = CARTESIAN_POINT ( 'NONE',  ( 109.0000000000000142, 110.0000000000000000, -55.00000000000000711 ) ) ;
#20361 = AXIS2_PLACEMENT_3D ( 'NONE', #3008, #18545, #14387 ) ;
#20362 = CARTESIAN_POINT ( 'NONE',  ( 13.14518615778179900, 33.95546875108393436, 5.444914386472293977 ) ) ;
#20363 = CARTESIAN_POINT ( 'NONE',  ( 5.444914386472297529, 32.36796875108393579, -13.14518615778179900 ) ) ;
#20364 = CARTESIAN_POINT ( 'NONE',  ( 208.5748159460630120, 32.61601562499999574, 5.622872871577869525 ) ) ;
#20365 = EDGE_CURVE ( 'NONE', #6963, #10159, #3647, .T. ) ;
#20366 = CARTESIAN_POINT ( 'NONE',  ( 13.57481594606304753, 35.19570312716788152, -5.622872871577873077 ) ) ;
#20367 = CARTESIAN_POINT ( 'NONE',  ( 130.0000000000000000, 50.00000000000000000, -1.503427012513233026E-14 ) ) ;
#20368 = FACE_OUTER_BOUND ( 'NONE', #13654, .T. ) ;
#20369 = CARTESIAN_POINT ( 'NONE',  ( 78.14518615778179367, 32.96328125108393436, 5.444914386472293977 ) ) ;
#20370 = CARTESIAN_POINT ( 'NONE',  ( 95.00472066334982912, 116.8754121666685393, -51.67500000273118133 ) ) ;
#20371 = CARTESIAN_POINT ( 'NONE',  ( 99.35312936802752404, 123.0000000000000284, -2.419468906465395364 ) ) ;
#20372 = ORIENTED_EDGE ( 'NONE', *, *, #25061, .F. ) ;
#20373 = CARTESIAN_POINT ( 'NONE',  ( 98.53841926354351699, 123.6500000010924794, -1.461580736456474794 ) ) ;
#20374 = CARTESIAN_POINT ( 'NONE',  ( 13.57481594606304931, 32.61601562499999574, 5.622872871577869525 ) ) ;
#20375 = CARTESIAN_POINT ( 'NONE',  ( 124.5550856135277087, 35.04687500108393294, -13.14518615778179900 ) ) ;
#20376 = EDGE_LOOP ( 'NONE', ( #26405, #1867, #16008, #16961 ) ) ;
#20377 = CARTESIAN_POINT ( 'NONE',  ( 104.9999999999999716, 80.50000000000000000, -1.449011120738813565E-14 ) ) ;
#20378 = CARTESIAN_POINT ( 'NONE',  ( 93.00000000000000000, 112.2744378736303332, -47.10000000000000853 ) ) ;
#20379 = CARTESIAN_POINT ( 'NONE',  ( 102.0710678118654329, 79.43750000273119838, 4.999999999999989342 ) ) ;
#20380 = CARTESIAN_POINT ( 'NONE',  ( 102.0710678118654613, 90.81249999999998579, 4.999999999999983125 ) ) ;
#20381 = CARTESIAN_POINT ( 'NONE',  ( 74.59884440882045453, 39.01562500216787299, 9.598844408820456309 ) ) ;
#20382 = CARTESIAN_POINT ( 'NONE',  ( 95.00472066334982912, 116.8754121666685393, -49.92499999726880588 ) ) ;
#20383 = CARTESIAN_POINT ( 'NONE',  ( 59.55508561352770158, 32.16953125108393152, 13.14518615778179722 ) ) ;
#20384 = CARTESIAN_POINT ( 'NONE',  ( -5.622872871577873077, 37.77539062716788010, -13.57481594606304753 ) ) ;
#20385 = VERTEX_POINT ( 'NONE', #10874 ) ;
#20386 = CARTESIAN_POINT ( 'NONE',  ( 198.0892609137967497, 36.00000000000000000, -13.21136010216380718 ) ) ;
#20387 = CARTESIAN_POINT ( 'NONE',  ( 104.9999999999999574, -2.071067811865462627, 14.43749999999999822 ) ) ;
#20388 = VERTEX_POINT ( 'NONE', #4341 ) ;
#20389 = CARTESIAN_POINT ( 'NONE',  ( 9.295050272127047819, 37.87460937608393863, 9.295050272127046043 ) ) ;
#20390 = CARTESIAN_POINT ( 'NONE',  ( 181.4251840539369596, 32.31835937716786589, -5.622872871577873077 ) ) ;
#20391 =( BOUNDED_CURVE ( )  B_SPLINE_CURVE ( 2, ( #11347, #18352, #548, #9229, #17922, #7363, #22639, #13912, #3107 ),
 .UNSPECIFIED., .F., .F. ) 
 B_SPLINE_CURVE_WITH_KNOTS ( ( 3, 2, 2, 2, 3 ),
 ( 0.8958333333333335924, 0.9062500000000002220, 0.9166666666666667407, 0.9270833333333334814, 0.9375000000000000000 ),
 .UNSPECIFIED. ) 
 CURVE ( )  GEOMETRIC_REPRESENTATION_ITEM ( )  RATIONAL_B_SPLINE_CURVE ( ( 0.9999999999999983347, 0.9238795325112884038, 1.000000000000000000, 0.9238795325112867385, 1.000000000000000000, 0.9238795325112867385, 1.000000000000000000, 0.9238795325112867385, 1.000000000000000000 ) ) 
 REPRESENTATION_ITEM ( '' )  );
#20392 = CARTESIAN_POINT ( 'NONE',  ( -13.14518615778179722, 33.36015625108393579, -5.444914386472297529 ) ) ;
#20393 = PRODUCT ( 'suction cup mounting thread', 'suction cup mounting thread', '', ( #5718 ) ) ;
#20394 = CARTESIAN_POINT ( 'NONE',  ( 13.57481594606304753, 36.78320312716788010, -5.622872871577873966 ) ) ;
#20395 = DIRECTION ( 'NONE',  ( 0.000000000000000000, 0.000000000000000000, -1.000000000000000000 ) ) ;
#20396 = CARTESIAN_POINT ( 'NONE',  ( -13.14518615778179544, 35.19570312608393436, 0.000000000000000000 ) ) ;
#20397 = CARTESIAN_POINT ( 'NONE',  ( 143.1451861577818079, 33.01289062608393010, -1.609821015232357215E-15 ) ) ;
#20398 = CARTESIAN_POINT ( 'NONE',  ( 99.99999999999998579, 90.56249999863440792, -4.458734124999994997 ) ) ;
#20399 = CARTESIAN_POINT ( 'NONE',  ( 99.99999999999998579, 138.0000000000000000, -5.204170427930421283E-15 ) ) ;
#20400 = CARTESIAN_POINT ( 'NONE',  ( 0.000000000000000000, 0.000000000000000000, 0.000000000000000000 ) ) ;
#20401 = CARTESIAN_POINT ( 'NONE',  ( 13.57481594606304753, 35.98945312716787015, -5.622872871577873966 ) ) ;
#20402 = CARTESIAN_POINT ( 'NONE',  ( 98.15313185440925281, 4.458734125000016313, 8.500000001365592084 ) ) ;
#20403 = CARTESIAN_POINT ( 'NONE',  ( 99.99999999999998579, 117.3602355696678643, -53.00000000546238255 ) ) ;
#20404 = CARTESIAN_POINT ( 'NONE',  ( 103.1528011352953342, 3.152801135295383084, 12.06250000136559208 ) ) ;
#20405 = CARTESIAN_POINT ( 'NONE',  ( 106.5389055433251002, 105.2492070361643215, -46.32500000273119412 ) ) ;
#20406 = CARTESIAN_POINT ( 'NONE',  ( 104.4587341249999923, 91.62499999863440792, -1.846868145590737198 ) ) ;
#20407 = CARTESIAN_POINT ( 'NONE',  ( 97.92893218813451028, 5.000000000000018652, 3.812500000000000000 ) ) ;
#20408 = CARTESIAN_POINT ( 'NONE',  ( -20.00000000000000000, 55.00000000000000000, 15.00000000000000178 ) ) ;
#20409 = CARTESIAN_POINT ( 'NONE',  ( -13.14518615778179900, 32.76484375108393010, -5.444914386472297529 ) ) ;
#20410 = ORIENTED_EDGE ( 'NONE', *, *, #25719, .T. ) ;
#20411 = SURFACE_STYLE_USAGE ( .BOTH. , #11687 ) ;
#20412 = LINE ( 'NONE', #7717, #2937 ) ;
#20413 = LINE ( 'NONE', #9569, #21148 ) ;
#20414 = CARTESIAN_POINT ( 'NONE',  ( 200.4449143864723055, 36.83281250108392868, 13.14518615778179189 ) ) ;
#20415 = ORIENTED_EDGE ( 'NONE', *, *, #19264, .T. ) ;
#20416 = CARTESIAN_POINT ( 'NONE',  ( 202.6362410680037272, 54.91786508990981019, -15.00000000000000355 ) ) ;
#20417 = CARTESIAN_POINT ( 'NONE',  ( 104.4587341249999781, 1.846868145590750299, 9.250000001365593860 ) ) ;
#20418 = PRODUCT_RELATED_PRODUCT_CATEGORY ( 'part', '', ( #2399 ) ) ;
#20419 = EDGE_CURVE ( 'NONE', #5311, #19746, #4484, .T. ) ;
#20420 = ORIENTED_EDGE ( 'NONE', *, *, #21282, .F. ) ;
#20421 = CARTESIAN_POINT ( 'NONE',  ( 93.46109445667491400, 105.2492070361643215, -53.17500000273119554 ) ) ;
#20422 = CARTESIAN_POINT ( 'NONE',  ( -8.049105076161786076E-16, 35.59257812608393579, -13.14518615778179544 ) ) ;
#20423 = DIRECTION ( 'NONE',  ( -1.000000000000000000, 0.000000000000000000, 2.385244779468110248E-16 ) ) ;
#20424 = CARTESIAN_POINT ( 'NONE',  ( 98.23223304703363112, 123.5000000000000000, 1.767766952966351557 ) ) ;
#20425 = CIRCLE ( 'NONE', #13557, 13.57481594606304398 ) ;
#20426 = CARTESIAN_POINT ( 'NONE',  ( 139.2950502721270425, 37.87460937608393152, -9.295050272127046043 ) ) ;
#20427 = CARTESIAN_POINT ( 'NONE',  ( -9.295050272127044266, 39.26367187608393294, 9.295050272127047819 ) ) ;
#20428 = CARTESIAN_POINT ( 'NONE',  ( -5.444914386472299306, 35.14609375108393152, 13.14518615778179722 ) ) ;
#20429 = CARTESIAN_POINT ( 'NONE',  ( -13.14518615778179189, 36.03906250108394005, 5.444914386472304635 ) ) ;
#20430 = CARTESIAN_POINT ( 'NONE',  ( 95.54126587500000767, 91.06249999863440792, -7.484931351350258973E-15 ) ) ;
#20431 = CARTESIAN_POINT ( 'NONE',  ( 60.14150070953499494, 49.99999999891522862, -12.70434618648778446 ) ) ;
#20432 = CARTESIAN_POINT ( 'NONE',  ( 108.0825317500000153, 110.0000000000000000, -54.37500000273119838 ) ) ;
#20433 = ORIENTED_EDGE ( 'NONE', *, *, #451, .T. ) ;
#20434 = LINE ( 'NONE', #916, #27170 ) ;
#20435 =( BOUNDED_CURVE ( )  B_SPLINE_CURVE ( 2, ( #5649, #10038, #24889, #18750, #27450, #1101, #25299, #14454, #23171 ),
 .UNSPECIFIED., .F., .F. ) 
 B_SPLINE_CURVE_WITH_KNOTS ( ( 3, 2, 2, 2, 3 ),
 ( 0.7500000000000006661, 0.7750000000000006883, 0.8000000000000007105, 0.8250000000000007327, 0.8500000000000007550 ),
 .UNSPECIFIED. ) 
 CURVE ( )  GEOMETRIC_REPRESENTATION_ITEM ( )  RATIONAL_B_SPLINE_CURVE ( ( 0.9999999999999980016, 0.9238795325112887369, 1.000000000000000000, 0.9238795325112867385, 1.000000000000000000, 0.9238795325112867385, 1.000000000000000000, 0.9238795325112844070, 1.000000000000002442 ) ) 
 REPRESENTATION_ITEM ( '' )  );
#20436 = CARTESIAN_POINT ( 'NONE',  ( -9.295050272127044266, 34.50117187608393721, 9.295050272127047819 ) ) ;
#20437 = CARTESIAN_POINT ( 'NONE',  ( 96.84719886470459471, -3.152801135295355994, 6.812500001365592084 ) ) ;
#20438 = CARTESIAN_POINT ( 'NONE',  ( 65.00000000000000000, 37.18007812608393436, -13.14518615778179544 ) ) ;
#20439 = CARTESIAN_POINT ( 'NONE',  ( 99.99999999999998579, 91.12499999726880162, -4.999999999999997335 ) ) ;
#20440 = CARTESIAN_POINT ( 'NONE',  ( 200.4449143864723055, 37.13046875108393152, -13.14518615778179722 ) ) ;
#20441 = VERTEX_POINT ( 'NONE', #28006 ) ;
#20442 = CARTESIAN_POINT ( 'NONE',  ( 9.295050272127046043, 34.89804687608393863, -9.295050272127046043 ) ) ;
#20443 = ORIENTED_EDGE ( 'NONE', *, *, #112, .T. ) ;
#20444 = CARTESIAN_POINT ( 'NONE',  ( 101.4615807364564546, 124.0500000010924850, 1.461580736456455476 ) ) ;
#20445 = CARTESIAN_POINT ( 'NONE',  ( 101.8468681455907330, 91.74999999863439371, -4.458734124999994997 ) ) ;
#20446 = CARTESIAN_POINT ( 'NONE',  ( 208.1451861577818079, 39.56132812608393579, -1.609821015232357215E-15 ) ) ;
#20447 = CARTESIAN_POINT ( 'NONE',  ( 91.91746824999998466, 110.0000000000000000, -51.87499999726882294 ) ) ;
#20448 = ORIENTED_EDGE ( 'NONE', *, *, #13672, .T. ) ;
#20449 = CARTESIAN_POINT ( 'NONE',  ( -13.57481594606304753, 34.60039062499999574, -5.622872871577873077 ) ) ;
#20450 = CARTESIAN_POINT ( 'NONE',  ( -5.444914386472297529, 32.46718750108393436, -13.14518615778179900 ) ) ;
#20451 = ORIENTED_EDGE ( 'NONE', *, *, #23264, .T. ) ;
#20452 = CARTESIAN_POINT ( 'NONE',  ( 130.0000000000000000, 34.20351562608394147, -13.14518615778179544 ) ) ;
#20453 = CARTESIAN_POINT ( 'NONE',  ( 130.0000000000000000, 36.93203125216787441, -13.57481594606304576 ) ) ;
#20454 = CARTESIAN_POINT ( 'NONE',  ( 208.1451861577818079, 33.21132812608393436, -1.609821015232357215E-15 ) ) ;
#20455 = EDGE_LOOP ( 'NONE', ( #17462, #17668, #27534 ) ) ;
#20456 = CARTESIAN_POINT ( 'NONE',  ( 103.5355339059327093, 3.535533905932755072, 8.750000002731184168 ) ) ;
#20457 = PLANE ( 'NONE',  #17686 ) ;
#20458 = EDGE_CURVE ( 'NONE', #15008, #10223, #6885, .T. ) ;
#20459 = CARTESIAN_POINT ( 'NONE',  ( 120.4011555911795455, 37.82500000216787583, -9.598844408820458085 ) ) ;
#20460 = CARTESIAN_POINT ( 'NONE',  ( 108.0825317500000011, 112.6261737610028320, -50.02500000273118985 ) ) ;
#20461 = ADVANCED_FACE ( 'NONE', ( #26287, #15005 ), #4201, .F. ) ;
#20462 = CARTESIAN_POINT ( 'NONE',  ( 97.92893218813451028, -4.999999999999989342, 7.187499999999999112 ) ) ;
#20463 = CARTESIAN_POINT ( 'NONE',  ( 2.493653234604083739E-15, 34.15390625216787157, 13.57481594606304576 ) ) ;
#20464 = CARTESIAN_POINT ( 'NONE',  ( 67.02462772553560910, 50.00000000050971494, 13.43320860980923115 ) ) ;
#20465 = EDGE_LOOP ( 'NONE', ( #25991, #19868, #28183, #19607, #13289, #24867, #12393, #10667 ) ) ;
#20466 = ORIENTED_EDGE ( 'NONE', *, *, #5336, .F. ) ;
#20467 = PRESENTATION_STYLE_ASSIGNMENT (( #7476 ) ) ;
#20468 = STYLED_ITEM ( 'NONE', ( #2376 ), #11047 ) ;
#20469 = CARTESIAN_POINT ( 'NONE',  ( 103.1528011352953342, -3.152801135295355106, 2.812500001365592528 ) ) ;
#20470 = VERTEX_POINT ( 'NONE', #6471 ) ;
#20471 = CARTESIAN_POINT ( 'NONE',  ( 1.464337720320554093, 36.00000000000002842, -13.46163418879032037 ) ) ;
#20472 = CARTESIAN_POINT ( 'NONE',  ( 101.8468681455906903, -4.458734124999987891, 8.750000001365592084 ) ) ;
#20473 = FACE_OUTER_BOUND ( 'NONE', #10366, .T. ) ;
#20474 = AXIS2_PLACEMENT_3D ( 'NONE', #18115, #7275, #2736 ) ;
#20475 = ADVANCED_FACE ( 'NONE', ( #8749 ), #4065, .T. ) ;
#20476 = CARTESIAN_POINT ( 'NONE',  ( 104.9999999999999716, 94.81249999726880162, 2.071067811865467956 ) ) ;
#20477 = CARTESIAN_POINT ( 'NONE',  ( 65.00000000000000000, 32.61601562608393579, -13.14518615778179544 ) ) ;
#20478 = CARTESIAN_POINT ( 'NONE',  ( 195.0000000000000000, 38.02343749999999289, 13.57481594606304576 ) ) ;
#20479 = CARTESIAN_POINT ( 'NONE',  ( 9.598844408820456309, 40.70234374999999716, -9.598844408820458085 ) ) ;
#20480 = DIRECTION ( 'NONE',  ( -0.000000000000000000, -0.000000000000000000, -1.000000000000000000 ) ) ;
#20481 = CARTESIAN_POINT ( 'NONE',  ( -1.947325922082419059, 51.47162402670901571, 14.99999999999934452 ) ) ;
#20482 = CARTESIAN_POINT ( 'NONE',  ( 99.99999999999998579, 129.0000000000000000, -5.204170427930421283E-15 ) ) ;
#20483 = CARTESIAN_POINT ( 'NONE',  ( 139.5988444088204403, 33.55859375000000000, -9.598844408820458085 ) ) ;
#20484 = ORIENTED_EDGE ( 'NONE', *, *, #16124, .T. ) ;
#20485 = CARTESIAN_POINT ( 'NONE',  ( 107.0000000000000000, 110.0000000000000000, -52.00000000000001421 ) ) ;
#20486 = CARTESIAN_POINT ( 'NONE',  ( 9.295050272127047819, 33.90585937608393863, 9.295050272127046043 ) ) ;
#20487 = CARTESIAN_POINT ( 'NONE',  ( -13.57481594606304576, 34.74921875216787726, 0.000000000000000000 ) ) ;
#20488 = CARTESIAN_POINT ( 'NONE',  ( 104.9999999999999574, 2.071067811865491937, 8.687500002731184168 ) ) ;
#20489 = CARTESIAN_POINT ( 'NONE',  ( 124.5550856135277087, 34.84843750108393579, -13.14518615778179900 ) ) ;
#20490 = CARTESIAN_POINT ( 'NONE',  ( 78.14518615778179367, 40.10703125108393152, 5.444914386472293977 ) ) ;
#20491 = CARTESIAN_POINT ( 'NONE',  ( 99.99999999999995737, 80.25000000000000000, 4.999999999999990230 ) ) ;
#20492 = CARTESIAN_POINT ( 'NONE',  ( -9.295050272127046043, 37.27929687608393294, -9.295050272127046043 ) ) ;
#20493 = EDGE_CURVE ( 'NONE', #13180, #2621, #17441, .T. ) ;
#20494 = CARTESIAN_POINT ( 'NONE',  ( -13.14518615778179189, 33.65781250108393152, 5.444914386472304635 ) ) ;
#20495 = CARTESIAN_POINT ( 'NONE',  ( 214.9999999999999716, 80.00000000000000000, -10.00000000000000000 ) ) ;
#20496 = CARTESIAN_POINT ( 'NONE',  ( 108.0825317500000011, 110.0000000000000000, -52.87499999726882294 ) ) ;
#20497 = CARTESIAN_POINT ( 'NONE',  ( 13.57481594606304576, 39.90859375216787441, -1.662435489736055892E-15 ) ) ;
#20498 = CARTESIAN_POINT ( 'NONE',  ( 189.5550856135277229, 31.67343750108393863, -13.14518615778179900 ) ) ;
#20499 = CARTESIAN_POINT ( 'NONE',  ( 0.000000000000000000, 40.99999999999999289, 0.000000000000000000 ) ) ;
#20500 = LINE ( 'NONE', #14199, #1426 ) ;
#20501 = ADVANCED_FACE ( 'NONE', ( #21589 ), #21452, .T. ) ;
#20502 = CARTESIAN_POINT ( 'NONE',  ( -20.00000000000000355, 55.00000000000000000, -9.999999999999998224 ) ) ;
#20503 = CARTESIAN_POINT ( 'NONE',  ( -9.598844408820454532, 35.54296874999999289, 9.598844408820459861 ) ) ;
#20504 = CARTESIAN_POINT ( 'NONE',  ( 102.0710678118654329, 5.000000000000018652, 12.68750000000000178 ) ) ;
#20505 = CARTESIAN_POINT ( 'NONE',  ( -9.598844408820458085, 32.96328124999999432, -9.598844408820458085 ) ) ;
#20506 = CARTESIAN_POINT ( 'NONE',  ( -9.598844408820454532, 33.16171874999999858, 9.598844408820459861 ) ) ;
#20507 = CARTESIAN_POINT ( 'NONE',  ( -13.14518615778179544, 35.19570312608393436, 0.000000000000000000 ) ) ;
#20508 = CARTESIAN_POINT ( 'NONE',  ( 13.14518615778179544, 33.01289062608393010, -1.609821015232357215E-15 ) ) ;
#20509 = CARTESIAN_POINT ( 'NONE',  ( -13.14518615778179544, 34.99726562608393721, 0.000000000000000000 ) ) ;
#20510 = EDGE_CURVE ( 'NONE', #778, #7715, #21877, .T. ) ;
#20511 = CARTESIAN_POINT ( 'NONE',  ( -13.57481594606304576, 37.13046875216787868, 0.000000000000000000 ) ) ;
#20512 = CARTESIAN_POINT ( 'NONE',  ( 13.57481594606304753, 37.57695312716787583, -5.622872871577873966 ) ) ;
#20513 = CARTESIAN_POINT ( 'NONE',  ( 99.99999999999998579, 97.00000000000000000, 2.999999999999982681 ) ) ;
#20514 = CARTESIAN_POINT ( 'NONE',  ( 51.85481384221820633, 33.45937500108392726, 5.444914386472304635 ) ) ;
#20515 = CARTESIAN_POINT ( 'NONE',  ( 104.9952793366501851, 116.8754121666685393, -54.07500000273119412 ) ) ;
#20516 = CARTESIAN_POINT ( 'NONE',  ( 99.99999999999998579, 94.25000000000000000, -4.999999999999997335 ) ) ;
#20517 = CARTESIAN_POINT ( 'NONE',  ( 100.8561741729129153, 124.3000000010924708, -2.066987299999999195 ) ) ;
#20518 = CARTESIAN_POINT ( 'NONE',  ( -13.57481594606304576, 34.64999999999999147, 0.000000000000000000 ) ) ;
#20519 = CARTESIAN_POINT ( 'NONE',  ( 99.99999999999997158, 101.5015231886685854, -55.37499999726883004 ) ) ;
#20520 = CARTESIAN_POINT ( 'NONE',  ( 143.1451861577818079, 33.16171875108393863, 5.444914386472293977 ) ) ;
#20521 = B_SPLINE_CURVE_WITH_KNOTS ( 'NONE', 3,
 ( #21053, #3672, #1537, #8068, #18900, #1122, #5670, #23053, #3802, #12334, #27205, #16763, #5534, #5390, #14335, #12186, #16487, #19036, #5808, #12050, #5943, #7931, #7510, #25465, #14611, #10329, #14060, #20776, #20915, #10058, #23328 ),
 .UNSPECIFIED., .F., .F.,
 ( 4, 2, 2, 2, 2, 2, 2, 2, 2, 2, 1, 2, 2, 2, 2, 4 ),
 ( 9.214435701904187837E-16, 0.001647793485001483246, 0.003295586970002045354, 0.004943380455002607463, 0.005767277197502887649, 0.006591173940003168703, 0.008238967425003728209, 0.009886760910004286848, 0.01318234788000540413, 0.01483014136500596276, 0.01647793485000652314, 0.01812572833500708178, 0.01977352182000764041, 0.02306910879000876116, 0.02471690227500931286, 0.02636469576000986109 ),
 .UNSPECIFIED. ) ;
#20522 = ORIENTED_EDGE ( 'NONE', *, *, #27226, .F. ) ;
#20523 = CARTESIAN_POINT ( 'NONE',  ( 104.3262379212492590, 115.9545556584642867, -50.70000000000000284 ) ) ;
#20524 = AXIS2_PLACEMENT_3D ( 'NONE', #27765, #28177, #23622 ) ;
#20525 = CARTESIAN_POINT ( 'NONE',  ( 204.5988444088204403, 36.83281250216787583, -9.598844408820458085 ) ) ;
#20526 = CARTESIAN_POINT ( 'NONE',  ( 95.54126587499996504, 83.43750000136560629, -1.387778780781445676E-14 ) ) ;
#20527 = CARTESIAN_POINT ( 'NONE',  ( 96.46446609406726225, 94.37500000000000000, -3.535533905932738197 ) ) ;
#20528 = CARTESIAN_POINT ( 'NONE',  ( 51.42518405393695957, 38.71796875216787726, 0.000000000000000000 ) ) ;
#20529 = CARTESIAN_POINT ( 'NONE',  ( 104.3262379212492448, 104.0454443415356991, -54.30000000000001137 ) ) ;
#20530 = CARTESIAN_POINT ( 'NONE',  ( 204.2950502721270425, 40.25585937608393294, 9.295050272127046043 ) ) ;
#20531 = CARTESIAN_POINT ( 'NONE',  ( 13.57481594606304753, 39.95820312716787726, -5.622872871577873077 ) ) ;
#20532 = ORIENTED_EDGE ( 'NONE', *, *, #27487, .T. ) ;
#20533 = CARTESIAN_POINT ( 'NONE',  ( 182.1404900439225116, 36.00000000000000711, -3.245221471866913010 ) ) ;
#20534 = CARTESIAN_POINT ( 'NONE',  ( 102.0710678118654329, -4.999999999999989342, 11.31249999999999822 ) ) ;
#20535 = ORIENTED_EDGE ( 'NONE', *, *, #13284, .T. ) ;
#20536 = CARTESIAN_POINT ( 'NONE',  ( -5.444914386472299306, 37.72578125108395142, 13.14518615778179722 ) ) ;
#20537 = CARTESIAN_POINT ( 'NONE',  ( 198.8783854107797424, 31.34156310770110565, -13.57481594606304931 ) ) ;
#20538 = CARTESIAN_POINT ( 'NONE',  ( 9.295050272127046043, 33.90585937608393152, -9.295050272127046043 ) ) ;
#20539 = EDGE_CURVE ( 'NONE', #17753, #15719, #15268, .T. ) ;
#20540 = CARTESIAN_POINT ( 'NONE',  ( 103.5355339059327093, 3.535533905932755072, 13.75000000273118594 ) ) ;
#20541 = DIRECTION ( 'NONE',  ( -0.000000000000000000, -1.000000000000000000, -0.000000000000000000 ) ) ;
#20542 = CARTESIAN_POINT ( 'NONE',  ( -8.049105076161786076E-16, 31.82226562608393650, -13.14518615778179544 ) ) ;
#20543 = CARTESIAN_POINT ( 'NONE',  ( 143.1451861577818079, 32.16953125108393152, 5.444914386472293977 ) ) ;
#20544 = CARTESIAN_POINT ( 'NONE',  ( 103.1528011352953484, 91.43749999863440792, -3.152801135295366208 ) ) ;
#20545 = CARTESIAN_POINT ( 'NONE',  ( 98.23223304703363112, 124.2999999999999972, 1.767766952966351557 ) ) ;
#20546 = APPLICATION_PROTOCOL_DEFINITION ( 'draft international standard', 'automotive_design', 1998, #3514 ) ;
#20547 = DIRECTION ( 'NONE',  ( 0.000000000000000000, -0.000000000000000000, 1.000000000000000000 ) ) ;
#20548 = CARTESIAN_POINT ( 'NONE',  ( 103.1528011352953342, -3.152801135295355106, 7.062500001365592972 ) ) ;
#20549 = CARTESIAN_POINT ( 'NONE',  ( 51.85481384221819923, 40.50390625108394005, -5.444914386472297529 ) ) ;
#20550 = AXIS2_PLACEMENT_3D ( 'NONE', #2197, #28130, #4327 ) ;
#20551 = CARTESIAN_POINT ( 'NONE',  ( 99.99999999999995737, 4.458734125000016313, 10.18750000136559208 ) ) ;
#20552 = CARTESIAN_POINT ( 'NONE',  ( 97.83688103937538472, 116.6573956140660897, -48.90000000546238113 ) ) ;
#20553 = CARTESIAN_POINT ( 'NONE',  ( 98.23223304703363112, 124.2000000021849502, -1.767766952966370209 ) ) ;
#20554 = CARTESIAN_POINT ( 'NONE',  ( 104.9999999999999716, 1.449011120738813565E-14, 4.499999999999999112 ) ) ;
#20555 = CARTESIAN_POINT ( 'NONE',  ( 99.99999999999998579, 90.00000000000000000, -6.938893903907228378E-15 ) ) ;
#20556 = CARTESIAN_POINT ( 'NONE',  ( -13.14518615778179544, 33.60820312608393579, 0.000000000000000000 ) ) ;
#20557 = VERTEX_POINT ( 'NONE', #10598 ) ;
#20558 = CARTESIAN_POINT ( 'NONE',  ( 99.99999999999998579, 110.0000000000000000, -145.0000000000000284 ) ) ;
#20559 = CARTESIAN_POINT ( 'NONE',  ( 9.598844408820459861, 39.80937500216786873, 9.598844408820456309 ) ) ;
#20560 = CARTESIAN_POINT ( 'NONE',  ( 104.9999999999999716, 1.449011120738813565E-14, 1.499999999999999556 ) ) ;
#20561 = CARTESIAN_POINT ( 'NONE',  ( 200.4449143864723055, 34.74921875108394431, -13.14518615778179900 ) ) ;
#20562 = EDGE_LOOP ( 'NONE', ( #12221, #5326 ) ) ;
#20563 =( BOUNDED_CURVE ( )  B_SPLINE_CURVE ( 2, ( #3566, #10370, #25220 ),
 .UNSPECIFIED., .F., .F. ) 
 B_SPLINE_CURVE_WITH_KNOTS ( ( 3, 3 ),
 ( 0.9375000000000000000, 0.9448586960708869054 ),
 .UNSPECIFIED. ) 
 CURVE ( )  GEOMETRIC_REPRESENTATION_ITEM ( )  RATIONAL_B_SPLINE_CURVE ( ( 1.000000000000000000, 0.9462258510377660192, 0.9684275648627984623 ) ) 
 REPRESENTATION_ITEM ( '' )  );
#20564 = CARTESIAN_POINT ( 'NONE',  ( 199.5715916325254966, 51.44262710531793203, -14.99999999999869083 ) ) ;
#20565 = CARTESIAN_POINT ( 'NONE',  ( 99.99999999999995737, 4.458734125000016313, 12.43750000136559208 ) ) ;
#20566 = ORIENTED_EDGE ( 'NONE', *, *, #9667, .T. ) ;
#20567 = CARTESIAN_POINT ( 'NONE',  ( 106.5389055433251002, 105.2492070361643215, -46.57500000273119412 ) ) ;
#20568 = CARTESIAN_POINT ( 'NONE',  ( -9.295050272127046043, 38.07304687608393579, -9.295050272127046043 ) ) ;
#20569 = CARTESIAN_POINT ( 'NONE',  ( 95.54126587499996504, 1.387778780781445676E-14, 14.68750000136559208 ) ) ;
#20570 = CARTESIAN_POINT ( 'NONE',  ( 139.2950502721270425, 37.08085937608393579, -9.295050272127046043 ) ) ;
#20571 = CARTESIAN_POINT ( 'NONE',  ( -5.444914386472299306, 38.51953125108393294, 13.14518615778179722 ) ) ;
#20572 = CARTESIAN_POINT ( 'NONE',  ( -13.14518615778179900, 40.70234375108393721, -5.444914386472297529 ) ) ;
#20573 = CARTESIAN_POINT ( 'NONE',  ( 95.54126587499999346, 91.99999999863439371, -1.846868145590737864 ) ) ;
#20574 = LINE ( 'NONE', #22991, #26453 ) ;
#20575 = CARTESIAN_POINT ( 'NONE',  ( 106.5389055433251002, 105.2492070361643215, -50.57500000273120122 ) ) ;
#20576 = CARTESIAN_POINT ( 'NONE',  ( -8.312177448680279460E-16, 38.51953125216787299, -13.57481594606304576 ) ) ;
#20577 = CARTESIAN_POINT ( 'NONE',  ( 13.14518615778179544, 35.59257812608393579, -1.609821015232357215E-15 ) ) ;
#20578 = CARTESIAN_POINT ( 'NONE',  ( 99.99999999999995737, 4.458734125000016313, 5.437500001365592972 ) ) ;
#20579 = CARTESIAN_POINT ( 'NONE',  ( 59.55508561352770158, 36.43593750108394147, -13.14518615778179722 ) ) ;
#20580 = CARTESIAN_POINT ( 'NONE',  ( 195.0000000000000000, 37.72578125216787726, -13.57481594606304576 ) ) ;
#20581 = CARTESIAN_POINT ( 'NONE',  ( 65.00000000000000000, 38.42031249999999432, -13.57481594606304576 ) ) ;
#20582 = CARTESIAN_POINT ( 'NONE',  ( 189.5550856135277229, 37.22968750108394431, -13.14518615778179722 ) ) ;
#20583 = CARTESIAN_POINT ( 'NONE',  ( -13.14518615778179722, 33.55859375108393294, -5.444914386472297529 ) ) ;
#20584 = EDGE_CURVE ( 'NONE', #4924, #20673, #1987, .T. ) ;
#20585 = CARTESIAN_POINT ( 'NONE',  ( 102.4999999999999858, 122.3000000021849587, -9.847140817659276890E-15 ) ) ;
#20586 = CARTESIAN_POINT ( 'NONE',  ( 103.1528011352953484, 91.68749999863440792, -3.152801135295366208 ) ) ;
#20587 = CARTESIAN_POINT ( 'NONE',  ( 189.5550856135277229, 37.42812500108394147, -13.14518615778179722 ) ) ;
#20588 = CARTESIAN_POINT ( 'NONE',  ( 106.5389055433250860, 114.7507929638356785, -52.67499999726882010 ) ) ;
#20589 = CARTESIAN_POINT ( 'NONE',  ( -5.622872871577873077, 32.91367187499999858, -13.57481594606304753 ) ) ;
#20590 = CARTESIAN_POINT ( 'NONE',  ( -9.295050272127044266, 35.09648437608392868, 9.295050272127047819 ) ) ;
#20591 = VERTEX_POINT ( 'NONE', #6198 ) ;
#20592 = CARTESIAN_POINT ( 'NONE',  ( 99.99999999999997158, 117.3602355696678501, -45.50000000000001421 ) ) ;
#20593 = CARTESIAN_POINT ( 'NONE',  ( 97.92893218813451028, -4.999999999999989342, 0.3125000027311853334 ) ) ;
#20594 = DIRECTION ( 'NONE',  ( 6.123233995736778362E-17, 0.8660254037844380415, -0.5000000000000009992 ) ) ;
#20595 = CARTESIAN_POINT ( 'NONE',  ( 181.8548138422181921, 33.65781250108393152, 5.444914386472304635 ) ) ;
#20596 = ORIENTED_EDGE ( 'NONE', *, *, #21552, .T. ) ;
#20597 = DIRECTION ( 'NONE',  ( -0.000000000000000000, 1.000000000000000000, -0.000000000000000000 ) ) ;
#20598 = CARTESIAN_POINT ( 'NONE',  ( 9.180175813647991845, 50.00000000000000000, -9.999999999999996447 ) ) ;
#20599 = PLANE ( 'NONE',  #17168 ) ;
#20600 = CARTESIAN_POINT ( 'NONE',  ( 116.4251840539369596, 37.18007812716787441, 5.622872871577880183 ) ) ;
#20601 =( BOUNDED_CURVE ( )  B_SPLINE_CURVE ( 2, ( #20463, #24590, #658, #16020, #13735, #9330, #20315, #18025, #22459 ),
 .UNSPECIFIED., .F., .F. ) 
 B_SPLINE_CURVE_WITH_KNOTS ( ( 3, 2, 2, 2, 3 ),
 ( 0.6458333333333333703, 0.6562500000000000000, 0.6666666666666665186, 0.6770833333333332593, 0.6874999999999997780 ),
 .UNSPECIFIED. ) 
 CURVE ( )  GEOMETRIC_REPRESENTATION_ITEM ( )  RATIONAL_B_SPLINE_CURVE ( ( 1.000000000000000000, 0.9238795325112867385, 1.000000000000000000, 0.9238795325112867385, 1.000000000000000000, 0.9238795325112867385, 1.000000000000000000, 0.9238795325112884038, 0.9999999999999983347 ) ) 
 REPRESENTATION_ITEM ( '' )  );
#20602 = CARTESIAN_POINT ( 'NONE',  ( 104.9999999999999716, 1.449011120738813565E-14, 7.500000000000000000 ) ) ;
#20603 = CARTESIAN_POINT ( 'NONE',  ( -8.312177448680279460E-16, 34.55078125216787299, -13.57481594606304576 ) ) ;
#20604 = CARTESIAN_POINT ( 'NONE',  ( 204.2950502721270425, 40.45429687608393721, -9.295050272127046043 ) ) ;
#20605 = ORIENTED_EDGE ( 'NONE', *, *, #11904, .T. ) ;
#20606 = ORIENTED_EDGE ( 'NONE', *, *, #24542, .T. ) ;
#20607 = CARTESIAN_POINT ( 'NONE',  ( 101.8468681455906903, 4.458734125000016313, 3.125000001365592528 ) ) ;
#20608 = VERTEX_POINT ( 'NONE', #6747 ) ;
#20609 = CARTESIAN_POINT ( 'NONE',  ( 97.92893218813451028, 5.000000000000018652, 12.93750000273118772 ) ) ;
#20610 = CARTESIAN_POINT ( 'NONE',  ( 103.1528011352953342, 3.152801135295383084, 3.062500001365592528 ) ) ;
#20611 = FACE_OUTER_BOUND ( 'NONE', #21469, .T. ) ;
#20612 = CARTESIAN_POINT ( 'NONE',  ( -7.778504368121734736, 35.99999999999997868, 10.60546543669443231 ) ) ;
#20613 = CARTESIAN_POINT ( 'NONE',  ( 74.59884440882045453, 37.42812500216787441, 9.598844408820456309 ) ) ;
#20614 = CARTESIAN_POINT ( 'NONE',  ( 112.9999999999999858, 102.0000000000000142, -13.00000000000000711 ) ) ;
#20615 = CARTESIAN_POINT ( 'NONE',  ( 99.99999999999998579, 101.5015231886685854, -44.62500000273119838 ) ) ;
#20616 = CARTESIAN_POINT ( 'NONE',  ( -9.598844408820458085, 38.51953124999999289, -9.598844408820458085 ) ) ;
#20617 = LINE ( 'NONE', #24890, #5300 ) ;
#20618 = CARTESIAN_POINT ( 'NONE',  ( -1.138768117105833477, 50.00000000043849013, 13.56816686242529357 ) ) ;
#20619 = CARTESIAN_POINT ( 'NONE',  ( 135.6228728715778971, 35.69179687499999432, 13.57481594606304576 ) ) ;
#20620 = VECTOR ( 'NONE', #18172, 1000.000000000000000 ) ;
#20621 = ORIENTED_EDGE ( 'NONE', *, *, #22413, .T. ) ;
#20622 = FACE_BOUND ( 'NONE', #5124, .T. ) ;
#20623 = EDGE_CURVE ( 'NONE', #12114, #13023, #15433, .T. ) ;
#20624 = CARTESIAN_POINT ( 'NONE',  ( 9.295050272127046043, 33.31054687608394005, -9.295050272127046043 ) ) ;
#20625 = CARTESIAN_POINT ( 'NONE',  ( -8.312177448680279460E-16, 33.75703125216787726, -13.57481594606304576 ) ) ;
#20626 = APPLICATION_CONTEXT ( 'automotive_design' ) ;
#20627 = CARTESIAN_POINT ( 'NONE',  ( 99.99999999999995737, -4.999999999999990230, 7.375000002731185944 ) ) ;
#20628 = CARTESIAN_POINT ( 'NONE',  ( 130.0000000000000000, 33.21132812608393436, -13.14518615778179544 ) ) ;
#20629 = CARTESIAN_POINT ( 'NONE',  ( 51.85481384221819923, 38.91640625108393436, -5.444914386472297529 ) ) ;
#20630 = ORIENTED_EDGE ( 'NONE', *, *, #16138, .T. ) ;
#20631 = CARTESIAN_POINT ( 'NONE',  ( 9.598844408820459861, 37.42812500216787441, 9.598844408820456309 ) ) ;
#20632 = CARTESIAN_POINT ( 'NONE',  ( -5.444914386472297529, 38.02343750108394005, -13.14518615778179900 ) ) ;
#20633 = CARTESIAN_POINT ( 'NONE',  ( 13.14518615778179722, 33.16171875108393863, 5.444914386472293977 ) ) ;
#20634 = CYLINDRICAL_SURFACE ( 'NONE', #10754, 4.999999999999999112 ) ;
#20635 = CARTESIAN_POINT ( 'NONE',  ( 97.50236033167490746, 102.3130555110000159, -51.47499999726882436 ) ) ;
#20636 = CARTESIAN_POINT ( 'NONE',  ( -13.57481594606304576, 37.92421875216787441, 0.000000000000000000 ) ) ;
#20637 = CARTESIAN_POINT ( 'NONE',  ( 99.99999999999995737, 81.37500000273119838, 4.999999999999990230 ) ) ;
#20638 = FACE_OUTER_BOUND ( 'NONE', #27644, .T. ) ;
#20639 = CARTESIAN_POINT ( 'NONE',  ( 102.1631189606246295, 103.3426043859339103, -52.40000000000001279 ) ) ;
#20640 = CARTESIAN_POINT ( 'NONE',  ( 102.0669872999999939, 124.1000000010924964, 0.8561741729129311862 ) ) ;
#20641 = CARTESIAN_POINT ( 'NONE',  ( 185.4011555911795313, 39.31328124999999574, -9.598844408820458085 ) ) ;
#20642 = EDGE_CURVE ( 'NONE', #2199, #16509, #4624, .T. ) ;
#20643 = CARTESIAN_POINT ( 'NONE',  ( 95.67376207875072680, 104.0454443415356991, -47.70000000000000284 ) ) ;
#20644 = CARTESIAN_POINT ( 'NONE',  ( 95.54126587499996504, 79.43750000136559208, -1.387778780781445676E-14 ) ) ;
#20645 = CARTESIAN_POINT ( 'NONE',  ( -13.57481594606304576, 35.44374999999999432, 0.000000000000000000 ) ) ;
#20646 = CARTESIAN_POINT ( 'NONE',  ( -8.669112105337029917, 36.00000000000002842, -10.16963847934323262 ) ) ;
#20647 = CARTESIAN_POINT ( 'NONE',  ( -9.295050272127044266, 33.70742187608393436, 9.295050272127047819 ) ) ;
#20648 = CARTESIAN_POINT ( 'NONE',  ( -13.14518615778179900, 31.77265625108393365, -5.444914386472297529 ) ) ;
#20649 = CARTESIAN_POINT ( 'NONE',  ( 204.5988444088204403, 32.76484374999999716, -9.598844408820458085 ) ) ;
#20650 = CARTESIAN_POINT ( 'NONE',  ( -5.622872871577873077, 35.69179687716786731, 13.57481594606304753 ) ) ;
#20651 = CARTESIAN_POINT ( 'NONE',  ( 2.493653234604083739E-15, 36.43593749999999432, 13.57481594606304576 ) ) ;
#20652 = DIRECTION ( 'NONE',  ( -0.000000000000000000, -0.000000000000000000, -1.000000000000000000 ) ) ;
#20653 = CARTESIAN_POINT ( 'NONE',  ( 65.00000000000000000, 32.81445312608393294, 13.14518615778179544 ) ) ;
#20654 = LINE ( 'NONE', #22935, #27603 ) ;
#20655 = DIRECTION ( 'NONE',  ( 0.8660254037844407060, 0.4999999999999963363, 0.000000000000000000 ) ) ;
#20656 = EDGE_CURVE ( 'NONE', #19872, #17571, #14540, .T. ) ;
#20657 = CARTESIAN_POINT ( 'NONE',  ( 99.14382582708707048, 123.9000000010924794, 2.066987299999979211 ) ) ;
#20658 = CARTESIAN_POINT ( 'NONE',  ( -5.622872871577873077, 34.00507812499999716, 13.57481594606304753 ) ) ;
#20659 = CARTESIAN_POINT ( 'NONE',  ( 97.50236033167490746, 117.6869444889999841, -54.27499999726882862 ) ) ;
#20660 = CARTESIAN_POINT ( 'NONE',  ( 143.1451861577818079, 34.00507812608393721, -1.609821015232357215E-15 ) ) ;
#20661 = ORIENTED_EDGE ( 'NONE', *, *, #17718, .T. ) ;
#20662 = CARTESIAN_POINT ( 'NONE',  ( 97.83688103937538472, 116.6573956140660897, -50.40000000000000568 ) ) ;
#20663 = EDGE_CURVE ( 'NONE', #487, #13578, #9808, .T. ) ;
#20664 = DIRECTION ( 'NONE',  ( 0.000000000000000000, 0.000000000000000000, 1.000000000000000000 ) ) ;
#20665 = CARTESIAN_POINT ( 'NONE',  ( 103.1528011352953342, 81.81250000136559208, 3.152801135295355106 ) ) ;
#20666 = CARTESIAN_POINT ( 'NONE',  ( 104.9999999999999716, 91.93749999999998579, 2.071067811865467956 ) ) ;
#20667 = CARTESIAN_POINT ( 'NONE',  ( 120.4011555911795455, 38.71796874999999716, 9.598844408820459861 ) ) ;
#20668 = EDGE_CURVE ( 'NONE', #20336, #20844, #9597, .T. ) ;
#20669 = VECTOR ( 'NONE', #23602, 1000.000000000000000 ) ;
#20670 = CARTESIAN_POINT ( 'NONE',  ( 95.67376207875069838, 115.9545556584642867, -53.30000000000000426 ) ) ;
#20671 = CARTESIAN_POINT ( 'NONE',  ( 208.1451861577818079, 40.35507812608393863, -1.609821015232357215E-15 ) ) ;
#20672 = CARTESIAN_POINT ( 'NONE',  ( -8.312177448680279460E-16, 40.10703125216787157, -13.57481594606304576 ) ) ;
#20673 = VERTEX_POINT ( 'NONE', #13718 ) ;
#20674 = CARTESIAN_POINT ( 'NONE',  ( 94.99999999999995737, 2.071067811865491048, 7.937500000000000888 ) ) ;
#20675 = EDGE_CURVE ( 'NONE', #17432, #19989, #1827, .T. ) ;
#20676 = VERTEX_POINT ( 'NONE', #24571 ) ;
#20677 = CARTESIAN_POINT ( 'NONE',  ( 5.444914386472302859, 32.26875000108393721, 13.14518615778179189 ) ) ;
#20678 = CARTESIAN_POINT ( 'NONE',  ( 208.1451861577817795, 39.31328125108392868, 5.444914386472293977 ) ) ;
#20679 = DIRECTION ( 'NONE',  ( -0.000000000000000000, 1.000000000000000000, -0.000000000000000000 ) ) ;
#20680 = CARTESIAN_POINT ( 'NONE',  ( 104.9999999999999574, 2.071067811865511032, 0.6875000027311864992 ) ) ;
#20681 = LINE ( 'NONE', #2860, #1634 ) ;
#20682 = CARTESIAN_POINT ( 'NONE',  ( 9.295050272127046043, 32.51679687608393721, -9.295050272127046043 ) ) ;
#20683 = CARTESIAN_POINT ( 'NONE',  ( 143.5748159460630688, 37.42812499999999432, -1.662435489736055892E-15 ) ) ;
#20684 = CARTESIAN_POINT ( 'NONE',  ( 95.54126587499999346, 90.87499999863439371, 1.846868145590722543 ) ) ;
#20685 = CARTESIAN_POINT ( 'NONE',  ( 99.99999999999998579, 123.6000000000000085, 2.499999999999978684 ) ) ;
#20686 = EDGE_CURVE ( 'NONE', #5734, #24831, #12699, .T. ) ;
#20687 = DIRECTION ( 'NONE',  ( 1.000000000000000000, 0.000000000000000000, 0.000000000000000000 ) ) ;
#20688 = CARTESIAN_POINT ( 'NONE',  ( 117.2616098421445230, 35.99999999999998579, 3.273369733618576305 ) ) ;
#20689 = CARTESIAN_POINT ( 'NONE',  ( 98.15313185440925281, -4.458734124999987891, 7.875000001365591196 ) ) ;
#20690 = CARTESIAN_POINT ( 'NONE',  ( 0.000000000000000000, -7.395377635281828788, 13.57481594606304398 ) ) ;
#20691 = CARTESIAN_POINT ( 'NONE',  ( 98.15313185440923860, -4.458734124999987891, 11.62500000136559031 ) ) ;
#20692 = CARTESIAN_POINT ( 'NONE',  ( 105.6631189606246295, 105.8855032339526758, -47.70000000546237828 ) ) ;
#20693 = CARTESIAN_POINT ( 'NONE',  ( 99.99999999999998579, 124.1000000021849416, -2.499999999999997780 ) ) ;
#20694 = CARTESIAN_POINT ( 'NONE',  ( 97.92893218813451028, -4.999999999999989342, 9.187500000000000000 ) ) ;
#20695 = CARTESIAN_POINT ( 'NONE',  ( 97.50236033167490746, 102.3130555110000159, -55.22499999726881725 ) ) ;
#20696 = CARTESIAN_POINT ( 'NONE',  ( 5.444914386472302859, 33.85625000108393579, 13.14518615778179189 ) ) ;
#20697 = ORIENTED_EDGE ( 'NONE', *, *, #21846, .F. ) ;
#20698 = LINE ( 'NONE', #26976, #17274 ) ;
#20699 = VECTOR ( 'NONE', #19556, 1000.000000000000000 ) ;
#20700 = ADVANCED_FACE ( 'NONE', ( #8021 ), #23284, .T. ) ;
#20701 = CARTESIAN_POINT ( 'NONE',  ( 99.99999999999998579, 91.25000000000000000, -4.999999999999997335 ) ) ;
#20702 = EDGE_CURVE ( 'NONE', #19327, #23304, #5618, .T. ) ;
#20703 = CARTESIAN_POINT ( 'NONE',  ( 204.2950502721270425, 32.91367187608393152, 9.295050272127046043 ) ) ;
#20704 = ORIENTED_EDGE ( 'NONE', *, *, #769, .T. ) ;
#20705 = CARTESIAN_POINT ( 'NONE',  ( 190.4951129136680947, 51.44650206076642007, -14.99999999999734968 ) ) ;
#20706 = CARTESIAN_POINT ( 'NONE',  ( 98.15313185440925281, 4.458734125000016313, 7.500000001365592084 ) ) ;
#20707 = ORIENTED_EDGE ( 'NONE', *, *, #1899, .T. ) ;
#20708 = CARTESIAN_POINT ( 'NONE',  ( 102.4976396683250925, 102.3130555110000159, -48.77500000273119696 ) ) ;
#20709 = CARTESIAN_POINT ( 'NONE',  ( -13.14518615778179189, 36.63437500108393152, 5.444914386472304635 ) ) ;
#20710 = CARTESIAN_POINT ( 'NONE',  ( 185.4011555911795313, 39.41250000216787441, -9.598844408820458085 ) ) ;
#20711 = DIRECTION ( 'NONE',  ( 0.000000000000000000, 0.000000000000000000, 1.000000000000000000 ) ) ;
#20712 = CARTESIAN_POINT ( 'NONE',  ( 116.8548138422182063, 38.91640625108393436, -5.444914386472297529 ) ) ;
#20713 = CARTESIAN_POINT ( 'NONE',  ( 2.414731522848535132E-15, 36.98164062608393721, 13.14518615778179544 ) ) ;
#20714 = CARTESIAN_POINT ( 'NONE',  ( 9.295050272127047819, 40.25585937608393294, 9.295050272127046043 ) ) ;
#20715 = CARTESIAN_POINT ( 'NONE',  ( 98.15313185440925281, 90.87499999863439371, -4.458734124999994997 ) ) ;
#20716 = CARTESIAN_POINT ( 'NONE',  ( 100.0000000000000000, 110.0000000000000000, -55.00000000000000711 ) ) ;
#20717 = CARTESIAN_POINT ( 'NONE',  ( 70.62287287157778337, 38.07304687499999574, 13.57481594606313813 ) ) ;
#20718 = CARTESIAN_POINT ( 'NONE',  ( -9.295050272127046043, 34.30273437608393294, -9.295050272127046043 ) ) ;
#20719 = CARTESIAN_POINT ( 'NONE',  ( 103.1528011352953342, -3.152801135295355106, 8.062500001365592084 ) ) ;
#20720 =( BOUNDED_CURVE ( )  B_SPLINE_CURVE ( 2, ( #5543, #846, #20506, #3388, #989, #9657, #14067, #11924, #9798 ),
 .UNSPECIFIED., .F., .F. ) 
 B_SPLINE_CURVE_WITH_KNOTS ( ( 3, 2, 2, 2, 3 ),
 ( 0.8124999999999998890, 0.8229166666666665186, 0.8333333333333331483, 0.8437499999999997780, 0.8541666666666662966 ),
 .UNSPECIFIED. ) 
 CURVE ( )  GEOMETRIC_REPRESENTATION_ITEM ( )  RATIONAL_B_SPLINE_CURVE ( ( 1.000000000000000888, 0.9238795325112859613, 1.000000000000000000, 0.9238795325112867385, 1.000000000000000000, 0.9238795325112867385, 1.000000000000000000, 0.9238795325112891810, 0.9999999999999975575 ) ) 
 REPRESENTATION_ITEM ( '' )  );
#20721 = CARTESIAN_POINT ( 'NONE',  ( 99.99999999999995737, 84.43750000136560629, -4.458734125000016313 ) ) ;
#20722 = CARTESIAN_POINT ( 'NONE',  ( 97.92893218813451028, 5.000000000000018652, 6.937500002731185056 ) ) ;
#20723 = CARTESIAN_POINT ( 'NONE',  ( 99.99999999999998579, 110.0000000000000000, -45.00000000000000711 ) ) ;
#20724 = ORIENTED_EDGE ( 'NONE', *, *, #1041, .F. ) ;
#20725 = CARTESIAN_POINT ( 'NONE',  ( -13.14518615778179722, 35.93984375108393436, -5.444914386472297529 ) ) ;
#20726 = CARTESIAN_POINT ( 'NONE',  ( 101.7677669529663547, 123.0000000021849615, 1.767766952966350891 ) ) ;
#20727 = CARTESIAN_POINT ( 'NONE',  ( 98.15313185440923860, 93.87499999863439371, -4.458734124999994997 ) ) ;
#20728 = LINE ( 'NONE', #10013, #17281 ) ;
#20729 = CARTESIAN_POINT ( 'NONE',  ( 104.9952793366501709, 103.1245878333314323, -49.17499999726881299 ) ) ;
#20730 = VECTOR ( 'NONE', #26258, 1000.000000000000000 ) ;
#20731 = CARTESIAN_POINT ( 'NONE',  ( 130.0000000000000000, 39.31328125216787583, -13.57481594606304576 ) ) ;
#20732 = CARTESIAN_POINT ( 'NONE',  ( 6.944423797152705191, 31.55306878032414986, -11.16113333171310451 ) ) ;
#20733 = ORIENTED_EDGE ( 'NONE', *, *, #4785, .F. ) ;
#20734 = CARTESIAN_POINT ( 'NONE',  ( 185.4011555911795313, 37.03125000216787299, -9.598844408820458085 ) ) ;
#20735 = CARTESIAN_POINT ( 'NONE',  ( 2.493653234604083739E-15, 36.53515625216787299, 13.57481594606304576 ) ) ;
#20736 = CARTESIAN_POINT ( 'NONE',  ( 185.7049497278729575, 34.30273437608393294, -9.295050272127046043 ) ) ;
#20737 = ORIENTED_EDGE ( 'NONE', *, *, #15055, .T. ) ;
#20738 = CARTESIAN_POINT ( 'NONE',  ( 94.99999999999995737, 2.071067811865491493, 2.062500002731185056 ) ) ;
#20739 = CARTESIAN_POINT ( 'NONE',  ( 1.602533130612657564, 53.60343507248209249, -15.00000000000000000 ) ) ;
#20740 = AXIS2_PLACEMENT_3D ( 'NONE', #16626, #3670, #12332 ) ;
#20741 = CARTESIAN_POINT ( 'NONE',  ( 139.5988444088204687, 36.63437500216787157, 9.598844408820456309 ) ) ;
#20742 = EDGE_CURVE ( 'NONE', #6897, #26002, #6034, .T. ) ;
#20743 = CARTESIAN_POINT ( 'NONE',  ( 103.5355339059327093, -3.535533905932726206, 7.375000000000000000 ) ) ;
#20744 = CARTESIAN_POINT ( 'NONE',  ( 2.493653234604083739E-15, 31.77265625216787370, 13.57481594606304576 ) ) ;
#20745 = CARTESIAN_POINT ( 'NONE',  ( 200.4449143864723055, 37.03125000108393294, 13.14518615778179189 ) ) ;
#20746 = ORIENTED_EDGE ( 'NONE', *, *, #15588, .T. ) ;
#20747 = VECTOR ( 'NONE', #17149, 1000.000000000000227 ) ;
#20748 = ORIENTED_EDGE ( 'NONE', *, *, #23297, .F. ) ;
#20749 = CARTESIAN_POINT ( 'NONE',  ( 98.15313185440925281, 4.458734125000016313, 2.250000001365591640 ) ) ;
#20750 = CARTESIAN_POINT ( 'NONE',  ( -11.69037824551319460, 35.99999999999998579, -6.307928093363390332 ) ) ;
#20751 = CARTESIAN_POINT ( 'NONE',  ( 94.99999999999995737, 1.387778780781445676E-14, 13.99999999999999822 ) ) ;
#20752 = CARTESIAN_POINT ( 'NONE',  ( 51.42518405393695957, 40.99999999999999289, 0.000000000000000000 ) ) ;
#20753 = CARTESIAN_POINT ( 'NONE',  ( -13.14518615778179900, 40.70234375108393721, -5.444914386472297529 ) ) ;
#20754 = CARTESIAN_POINT ( 'NONE',  ( -13.57481594606304398, 39.56132812716787583, 5.622872871577880183 ) ) ;
#20755 = CARTESIAN_POINT ( 'NONE',  ( 13.04200858114998418, 36.00000000000000711, -3.640726557253423756 ) ) ;
#20756 = CARTESIAN_POINT ( 'NONE',  ( 8.769389672083836018, 50.37710889402394088, 14.99999999999737277 ) ) ;
#20757 = CARTESIAN_POINT ( 'NONE',  ( 124.3771271284221314, 35.29492187500000000, -13.57481594606304753 ) ) ;
#20758 = ORIENTED_EDGE ( 'NONE', *, *, #26932, .T. ) ;
#20759 = ORIENTED_EDGE ( 'NONE', *, *, #25297, .T. ) ;
#20760 = CARTESIAN_POINT ( 'NONE',  ( -8.312177448680279460E-16, 36.93203125216787441, -13.57481594606304576 ) ) ;
#20761 = CARTESIAN_POINT ( 'NONE',  ( -13.14518615778179189, 34.45156250108394147, 5.444914386472304635 ) ) ;
#20762 = CARTESIAN_POINT ( 'NONE',  ( 2.493653234604083739E-15, 33.36015625216786873, 13.57481594606304576 ) ) ;
#20763 = CARTESIAN_POINT ( 'NONE',  ( 99.99999999999995737, 5.000000000000018652, 4.875000002731185944 ) ) ;
#20764 = CARTESIAN_POINT ( 'NONE',  ( 130.0000000000000000, 38.17226562608394147, -13.14518615778179544 ) ) ;
#20765 = CARTESIAN_POINT ( 'NONE',  ( 74.29505027212704249, 40.25585937608393294, -9.295050272127046043 ) ) ;
#20766 =( BOUNDED_CURVE ( )  B_SPLINE_CURVE ( 2, ( #25814, #6288, #23685, #4162, #8706, #12822, #26097, #6562, #15242 ),
 .UNSPECIFIED., .F., .F. ) 
 B_SPLINE_CURVE_WITH_KNOTS ( ( 3, 2, 2, 2, 3 ),
 ( 0.3571428571428572063, 0.3660714285714286031, 0.3750000000000000000, 0.3839285714285714524, 0.3928571428571428492 ),
 .UNSPECIFIED. ) 
 CURVE ( )  GEOMETRIC_REPRESENTATION_ITEM ( )  RATIONAL_B_SPLINE_CURVE ( ( 0.9999999999999995559, 0.9238795325112871826, 1.000000000000000000, 0.9238795325112867385, 1.000000000000000000, 0.9238795325112867385, 1.000000000000000000, 0.9238795325112867385, 1.000000000000000000 ) ) 
 REPRESENTATION_ITEM ( '' )  );
#20767 = FACE_BOUND ( 'NONE', #13550, .T. ) ;
#20768 = CARTESIAN_POINT ( 'NONE',  ( 5.444914386472302859, 38.42031250108393436, 13.14518615778179189 ) ) ;
#20769 = CARTESIAN_POINT ( 'NONE',  ( -13.14518615778179722, 31.97109375108393792, -5.444914386472297529 ) ) ;
#20770 = FACE_OUTER_BOUND ( 'NONE', #17309, .T. ) ;
#20771 = CARTESIAN_POINT ( 'NONE',  ( 102.4976396683250783, 117.6869444889999841, -52.47499999726882436 ) ) ;
#20772 = ADVANCED_FACE ( 'NONE', ( #21137 ), #1623, .T. ) ;
#20773 = ORIENTED_EDGE ( 'NONE', *, *, #18554, .F. ) ;
#20774 = CARTESIAN_POINT ( 'NONE',  ( 204.2950502721270425, 32.11992187608393579, 9.295050272127046043 ) ) ;
#20775 = CIRCLE ( 'NONE', #8469, 2.999999999999989786 ) ;
#20776 = CARTESIAN_POINT ( 'NONE',  ( 142.8921516136354342, 35.99999999999997158, -4.169510824908009283 ) ) ;
#20777 = CARTESIAN_POINT ( 'NONE',  ( 98.23223304703363112, 123.5069999999781487, 1.767766952966351557 ) ) ;
#20778 = DIRECTION ( 'NONE',  ( 0.000000000000000000, 0.000000000000000000, 1.000000000000000000 ) ) ;
#20779 = CARTESIAN_POINT ( 'NONE',  ( 118.8544531269044029, 36.00000000000001421, -7.260818043106923803 ) ) ;
#20780 = CARTESIAN_POINT ( 'NONE',  ( 124.3771271284222308, 40.15664062716787441, -13.57481594606315412 ) ) ;
#20781 = CARTESIAN_POINT ( 'NONE',  ( 98.15313185440925281, 4.458734125000016313, 11.25000000136559031 ) ) ;
#20782 = CARTESIAN_POINT ( 'NONE',  ( -9.598844408820454532, 33.16171874999999858, 9.598844408820459861 ) ) ;
#20783 = ORIENTED_EDGE ( 'NONE', *, *, #24830, .F. ) ;
#20784 = LINE ( 'NONE', #9929, #3433 ) ;
#20785 = CARTESIAN_POINT ( 'NONE',  ( -5.444914386472297529, 32.66562500108393863, -13.14518615778179900 ) ) ;
#20786 = CARTESIAN_POINT ( 'NONE',  ( 2.414731522848535132E-15, 32.81445312608393294, 13.14518615778179544 ) ) ;
#20787 = CARTESIAN_POINT ( 'NONE',  ( 208.5748159460630688, 32.66562499999999858, -1.662435489736055892E-15 ) ) ;
#20788 = CARTESIAN_POINT ( 'NONE',  ( -13.57481594606304576, 34.00507812716787015, 5.622872871577880183 ) ) ;
#20789 = CARTESIAN_POINT ( 'NONE',  ( 94.99999999999995737, 1.387778780781445676E-14, 13.99999999999999822 ) ) ;
#20790 = CARTESIAN_POINT ( 'NONE',  ( 99.99999999999995737, 83.68750000136560629, 4.458734124999988779 ) ) ;
#20791 = CARTESIAN_POINT ( 'NONE',  ( 65.00000000000000000, 32.41757812608393863, -13.14518615778179544 ) ) ;
#20792 = CARTESIAN_POINT ( 'NONE',  ( 99.99999999999998579, 118.4984768113314004, -47.87500000273119127 ) ) ;
#20793 = CARTESIAN_POINT ( 'NONE',  ( 102.1631189606246295, 103.3426043859339103, -46.40000000000001279 ) ) ;
#20794 = ORIENTED_EDGE ( 'NONE', *, *, #16163, .F. ) ;
#20795 = CARTESIAN_POINT ( 'NONE',  ( 102.0669872999999939, 124.1000000010924964, 0.8561741729129311862 ) ) ;
#20796 = CARTESIAN_POINT ( 'NONE',  ( -5.622872871577873077, 34.50117187499999005, -13.57481594606304753 ) ) ;
#20797 = CARTESIAN_POINT ( 'NONE',  ( 104.9952793366501709, 116.8754121666685393, -52.57499999726881867 ) ) ;
#20798 = CARTESIAN_POINT ( 'NONE',  ( 139.2950502721270425, 33.90585937608393863, 9.295050272127046043 ) ) ;
#20799 = ORIENTED_EDGE ( 'NONE', *, *, #17684, .F. ) ;
#20800 = CARTESIAN_POINT ( 'NONE',  ( -6.079080020518830452, 54.65154858643462887, -14.99999999999999822 ) ) ;
#20801 = CARTESIAN_POINT ( 'NONE',  ( 99.99999999999998579, 92.25000000000000000, -4.999999999999997335 ) ) ;
#20802 = CARTESIAN_POINT ( 'NONE',  ( 96.84719886470459471, 83.56250000136560629, 3.152801135295355994 ) ) ;
#20803 = CARTESIAN_POINT ( 'NONE',  ( 2.493653234604083739E-15, 33.36015625216786873, 13.57481594606304576 ) ) ;
#20804 = CARTESIAN_POINT ( 'NONE',  ( 51.90409344636400846, 36.00000000000000000, 1.137167824541468031 ) ) ;
#20805 = CARTESIAN_POINT ( 'NONE',  ( 95.00472066334982912, 116.8754121666685393, -45.92499999726882720 ) ) ;
#20806 = CARTESIAN_POINT ( 'NONE',  ( 13.57481594606304753, 38.37070312716786447, -5.622872871577873077 ) ) ;
#20807 = ORIENTED_EDGE ( 'NONE', *, *, #20365, .T. ) ;
#20808 = CARTESIAN_POINT ( 'NONE',  ( 99.99999999999995737, 5.000000000000018652, 8.749999999999998224 ) ) ;
#20809 = ORIENTED_EDGE ( 'NONE', *, *, #10194, .T. ) ;
#20810 = CARTESIAN_POINT ( 'NONE',  ( -13.14518615778179900, 32.76484375108393010, -5.444914386472297529 ) ) ;
#20811 = CARTESIAN_POINT ( 'NONE',  ( 189.5550856135277229, 40.40468750108393436, -13.14518615778179900 ) ) ;
#20812 = AXIS2_PLACEMENT_3D ( 'NONE', #26679, #19682, #11398 ) ;
#20813 = EDGE_CURVE ( 'NONE', #25968, #6997, #3071, .T. ) ;
#20814 = CARTESIAN_POINT ( 'NONE',  ( 99.99999999999995737, 5.000000000000018652, 13.87500000273118594 ) ) ;
#20815 = CARTESIAN_POINT ( 'NONE',  ( 97.92893218813451028, -4.999999999999989342, 12.31250000273118772 ) ) ;
#20816 = CARTESIAN_POINT ( 'NONE',  ( 200.6228728715779255, 38.17226562716787441, 13.57481594606301023 ) ) ;
#20817 = CARTESIAN_POINT ( 'NONE',  ( 13.14518615778179544, 32.41757812608393863, -1.609821015232357215E-15 ) ) ;
#20818 = EDGE_CURVE ( 'NONE', #5192, #5473, #19947, .T. ) ;
#20819 = CARTESIAN_POINT ( 'NONE',  ( 103.5355339059327093, -3.535533905932726206, 11.37500000000000000 ) ) ;
#20820 = CARTESIAN_POINT ( 'NONE',  ( 51.42518405393695957, 32.26874999999999716, 0.000000000000000000 ) ) ;
#20821 = CARTESIAN_POINT ( 'NONE',  ( 101.4615807364564546, 123.6500000010924651, -1.461580736456474794 ) ) ;
#20822 = CARTESIAN_POINT ( 'NONE',  ( 181.8548138422181921, 32.76484375108393010, -5.444914386472297529 ) ) ;
#20823 = APPLICATION_PROTOCOL_DEFINITION ( 'draft international standard', 'automotive_design', 1998, #21529 ) ;
#20824 = CARTESIAN_POINT ( 'NONE',  ( 9.598844408820459861, 35.74140624999999716, 9.598844408820456309 ) ) ;
#20825 = CARTESIAN_POINT ( 'NONE',  ( 96.84719886470459471, -3.152801135295355994, 6.812500001365592084 ) ) ;
#20826 = SPHERICAL_SURFACE ( 'NONE', #13495, 5.000000000000000000 ) ;
#20827 = CARTESIAN_POINT ( 'NONE',  ( 96.84719886470459471, 3.152801135295383084, 9.312500001365593860 ) ) ;
#20828 = CARTESIAN_POINT ( 'NONE',  ( 107.0000000000000142, 112.2744378736303332, -49.40000000546237402 ) ) ;
#20829 = CARTESIAN_POINT ( 'NONE',  ( 104.4587341249999923, 95.49999999863442213, 1.846868145590726318 ) ) ;
#20830 = CARTESIAN_POINT ( 'NONE',  ( 2.493653234604083739E-15, 39.61093749999999147, 13.57481594606304576 ) ) ;
#20831 = CYLINDRICAL_SURFACE ( 'NONE', #10251, 13.57481594606304576 ) ;
#20832 = CARTESIAN_POINT ( 'NONE',  ( 2.414731522848535132E-15, 32.21914062608393436, 13.14518615778179544 ) ) ;
#20833 = ADVANCED_FACE ( 'NONE', ( #9111 ), #19279, .T. ) ;
#20834 = ORIENTED_EDGE ( 'NONE', *, *, #26766, .T. ) ;
#20835 = CARTESIAN_POINT ( 'NONE',  ( 103.1528011352953342, 82.31250000136559208, -3.152801135295383084 ) ) ;
#20836 = CIRCLE ( 'NONE', #27667, 13.57481594606304398 ) ;
#20838 = CARTESIAN_POINT ( 'NONE',  ( -8.312177448680279460E-16, 37.62656249999999858, -13.57481594606304576 ) ) ;
#20837 = AXIS2_PLACEMENT_3D ( 'NONE', #7293, #20423, #907 ) ;
#20839 = CARTESIAN_POINT ( 'NONE',  ( 181.8548138422181921, 34.15390625108393863, -5.444914386472297529 ) ) ;
#20840 = ORIENTED_EDGE ( 'NONE', *, *, #22765, .F. ) ;
#20841 = CARTESIAN_POINT ( 'NONE',  ( 194.0169348148962740, 49.99999999949044849, -13.54930971656736638 ) ) ;
#20842 = CARTESIAN_POINT ( 'NONE',  ( 98.15313185440925281, 4.458734125000016313, 6.500000001365592084 ) ) ;
#20843 = ADVANCED_FACE ( 'NONE', ( #25971 ), #2038, .F. ) ;
#20844 = VERTEX_POINT ( 'NONE', #22232 ) ;
#20845 = CARTESIAN_POINT ( 'NONE',  ( 97.50236033167492167, 117.6869444889999841, -47.77500000273119696 ) ) ;
#20846 = CARTESIAN_POINT ( 'NONE',  ( 9.295050272127047819, 32.11992187608393579, 9.295050272127046043 ) ) ;
#20847 = CARTESIAN_POINT ( 'NONE',  ( 185.4011555911795313, 38.61875000216787157, -9.598844408820458085 ) ) ;
#20848 = CARTESIAN_POINT ( 'NONE',  ( 107.0000000000000000, 110.0000000000000000, -54.00000000000001421 ) ) ;
#20849 = CARTESIAN_POINT ( 'NONE',  ( 13.14518615778179722, 38.02343750108395426, -5.444914386472297529 ) ) ;
#20850 = CARTESIAN_POINT ( 'NONE',  ( -5.444914386472297529, 40.60312500108393863, -13.14518615778179900 ) ) ;
#20851 = CARTESIAN_POINT ( 'NONE',  ( 103.1528011352953484, 90.68749999863440792, -3.152801135295366208 ) ) ;
#20852 = CARTESIAN_POINT ( 'NONE',  ( 195.0000000000000000, -7.395377635281828788, -2.255140518769849538E-14 ) ) ;
#20853 = EDGE_CURVE ( 'NONE', #10914, #20981, #17161, .T. ) ;
#20854 = VERTEX_POINT ( 'NONE', #14835 ) ;
#20855 = CARTESIAN_POINT ( 'NONE',  ( -8.049105076161786076E-16, 31.82226562608393650, -13.14518615778179544 ) ) ;
#20856 = CARTESIAN_POINT ( 'NONE',  ( 95.54126587499996504, 1.846868145590750077, 4.625000001365592084 ) ) ;
#20857 = CARTESIAN_POINT ( 'NONE',  ( 104.4587341249999781, 84.12500000136560629, 1.846868145590721655 ) ) ;
#20858 = CARTESIAN_POINT ( 'NONE',  ( 5.444914386472297529, 36.33671875108394289, -13.14518615778179900 ) ) ;
#20859 = DIRECTION ( 'NONE',  ( 0.000000000000000000, 1.000000000000000000, 0.000000000000000000 ) ) ;
#20860 = CARTESIAN_POINT ( 'NONE',  ( 65.32472431119603584, 53.49346745874647269, 14.99999999999997691 ) ) ;
#20861 = ORIENTED_EDGE ( 'NONE', *, *, #25711, .T. ) ;
#20862 = CARTESIAN_POINT ( 'NONE',  ( -13.14518615778179544, 34.40195312608393152, 0.000000000000000000 ) ) ;
#20863 = CARTESIAN_POINT ( 'NONE',  ( 99.99999999999998579, 122.9000000021849530, 2.499999999999978684 ) ) ;
#20864 = DIRECTION ( 'NONE',  ( -0.000000000000000000, 1.000000000000000000, -0.000000000000000000 ) ) ;
#20865 = CARTESIAN_POINT ( 'NONE',  ( 185.7049497278729575, 36.08867187608393579, 9.295050272127047819 ) ) ;
#20866 = CARTESIAN_POINT ( 'NONE',  ( 91.91746824999997045, 107.3738262389971538, -53.77499999726881441 ) ) ;
#20867 = DIRECTION ( 'NONE',  ( 5.782411586589357392E-17, -0.000000000000000000, 1.000000000000000000 ) ) ;
#20868 = EDGE_LOOP ( 'NONE', ( #20229, #27817 ) ) ;
#20869 = CARTESIAN_POINT ( 'NONE',  ( 74.29505027212704249, 39.46210937608393721, 9.295050272127046043 ) ) ;
#20870 = EDGE_LOOP ( 'NONE', ( #25128, #17478, #17136, #28046 ) ) ;
#20871 = CARTESIAN_POINT ( 'NONE',  ( 2.493653234604083739E-15, 38.12265625216787157, 13.57481594606304576 ) ) ;
#20872 = AXIS2_PLACEMENT_3D ( 'NONE', #9934, #12475, #25334 ) ;
#20873 = CARTESIAN_POINT ( 'NONE',  ( -2.743444426250911979E-15, 0.4999999999999970024, -22.40192378864669465 ) ) ;
#20874 = ORIENTED_EDGE ( 'NONE', *, *, #25719, .F. ) ;
#20875 = CARTESIAN_POINT ( 'NONE',  ( 97.83688103937538472, 116.6573956140660897, -54.40000000000000568 ) ) ;
#20876 = DIRECTION ( 'NONE',  ( 0.000000000000000000, 0.000000000000000000, -1.000000000000000000 ) ) ;
#20877 =( GEOMETRIC_REPRESENTATION_CONTEXT ( 3 ) GLOBAL_UNCERTAINTY_ASSIGNED_CONTEXT ( ( #8053 ) ) GLOBAL_UNIT_ASSIGNED_CONTEXT ( ( #16875, #19299, #15136 ) ) REPRESENTATION_CONTEXT ( 'NONE', 'WORKASPACE' ) );
#20878 = CYLINDRICAL_SURFACE ( 'NONE', #17230, 5.000000000000004441 ) ;
#20879 = CARTESIAN_POINT ( 'NONE',  ( 130.0000000000000000, 38.12265625216787157, 13.57481594606304576 ) ) ;
#20880 =( BOUNDED_CURVE ( )  B_SPLINE_CURVE ( 2, ( #12552, #12418, #14978, #16719, #21003, #14697, #10139, #23697, #21278, #27976, #10426 ),
 .UNSPECIFIED., .F., .T. ) 
 B_SPLINE_CURVE_WITH_KNOTS ( ( 3, 2, 2, 2, 2, 3 ),
 ( 0.6999999999999998446, 0.7199999999999998623, 0.7399999999999998801, 0.7600000000000000089, 0.7800000000000000266, 0.8000000000000000444 ),
 .UNSPECIFIED. ) 
 CURVE ( )  GEOMETRIC_REPRESENTATION_ITEM ( )  RATIONAL_B_SPLINE_CURVE ( ( 1.000000000000000222, 0.9510565162951533091, 1.000000000000000000, 0.9510565162951535312, 1.000000000000000000, 0.9510565162951535312, 1.000000000000000000, 0.9510565162951535312, 1.000000000000000000, 0.9510565162951535312, 1.000000000000000000 ) ) 
 REPRESENTATION_ITEM ( '' )  );
#20881 = DIRECTION ( 'NONE',  ( 0.000000000000000000, 1.000000000000000000, 0.000000000000000000 ) ) ;
#20882 = CARTESIAN_POINT ( 'NONE',  ( 0.000000000000000000, 0.000000000000000000, 0.000000000000000000 ) ) ;
#20883 = CARTESIAN_POINT ( 'NONE',  ( 204.2950502721270425, 37.08085937608393579, 9.295050272127046043 ) ) ;
#20884 = ORIENTED_EDGE ( 'NONE', *, *, #13236, .T. ) ;
#20885 = SHAPE_REPRESENTATION_RELATIONSHIP ( 'NONE' , 'NONE' ,  #26810, #19902 ) ;
#20886 = CARTESIAN_POINT ( 'NONE',  ( 98.15313185440925281, -4.458734124999987891, 13.87500000136559208 ) ) ;
#20887 = CARTESIAN_POINT ( 'NONE',  ( 101.8468681455907046, -4.458734124999987891, 14.00000000136559208 ) ) ;
#20888 = DIRECTION ( 'NONE',  ( -0.000000000000000000, -1.000000000000000000, -0.000000000000000000 ) ) ;
#20889 = AXIS2_PLACEMENT_3D ( 'NONE', #22050, #17766, #13035 ) ;
#20890 = CIRCLE ( 'NONE', #12664, 11.57481594606304576 ) ;
#20891 = FACE_OUTER_BOUND ( 'NONE', #12769, .T. ) ;
#20892 = PLANE ( 'NONE',  #27647 ) ;
#20893 = CARTESIAN_POINT ( 'NONE',  ( 13.14518615778179900, 39.61093750108393863, -5.444914386472297529 ) ) ;
#20894 = CARTESIAN_POINT ( 'NONE',  ( 0.000000000000000000, 30.99999999999999645, 0.000000000000000000 ) ) ;
#20895 = AXIS2_PLACEMENT_3D ( 'NONE', #654, #9327, #13591 ) ;
#20896 = DIRECTION ( 'NONE',  ( 0.000000000000000000, 1.000000000000000000, 0.000000000000000000 ) ) ;
#20897 = DIRECTION ( 'NONE',  ( 0.000000000000000000, 0.000000000000000000, -1.000000000000000000 ) ) ;
#20898 = CARTESIAN_POINT ( 'NONE',  ( 135.6228728715778686, 35.19570312499999432, -13.57481594606304753 ) ) ;
#20899 = ORIENTED_EDGE ( 'NONE', *, *, #3086, .F. ) ;
#20900 = ORIENTED_EDGE ( 'NONE', *, *, #26414, .F. ) ;
#20901 = LINE ( 'NONE', #7642, #867 ) ;
#20902 = PRODUCT_DEFINITION_CONTEXT ( 'detailed design', #3147, 'design' ) ;
#20903 = CARTESIAN_POINT ( 'NONE',  ( 5.622872871577871301, 40.75195312500000711, -13.57481594606304753 ) ) ;
#20904 = CARTESIAN_POINT ( 'NONE',  ( -13.57481594606304753, 31.52460937716787370, -5.622872871577873077 ) ) ;
#20905 = CARTESIAN_POINT ( 'NONE',  ( 99.99999999999995737, -4.999999999999990230, 4.375000002731185056 ) ) ;
#20906 = CARTESIAN_POINT ( 'NONE',  ( 124.5550856135277087, 39.01562500108394005, -13.14518615778179900 ) ) ;
#20907 = CARTESIAN_POINT ( 'NONE',  ( 78.14518615778179367, 36.93203125108394147, 5.444914386472293977 ) ) ;
#20908 = DIRECTION ( 'NONE',  ( -0.000000000000000000, 1.000000000000000000, -0.000000000000000000 ) ) ;
#20909 = CARTESIAN_POINT ( 'NONE',  ( -13.14518615778179900, 38.12265625108393152, -5.444914386472297529 ) ) ;
#20910 = DIRECTION ( 'NONE',  ( 0.8660254037844392627, 0.000000000000000000, -0.4999999999999987788 ) ) ;
#20911 = CARTESIAN_POINT ( 'NONE',  ( 51.42518405393695957, 37.82499999999999574, 0.000000000000000000 ) ) ;
#20912 = CARTESIAN_POINT ( 'NONE',  ( 93.00000000000000000, 110.0000000000000000, -52.50000000546237544 ) ) ;
#20913 = LINE ( 'NONE', #18768, #4803 ) ;
#20914 = CARTESIAN_POINT ( 'NONE',  ( 181.8548138422181921, 31.77265625108393365, -5.444914386472297529 ) ) ;
#20915 = CARTESIAN_POINT ( 'NONE',  ( 142.5314254911195349, 35.99999999999996447, -5.200562670744178995 ) ) ;
#20916 = CARTESIAN_POINT ( 'NONE',  ( 101.0355339059327378, 124.4500000000000028, 2.499999999999977796 ) ) ;
#20917 =( GEOMETRIC_REPRESENTATION_CONTEXT ( 3 ) GLOBAL_UNCERTAINTY_ASSIGNED_CONTEXT ( ( #17245 ) ) GLOBAL_UNIT_ASSIGNED_CONTEXT ( ( #16604, #1237, #18748 ) ) REPRESENTATION_CONTEXT ( 'NONE', 'WORKASPACE' ) );
#20918 = CARTESIAN_POINT ( 'NONE',  ( 99.99999999999998579, 124.1500000010924651, 2.066987299999980099 ) ) ;
#20919 = CARTESIAN_POINT ( 'NONE',  ( 116.8258427830772348, 35.99999999999998579, 0.03826467346029212291 ) ) ;
#20920 = CARTESIAN_POINT ( 'NONE',  ( 181.4251840539369596, 39.51171875216787299, 0.000000000000000000 ) ) ;
#20921 = CARTESIAN_POINT ( 'NONE',  ( 103.1528011352953342, -3.152801135295355106, 11.81250000136559208 ) ) ;
#20922 = CARTESIAN_POINT ( 'NONE',  ( 2.493653234604083739E-15, 32.56640625216787299, 13.57481594606304576 ) ) ;
#20923 = ORIENTED_EDGE ( 'NONE', *, *, #24846, .T. ) ;
#20924 = CARTESIAN_POINT ( 'NONE',  ( 9.598844408820456309, 40.70234374999999716, -9.598844408820458085 ) ) ;
#20925 = CARTESIAN_POINT ( 'NONE',  ( -5.622872871577873077, 39.26367187499999289, -13.57481594606304753 ) ) ;
#20926 = CARTESIAN_POINT ( 'NONE',  ( 6.944423797152706079, 31.55306878032414986, -11.16113333171310451 ) ) ;
#20927 = CARTESIAN_POINT ( 'NONE',  ( 9.598844408820459861, 31.87187500216787228, 9.598844408820456309 ) ) ;
#20928 = CARTESIAN_POINT ( 'NONE',  ( 96.84719886470459471, 81.31250000136559208, -3.152801135295383084 ) ) ;
#20929 = CARTESIAN_POINT ( 'NONE',  ( 65.00000000000000000, 37.77539062608393294, 13.14518615778179544 ) ) ;
#20930 = CARTESIAN_POINT ( 'NONE',  ( 91.91746824999998466, 112.6261737610028320, -49.47500000273119269 ) ) ;
#20931 = CYLINDRICAL_SURFACE ( 'NONE', #24144, 2.499999999999995115 ) ;
#20932 = CARTESIAN_POINT ( 'NONE',  ( 101.4615807364564546, 123.4500000010924765, 1.461580736456455476 ) ) ;
#20933 = CARTESIAN_POINT ( 'NONE',  ( 51.42518405393695957, 38.76757812716787299, 5.622872871577880183 ) ) ;
#20934 = CARTESIAN_POINT ( 'NONE',  ( 104.3262379212492448, 104.0454443415356991, -49.79999999453762882 ) ) ;
#20935 = CARTESIAN_POINT ( 'NONE',  ( 116.8548138422182205, 33.60820312608393579, 0.000000000000000000 ) ) ;
#20936 = EDGE_LOOP ( 'NONE', ( #25601, #1562, #14234, #4104 ) ) ;
#20937 = CARTESIAN_POINT ( 'NONE',  ( 139.5988444088204687, 37.42812500216787441, 9.598844408820456309 ) ) ;
#20938 = EDGE_CURVE ( 'NONE', #6173, #25694, #27841, .T. ) ;
#20939 =( BOUNDED_CURVE ( )  B_SPLINE_CURVE ( 2, ( #20432, #2763, #20003, #13706, #4902, #26562, #2895, #15989, #18431, #767, #9301, #18141, #22572, #20145, #13988, #23235, #26854, #17998, #3712, #11708, #483, #15851, #24845, #13564, #7014, #11564, #17857, #22713, #15710, #7302, #7590, #3183, #18289, #9728, #11853, #20281, #3038, #626, #20575, #9165, #24703, #27139, #24560, #1056, #5849, #5042, #16283, #22287, #24412, #9441, #11426, #24984, #26706, #5183, #14520, #7155, #26995, #22424, #13846, #915, #9585, #7441, #16137, #21511, #4263, #21798, #19365, #4407, #15649, #28068, #21655, #2557, #12793, #15068, #17646, #6954, #26205, #11218, #10936, #8675, #16769, #22080, #17795, #17366, #24069, #2131, #17504, #4545, #12923, #21941, #24348, #13207, #26062, #19647, #10658, #2419, #1991, #23787, #129, #24212, #6531 ),
 .UNSPECIFIED., .F., .F. ) 
 B_SPLINE_CURVE_WITH_KNOTS ( ( 3, 2, 2, 2, 2, 2, 2, 2, 2, 2, 2, 2, 2, 2, 2, 2, 2, 2, 2, 2, 2, 2, 2, 2, 2, 2, 2, 2, 2, 2, 2, 2, 2, 2, 2, 2, 2, 2, 2, 2, 2, 2, 2, 2, 2, 2, 2, 2, 2, 2, 3 ),
 ( 0.000000000000000000, 0.02000000000000000042, 0.04000000000000000083, 0.05999999999999999778, 0.08000000000000000167, 0.1000000000000000056, 0.1199999999999999956, 0.1400000000000000133, 0.1600000000000000033, 0.1799999999999999933, 0.2000000000000000111, 0.2200000000000000011, 0.2399999999999999911, 0.2600000000000000089, 0.2800000000000000266, 0.2999999999999999889, 0.3200000000000000067, 0.3400000000000000244, 0.3599999999999999867, 0.3800000000000000044, 0.4000000000000000222, 0.4199999999999999845, 0.4400000000000000022, 0.4600000000000000200, 0.4799999999999999822, 0.5000000000000000000, 0.5200000000000000178, 0.5400000000000000355, 0.5600000000000000533, 0.5799999999999999600, 0.5999999999999999778, 0.6199999999999999956, 0.6400000000000000133, 0.6600000000000000311, 0.6800000000000000488, 0.6999999999999999556, 0.7199999999999999734, 0.7399999999999999911, 0.7600000000000000089, 0.7800000000000000266, 0.8000000000000000444, 0.8199999999999999512, 0.8399999999999999689, 0.8599999999999999867, 0.8800000000000000044, 0.9000000000000000222, 0.9200000000000000400, 0.9399999999999999467, 0.9599999999999999645, 0.9799999999999999822, 1.000000000000000000 ),
 .UNSPECIFIED. ) 
 CURVE ( )  GEOMETRIC_REPRESENTATION_ITEM ( )  RATIONAL_B_SPLINE_CURVE ( ( 1.000000000000000000, 0.9510565162951535312, 1.000000000000000000, 0.9510565162951535312, 1.000000000000000000, 0.9510565162951535312, 1.000000000000000000, 0.9510565162951535312, 1.000000000000000000, 0.9510565162951535312, 1.000000000000000000, 0.9510565162951535312, 1.000000000000000000, 0.9510565162951535312, 1.000000000000000000, 0.9510565162951535312, 1.000000000000000000, 0.9510565162951535312, 1.000000000000000000, 0.9510565162951535312, 1.000000000000000000, 0.9510565162951535312, 1.000000000000000000, 0.9510565162951535312, 1.000000000000000000, 0.9510565162951535312, 1.000000000000000000, 0.9510565162951535312, 1.000000000000000000, 0.9510565162951535312, 1.000000000000000000, 0.9510565162951535312, 1.000000000000000000, 0.9510565162951535312, 1.000000000000000000, 0.9510565162951535312, 1.000000000000000000, 0.9510565162951535312, 1.000000000000000000, 0.9510565162951535312, 1.000000000000000000, 0.9510565162951535312, 1.000000000000000000, 0.9510565162951535312, 1.000000000000000000, 0.9510565162951535312, 1.000000000000000000, 0.9510565162951535312, 1.000000000000000000, 0.9510565162951535312, 1.000000000000000000, 0.9510565162951535312, 1.000000000000000000, 0.9510565162951535312, 1.000000000000000000, 0.9510565162951535312, 1.000000000000000000, 0.9510565162951535312, 1.000000000000000000, 0.9510565162951535312, 1.000000000000000000, 0.9510565162951535312, 1.000000000000000000, 0.9510565162951535312, 1.000000000000000000, 0.9510565162951535312, 1.000000000000000000, 0.9510565162951535312, 1.000000000000000000, 0.9510565162951535312, 1.000000000000000000, 0.9510565162951535312, 1.000000000000000000, 0.9510565162951535312, 1.000000000000000000, 0.9510565162951535312, 1.000000000000000000, 0.9510565162951535312, 1.000000000000000000, 0.9510565162951535312, 1.000000000000000000, 0.9510565162951535312, 1.000000000000000000, 0.9510565162951535312, 1.000000000000000000, 0.9510565162951535312, 1.000000000000000000, 0.9510565162951535312, 1.000000000000000000, 0.9510565162951535312, 1.000000000000000000, 0.9510565162951535312, 1.000000000000000000, 0.9510565162951535312, 1.000000000000000000, 0.9510565162951535312, 1.000000000000000000, 0.9510565162951535312, 1.000000000000000000, 0.9510565162951535312, 1.000000000000000000 ) ) 
 REPRESENTATION_ITEM ( '' )  );
#20940 = CARTESIAN_POINT ( 'NONE',  ( -9.295050272127046043, 39.85898437608393152, -9.295050272127046043 ) ) ;
#20941 = CARTESIAN_POINT ( 'NONE',  ( -5.622872871577873077, 39.36289062716787157, -13.57481594606304753 ) ) ;
#20942 = CARTESIAN_POINT ( 'NONE',  ( 97.92893218813452449, 94.68749999999998579, 4.999999999999983125 ) ) ;
#20943 = CARTESIAN_POINT ( 'NONE',  ( 78.57481594606304043, 39.95820312716787726, -5.622872871577873077 ) ) ;
#20944 = CARTESIAN_POINT ( 'NONE',  ( 108.0825317499999869, 112.6261737610028320, -52.52499999726881441 ) ) ;
#20945 = CARTESIAN_POINT ( 'NONE',  ( 5.622872871577871301, 38.46992187716787015, -13.57481594606304753 ) ) ;
#20946 = ORIENTED_EDGE ( 'NONE', *, *, #13074, .T. ) ;
#20947 = VECTOR ( 'NONE', #6258, 1000.000000000000000 ) ;
#20948 = CARTESIAN_POINT ( 'NONE',  ( 102.0710678118654329, 5.000000000000018652, 7.687499999999999112 ) ) ;
#20949 = EDGE_LOOP ( 'NONE', ( #22150, #12209, #19479, #14014 ) ) ;
#20950 = CARTESIAN_POINT ( 'NONE',  ( 9.295050272127046043, 34.10429687608393579, -9.295050272127046043 ) ) ;
#20951 = CARTESIAN_POINT ( 'NONE',  ( 200.4449143864723055, 40.00781250108393294, 13.14518615778179189 ) ) ;
#20952 = CARTESIAN_POINT ( 'NONE',  ( 94.99999999999995737, 1.387778780781445676E-14, 14.12500000273118594 ) ) ;
#20953 = CARTESIAN_POINT ( 'NONE',  ( 94.99999999999995737, 1.387778780781445676E-14, 1.125000002731184390 ) ) ;
#20954 = CARTESIAN_POINT ( 'NONE',  ( 116.8548138422182205, 37.42812500108393436, 5.444914386472304635 ) ) ;
#20955 = CARTESIAN_POINT ( 'NONE',  ( 94.99999999999995737, 80.12500000273119838, -1.387778780781445676E-14 ) ) ;
#20956 = DIRECTION ( 'NONE',  ( 1.000000000000000000, -0.000000000000000000, -7.228014483236696740E-18 ) ) ;
#20957 = CARTESIAN_POINT ( 'NONE',  ( 98.15313185440923860, 93.62499999863439371, -4.458734124999994997 ) ) ;
#20958 = CARTESIAN_POINT ( 'NONE',  ( 101.0355339059327378, 124.4500000000000028, 2.499999999999977796 ) ) ;
#20959 = CARTESIAN_POINT ( 'NONE',  ( 200.6228728715778686, 39.16445312499999432, -13.57481594606304753 ) ) ;
#20960 = APPLICATION_PROTOCOL_DEFINITION ( 'draft international standard', 'automotive_design', 1998, #22453 ) ;
#20961 = FACE_OUTER_BOUND ( 'NONE', #3484, .T. ) ;
#20962 = CARTESIAN_POINT ( 'NONE',  ( 101.8468681455906903, 4.458734125000016313, 1.375000001365592972 ) ) ;
#20963 = CARTESIAN_POINT ( 'NONE',  ( 98.96446609406724804, 123.2499999999999716, -2.499999999999993339 ) ) ;
#20964 = AXIS2_PLACEMENT_3D ( 'NONE', #23482, #19617, #5959 ) ;
#20965 = CARTESIAN_POINT ( 'NONE',  ( 103.1528011352953342, 3.152801135295383084, 5.062500001365592972 ) ) ;
#20966 = CARTESIAN_POINT ( 'NONE',  ( 95.67376207875072680, 104.0454443415356991, -46.20000000546237118 ) ) ;
#20967 = CARTESIAN_POINT ( 'NONE',  ( 95.54126587499999346, 93.99999999863439371, -1.846868145590737864 ) ) ;
#20968 = DIRECTION ( 'NONE',  ( 0.000000000000000000, 1.000000000000000000, 0.000000000000000000 ) ) ;
#20969 = CARTESIAN_POINT ( 'NONE',  ( 102.4999999999999858, 122.3000000021849587, -9.847140817659276890E-15 ) ) ;
#20970 = CARTESIAN_POINT ( 'NONE',  ( -5.622872871577873077, 40.35507812499998437, 13.57481594606304753 ) ) ;
#20971 = VERTEX_POINT ( 'NONE', #4174 ) ;
#20972 = CARTESIAN_POINT ( 'NONE',  ( 101.8468681455906903, 83.37500000136563472, -4.458734125000016313 ) ) ;
#20973 = VECTOR ( 'NONE', #17465, 1000.000000000000000 ) ;
#20974 =( BOUNDED_CURVE ( )  B_SPLINE_CURVE ( 2, ( #9888, #5350, #13730, #9610, #16311, #24584, #20456, #18313, #24728 ),
 .UNSPECIFIED., .F., .F. ) 
 B_SPLINE_CURVE_WITH_KNOTS ( ( 3, 2, 2, 2, 3 ),
 ( 0.3571428571428572063, 0.3660714285714286031, 0.3750000000000000000, 0.3839285714285714524, 0.3928571428571428492 ),
 .UNSPECIFIED. ) 
 CURVE ( )  GEOMETRIC_REPRESENTATION_ITEM ( )  RATIONAL_B_SPLINE_CURVE ( ( 0.9999999999999995559, 0.9238795325112871826, 1.000000000000000000, 0.9238795325112867385, 1.000000000000000000, 0.9238795325112867385, 1.000000000000000000, 0.9238795325112867385, 1.000000000000000000 ) ) 
 REPRESENTATION_ITEM ( '' )  );
#20975 = CARTESIAN_POINT ( 'NONE',  ( -13.57481594606304398, 31.62382812716787228, 5.622872871577880183 ) ) ;
#20976 = VERTEX_POINT ( 'NONE', #15801 ) ;
#20977 = EDGE_CURVE ( 'NONE', #15512, #21487, #8005, .T. ) ;
#20978 = EDGE_LOOP ( 'NONE', ( #13553, #6354, #23575, #565 ) ) ;
#20979 = CARTESIAN_POINT ( 'NONE',  ( 201.1610621748488370, 51.27996893917539012, -15.00000000000137845 ) ) ;
#20980 = CARTESIAN_POINT ( 'NONE',  ( 101.8468681455906903, -4.458734124999987891, 7.000000001365592972 ) ) ;
#20981 = VERTEX_POINT ( 'NONE', #12836 ) ;
#20982 = CARTESIAN_POINT ( 'NONE',  ( 108.0825317500000011, 107.3738262389971538, -44.47500000273118559 ) ) ;
#20983 = CARTESIAN_POINT ( 'NONE',  ( 9.295050272127046043, 34.69960937608393436, -9.295050272127046043 ) ) ;
#20984 = CYLINDRICAL_SURFACE ( 'NONE', #12215, 4.999999999999989342 ) ;
#20985 = CARTESIAN_POINT ( 'NONE',  ( -8.049105076161786076E-16, 38.76757812608393294, -13.14518615778179544 ) ) ;
#20986 = CARTESIAN_POINT ( 'NONE',  ( 95.00472066334981491, 103.1245878333314465, -48.82500000273119412 ) ) ;
#20987 = CARTESIAN_POINT ( 'NONE',  ( 135.4449143864723339, 40.20625000108394431, 13.14518615778179189 ) ) ;
#20988 = CARTESIAN_POINT ( 'NONE',  ( 6.944426393311538881, 31.55306875057403104, -11.16113171639042356 ) ) ;
#20989 = AXIS2_PLACEMENT_3D ( 'NONE', #11595, #9754, #6909 ) ;
#20990 = CARTESIAN_POINT ( 'NONE',  ( 78.57481594606304043, 37.37851562499999858, 5.622872871577869525 ) ) ;
#20991 = DIRECTION ( 'NONE',  ( 0.000000000000000000, 0.000000000000000000, 1.000000000000000000 ) ) ;
#20992 = CARTESIAN_POINT ( 'NONE',  ( 107.0000000000000000, 110.0000000000000000, -50.00000000000000711 ) ) ;
#20993 = EDGE_CURVE ( 'NONE', #22034, #26723, #27145, .T. ) ;
#20994 = CARTESIAN_POINT ( 'NONE',  ( -8.049105076161786076E-16, 32.61601562608393579, -13.14518615778179544 ) ) ;
#20995 = CARTESIAN_POINT ( 'NONE',  ( 99.99999999999995737, 4.458734125000016313, 1.437500001365592972 ) ) ;
#20996 = CARTESIAN_POINT ( 'NONE',  ( 104.4587341249999781, 83.25000000136559208, -1.846868145590750521 ) ) ;
#20997 = CARTESIAN_POINT ( 'NONE',  ( 5.444914386472302859, 36.03906250108394005, 13.14518615778179189 ) ) ;
#20998 = CARTESIAN_POINT ( 'NONE',  ( 99.99999999999998579, 128.0000000000000000, -5.204170427930421283E-15 ) ) ;
#20999 = AXIS2_PLACEMENT_3D ( 'NONE', #20502, #9794, #16061 ) ;
#21000 = LINE ( 'NONE', #8014, #4229 ) ;
#21001 = ORIENTED_EDGE ( 'NONE', *, *, #1090, .F. ) ;
#21002 = DIRECTION ( 'NONE',  ( 1.000000000000000000, 1.734723475976808080E-15, -7.228014483236698281E-18 ) ) ;
#21004 = EDGE_CURVE ( 'NONE', #19618, #21949, #18559, .T. ) ;
#21003 = CARTESIAN_POINT ( 'NONE',  ( 102.1631189606246295, 103.3426043859339103, -53.89999999453763735 ) ) ;
#21005 = CARTESIAN_POINT ( 'NONE',  ( 101.8468681455907330, 92.74999999863439371, -4.458734124999994997 ) ) ;
#21006 = FACE_OUTER_BOUND ( 'NONE', #20177, .T. ) ;
#21007 = CARTESIAN_POINT ( 'NONE',  ( -20.00000000000000000, 50.00000000000000000, 10.00000000000000178 ) ) ;
#21008 = CARTESIAN_POINT ( 'NONE',  ( 104.9999999999999716, -2.071067811865462627, 6.562500002731185944 ) ) ;
#21009 = VERTEX_POINT ( 'NONE', #18377 ) ;
#21010 = CARTESIAN_POINT ( 'NONE',  ( 51.85481384221821344, 38.42031250108393436, 5.444914386472304635 ) ) ;
#21011 = ADVANCED_FACE ( 'NONE', ( #12077 ), #27365, .T. ) ;
#21012 = CARTESIAN_POINT ( 'NONE',  ( 0.000000000000000000, 52.00000000000000711, 0.000000000000000000 ) ) ;
#21013 = CARTESIAN_POINT ( 'NONE',  ( 195.0000000000000000, 32.21914062608393436, 13.14518615778179544 ) ) ;
#21014 =( BOUNDED_CURVE ( )  B_SPLINE_CURVE ( 2, ( #15284, #15427, #8463, #6742, #11143 ),
 .UNSPECIFIED., .F., .F. ) 
 B_SPLINE_CURVE_WITH_KNOTS ( ( 3, 2, 3 ),
 ( 0.9500000000000009548, 0.9750000000000005329, 1.000000000000000000 ),
 .UNSPECIFIED. ) 
 CURVE ( )  GEOMETRIC_REPRESENTATION_ITEM ( )  RATIONAL_B_SPLINE_CURVE ( ( 0.9999999999999970024, 0.9238795325112897361, 1.000000000000000000, 0.9238795325112867385, 1.000000000000000000 ) ) 
 REPRESENTATION_ITEM ( '' )  );
#21015 = VERTEX_POINT ( 'NONE', #863 ) ;
#21016 = DIRECTION ( 'NONE',  ( 0.000000000000000000, 1.000000000000000000, 0.000000000000000000 ) ) ;
#21017 = CARTESIAN_POINT ( 'NONE',  ( -3.636496246811128596, 51.46815297079189122, -15.00000000000000178 ) ) ;
#21018 = CARTESIAN_POINT ( 'NONE',  ( -9.598844408820458085, 33.75703124999999005, -9.598844408820458085 ) ) ;
#21019 = ADVANCED_FACE ( 'NONE', ( #5696 ), #285, .T. ) ;
#21020 = CARTESIAN_POINT ( 'NONE',  ( 139.5988444088204687, 35.84062500216786873, 9.598844408820456309 ) ) ;
#21021 = CYLINDRICAL_SURFACE ( 'NONE', #27896, 13.57481594606304398 ) ;
#21022 = CARTESIAN_POINT ( 'NONE',  ( 7.114649318941503431, 31.93754143773660203, -11.43472154218138570 ) ) ;
#21023 = PRODUCT_DEFINITION_SHAPE ( 'NONE', 'NONE',  #28216 ) ;
#21024 = CARTESIAN_POINT ( 'NONE',  ( 195.0000000000000000, 36.58476562608393579, -13.14518615778179544 ) ) ;
#21025 = VERTEX_POINT ( 'NONE', #11655 ) ;
#21026 = CARTESIAN_POINT ( 'NONE',  ( 99.99999999999995737, 4.458734125000016313, 13.43750000136559386 ) ) ;
#21027 = CARTESIAN_POINT ( 'NONE',  ( 104.9999999999999716, 90.93749999999998579, 2.071067811865467956 ) ) ;
#21028 = CARTESIAN_POINT ( 'NONE',  ( 104.4587341249999781, 83.00000000136562051, -1.846868145590750521 ) ) ;
#21029 = CARTESIAN_POINT ( 'NONE',  ( 99.99999999999998579, 89.99899999999999523, -9.540979117872439019E-15 ) ) ;
#21030 = FACE_OUTER_BOUND ( 'NONE', #11588, .T. ) ;
#21031 = CARTESIAN_POINT ( 'NONE',  ( 84.99999999999998579, 120.0000000000000000, -15.00000000000000533 ) ) ;
#21032 = CARTESIAN_POINT ( 'NONE',  ( -8.312177448680279460E-16, 32.86406249999999574, -13.57481594606304576 ) ) ;
#21033 = CARTESIAN_POINT ( 'NONE',  ( 195.0000000000000000, -7.395377635281828788, -2.255140518769849538E-14 ) ) ;
#21034 = CARTESIAN_POINT ( 'NONE',  ( 97.50236033167490746, 117.6869444889999841, -48.02499999726882152 ) ) ;
#21035 = ORIENTED_EDGE ( 'NONE', *, *, #25847, .F. ) ;
#21036 = VERTEX_POINT ( 'NONE', #24930 ) ;
#21037 = CARTESIAN_POINT ( 'NONE',  ( -13.57481594606304398, 37.18007812716787441, 5.622872871577880183 ) ) ;
#21038 = CARTESIAN_POINT ( 'NONE',  ( -5.622872871577873077, 38.46992187499999716, -13.57481594606304753 ) ) ;
#21039 = CARTESIAN_POINT ( 'NONE',  ( 9.295050272127047819, 40.05742187608392868, 9.295050272127046043 ) ) ;
#21040 = CARTESIAN_POINT ( 'NONE',  ( 94.99999999999995737, 1.387778780781445676E-14, 6.125000002731185056 ) ) ;
#21041 = CARTESIAN_POINT ( 'NONE',  ( 143.1451861577818079, 38.76757812608393294, -1.609821015232357215E-15 ) ) ;
#21042 = CARTESIAN_POINT ( 'NONE',  ( 78.14518615778179367, 35.44375000108393436, -5.444914386472297529 ) ) ;
#21043 = EDGE_CURVE ( 'NONE', #15854, #15131, #22662, .T. ) ;
#21044 = DIRECTION ( 'NONE',  ( 0.000000000000000000, -1.000000000000000000, 0.000000000000000000 ) ) ;
#21045 = CARTESIAN_POINT ( 'NONE',  ( -9.295050272127044266, 35.09648437608392868, 9.295050272127047819 ) ) ;
#21046 =( BOUNDED_CURVE ( )  B_SPLINE_CURVE ( 2, ( #9082, #8795, #6515, #15631, #26335, #19491, #15053, #25909, #24195 ),
 .UNSPECIFIED., .F., .T. ) 
 B_SPLINE_CURVE_WITH_KNOTS ( ( 3, 2, 2, 2, 3 ),
 ( 0.2500000000000002220, 0.2750000000000002442, 0.3000000000000002665, 0.3250000000000002887, 0.3500000000000003109 ),
 .UNSPECIFIED. ) 
 CURVE ( )  GEOMETRIC_REPRESENTATION_ITEM ( )  RATIONAL_B_SPLINE_CURVE ( ( 0.9999999999999993339, 0.9238795325112874046, 1.000000000000000000, 0.9238795325112867385, 1.000000000000000000, 0.9238795325112867385, 1.000000000000000000, 0.9238795325112857393, 1.000000000000001110 ) ) 
 REPRESENTATION_ITEM ( '' )  );
#21047 = CARTESIAN_POINT ( 'NONE',  ( 196.4643377203195200, 35.99999999999997868, -13.46163418879037188 ) ) ;
#21048 = CARTESIAN_POINT ( 'NONE',  ( 97.50000000000000000, 123.5500000021849587, 1.035533905932725096 ) ) ;
#21049 = CARTESIAN_POINT ( 'NONE',  ( 195.0000000000000000, 39.21406249999999716, -13.57481594606304576 ) ) ;
#21050 = LINE ( 'NONE', #25879, #7621 ) ;
#21051 = CARTESIAN_POINT ( 'NONE',  ( 195.0000000000000000, 40.80156249999999574, -13.57481594606304576 ) ) ;
#21052 = CARTESIAN_POINT ( 'NONE',  ( -8.049105076161786076E-16, 37.18007812608393436, -13.14518615778179544 ) ) ;
#21053 = CARTESIAN_POINT ( 'NONE',  ( 131.1371678245417627, 36.00000000000000000, 13.09590655363595602 ) ) ;
#21054 = CARTESIAN_POINT ( 'NONE',  ( 102.4999999999999716, 123.7569999999781771, 1.035533905932722876 ) ) ;
#21055 = CARTESIAN_POINT ( 'NONE',  ( 98.53841926354351699, 124.6500000010924651, -1.461580736456474794 ) ) ;
#21056 = DIRECTION ( 'NONE',  ( -0.000000000000000000, -1.000000000000000000, -0.000000000000000000 ) ) ;
#21057 = FACE_OUTER_BOUND ( 'NONE', #17062, .T. ) ;
#21058 = CARTESIAN_POINT ( 'NONE',  ( 2.493653234604083739E-15, 32.46718749999999432, 13.57481594606304576 ) ) ;
#21059 = CARTESIAN_POINT ( 'NONE',  ( 116.4251840539369596, 40.95039062499999005, -5.622872871577872189 ) ) ;
#21060 = CARTESIAN_POINT ( 'NONE',  ( 13.57481594606304931, 40.55351562499998863, 5.622872871577869525 ) ) ;
#21061 = CARTESIAN_POINT ( 'NONE',  ( 2.414731522848535132E-15, 32.81445312608393294, 13.14518615778179544 ) ) ;
#21062 = VECTOR ( 'NONE', #8808, 1000.000000000000000 ) ;
#21063 = CARTESIAN_POINT ( 'NONE',  ( 2.493653234604083739E-15, 32.56640625216787299, 13.57481594606304576 ) ) ;
#21064 = CARTESIAN_POINT ( 'NONE',  ( 0.000000000000000000, 40.99999999999999289, 0.000000000000000000 ) ) ;
#21065 = CARTESIAN_POINT ( 'NONE',  ( 103.1528011352953342, 80.81250000136559208, 3.152801135295355106 ) ) ;
#21066 = CARTESIAN_POINT ( 'NONE',  ( 51.85481384221820633, 37.57695312608393579, 0.000000000000000000 ) ) ;
#21067 = CARTESIAN_POINT ( 'NONE',  ( 95.00472066334982912, 103.1245878333314323, -47.07500000273119412 ) ) ;
#21068 = CARTESIAN_POINT ( 'NONE',  ( 13.57481594606304753, 35.19570312716787441, -5.622872871577873966 ) ) ;
#21069 = CYLINDRICAL_SURFACE ( 'NONE', #26220, 11.57481594606304576 ) ;
#21070 = CARTESIAN_POINT ( 'NONE',  ( 99.99999999999998579, 110.0000000000000000, -145.0000000000000284 ) ) ;
#21071 = CARTESIAN_POINT ( 'NONE',  ( 104.3262379212492448, 115.9545556584642867, -49.19999999453763451 ) ) ;
#21072 = CARTESIAN_POINT ( 'NONE',  ( 130.0000000000000000, 32.61601562608393579, -13.14518615778179544 ) ) ;
#21073 = ORIENTED_EDGE ( 'NONE', *, *, #20642, .F. ) ;
#21074 = CARTESIAN_POINT ( 'NONE',  ( 0.8421075954646569661, 53.50112910130383881, -15.00000000000000178 ) ) ;
#21075 = CARTESIAN_POINT ( 'NONE',  ( -8.049105076161786076E-16, 39.75976562608394005, -13.14518615778179544 ) ) ;
#21076 = CARTESIAN_POINT ( 'NONE',  ( 103.1528011352953342, 79.81250000136559208, 3.152801135295355106 ) ) ;
#21077 = CARTESIAN_POINT ( 'NONE',  ( 124.5550856135277087, 39.61093750108393152, -13.14518615778179900 ) ) ;
#21078 = CARTESIAN_POINT ( 'NONE',  ( 78.57481594606305464, 35.93984375216787441, -1.662435489736055892E-15 ) ) ;
#21079 = CARTESIAN_POINT ( 'NONE',  ( 91.91746824999998466, 110.0000000000000000, -55.62499999726882294 ) ) ;
#21080 = CARTESIAN_POINT ( 'NONE',  ( -5.622872871577873077, 34.60039062716786873, -13.57481594606304753 ) ) ;
#21081 = VERTEX_POINT ( 'NONE', #20801 ) ;
#21082 = AXIS2_PLACEMENT_3D ( 'NONE', #4806, #2391, #20052 ) ;
#21083 = CARTESIAN_POINT ( 'NONE',  ( 97.92893218813451028, 5.000000000000018652, 9.812499999999998224 ) ) ;
#21084 = CARTESIAN_POINT ( 'NONE',  ( 107.0000000000000142, 112.2744378736303332, -52.90000000000001279 ) ) ;
#21085 = CARTESIAN_POINT ( 'NONE',  ( 9.295050272127046043, 32.51679687608393721, -9.295050272127046043 ) ) ;
#21086 = CARTESIAN_POINT ( 'NONE',  ( 181.8548138422181921, 36.63437500108393152, 5.444914386472304635 ) ) ;
#21087 = CARTESIAN_POINT ( 'NONE',  ( 13.57481594606304753, 36.78320312716788010, -5.622872871577873966 ) ) ;
#21088 = CARTESIAN_POINT ( 'NONE',  ( 130.0000000000000000, 37.57695312608392868, 13.14518615778179544 ) ) ;
#21089 = CARTESIAN_POINT ( 'NONE',  ( 5.444914386472302859, 32.26875000108393721, 13.14518615778179189 ) ) ;
#21090 = EDGE_CURVE ( 'NONE', #10399, #21990, #16080, .T. ) ;
#21091 = CARTESIAN_POINT ( 'NONE',  ( 104.4587341249999923, 95.24999999863437949, 1.846868145590726318 ) ) ;
#21092 = CARTESIAN_POINT ( 'NONE',  ( 59.37712712842218821, 37.18007812499999432, 13.57481594606311504 ) ) ;
#21093 = CARTESIAN_POINT ( 'NONE',  ( 102.4999999999999858, 124.6000000000000085, -9.847140817659276890E-15 ) ) ;
#21094 = CARTESIAN_POINT ( 'NONE',  ( 195.0000000000000000, 38.42031249999999432, -13.57481594606304576 ) ) ;
#21095 = PRODUCT_CONTEXT ( 'NONE', #18624, 'mechanical' ) ;
#21096 = LINE ( 'NONE', #16675, #20947 ) ;
#21097 = CARTESIAN_POINT ( 'NONE',  ( 96.84719886470459471, -3.152801135295355994, 1.812500001365591640 ) ) ;
#21098 = CARTESIAN_POINT ( 'NONE',  ( 74.29505027212704249, 40.05742187608392868, 9.295050272127046043 ) ) ;
#21099 = CARTESIAN_POINT ( 'NONE',  ( 95.54126587499996504, -1.846868145590724986, 4.500000001365592084 ) ) ;
#21100 = CARTESIAN_POINT ( 'NONE',  ( 97.83688103937537051, 103.3426043859339103, -46.10000000546238397 ) ) ;
#21101 = CARTESIAN_POINT ( 'NONE',  ( 103.1528011352953484, 93.43749999863440792, 3.152801135295352886 ) ) ;
#21102 = CARTESIAN_POINT ( 'NONE',  ( 103.5355339059327093, -3.535533905932726206, 9.375000000000000000 ) ) ;
#21103 = CARTESIAN_POINT ( 'NONE',  ( -9.713547494048821562, 36.00000000000000000, 8.898183052316806396 ) ) ;
#21104 = CARTESIAN_POINT ( 'NONE',  ( 5.622872871577871301, 38.37070312499999147, -13.57481594606304753 ) ) ;
#21105 = ORIENTED_EDGE ( 'NONE', *, *, #14634, .T. ) ;
#21106 = CARTESIAN_POINT ( 'NONE',  ( 99.99999999999995737, 84.43750000136560629, -4.458734125000016313 ) ) ;
#21107 = AXIS2_PLACEMENT_3D ( 'NONE', #26919, #2687, #5105 ) ;
#21108 = CARTESIAN_POINT ( 'NONE',  ( 101.8468681455907330, 90.49999999863442213, -4.458734124999994997 ) ) ;
#21109 = ORIENTED_EDGE ( 'NONE', *, *, #13826, .F. ) ;
#21110 = B_SPLINE_CURVE_WITH_KNOTS ( 'NONE', 3,
 ( #3583, #27528, #6264, #16945, #10107, #1864, #8395, #5995, #1591, #21103, #10664, #14937, #18954, #19372, #23659, #21518, #1997, #28076, #17226, #27662, #8124, #5726, #23109, #16820, #18821 ),
 .UNSPECIFIED., .F., .F.,
 ( 4, 2, 2, 2, 2, 2, 2, 1, 2, 2, 2, 2, 4 ),
 ( 0.000000000000000000, 0.001301161269048867718, 0.002602322538097735435, 0.005204645076195470003, 0.007806967614293204571, 0.01040929015239093480, 0.01171045142143979818, 0.01301161269048865983, 0.01431277395953752495, 0.01561393522858638833, 0.01821625776668411162, 0.01951741903573297673, 0.02081858030478183838 ),
 .UNSPECIFIED. ) ;
#21111 = ORIENTED_EDGE ( 'NONE', *, *, #21157, .T. ) ;
#21112 = CARTESIAN_POINT ( 'NONE',  ( -5.622872871577965448, 33.31054687716787299, 13.57481594606295161 ) ) ;
#21113 = CARTESIAN_POINT ( 'NONE',  ( 103.1528011352953342, 3.152801135295383084, 7.312500001365592084 ) ) ;
#21114 = ORIENTED_EDGE ( 'NONE', *, *, #11950, .T. ) ;
#21115 = CARTESIAN_POINT ( 'NONE',  ( 108.0825317500000153, 110.0000000000000000, -46.37500000273119838 ) ) ;
#21116 = CARTESIAN_POINT ( 'NONE',  ( 13.14518615778179900, 34.55078125108393294, 5.444914386472293977 ) ) ;
#21117 = CARTESIAN_POINT ( 'NONE',  ( 185.4011555911795597, 39.61093750216787868, 9.598844408820459861 ) ) ;
#21118 = CARTESIAN_POINT ( 'NONE',  ( 9.295050272127047819, 38.46992187608393010, 9.295050272127046043 ) ) ;
#21119 = CARTESIAN_POINT ( 'NONE',  ( 97.50236033167492167, 117.6869444889999841, -49.52500000273119696 ) ) ;
#21120 = CARTESIAN_POINT ( 'NONE',  ( 116.8548138422182205, 40.70234375108392300, -5.444914386472297529 ) ) ;
#21121 = CARTESIAN_POINT ( 'NONE',  ( -13.14518615778179189, 33.45937500108392726, 5.444914386472304635 ) ) ;
#21122 = EDGE_CURVE ( 'NONE', #14157, #22191, #4907, .T. ) ;
#21123 = ORIENTED_EDGE ( 'NONE', *, *, #18893, .F. ) ;
#21124 = CARTESIAN_POINT ( 'NONE',  ( 70.62287287157788285, 36.48554687499999716, 13.57481594606304576 ) ) ;
#21125 = CARTESIAN_POINT ( 'NONE',  ( 101.7677669529663547, 123.0999999999999943, -1.767766952966370209 ) ) ;
#21126 = CARTESIAN_POINT ( 'NONE',  ( 202.0656349887611327, 36.00000000000000000, 11.21307450592185795 ) ) ;
#21127 = CARTESIAN_POINT ( 'NONE',  ( 95.54126587499995082, -1.846868145590724986, 4.500000001365592084 ) ) ;
#21128 = CARTESIAN_POINT ( 'NONE',  ( -9.295050272127044266, 32.91367187608393152, 9.295050272127047819 ) ) ;
#21129 = CARTESIAN_POINT ( 'NONE',  ( 103.1528011352953342, -3.152801135295355106, 3.062500001365592528 ) ) ;
#21130 =( BOUNDED_CURVE ( )  B_SPLINE_CURVE ( 2, ( #524, #9205, #16741, #5644, #6059, #16877, #3780, #1373, #6194, #23308, #14864 ),
 .UNSPECIFIED., .F., .F. ) 
 B_SPLINE_CURVE_WITH_KNOTS ( ( 3, 2, 2, 2, 2, 3 ),
 ( 0.1000000000000000056, 0.1200000000000000233, 0.1400000000000000688, 0.1600000000000001144, 0.1800000000000001044, 0.2000000000000001776 ),
 .UNSPECIFIED. ) 
 CURVE ( )  GEOMETRIC_REPRESENTATION_ITEM ( )  RATIONAL_B_SPLINE_CURVE ( ( 1.000000000000000000, 0.9510565162951535312, 1.000000000000000000, 0.9510565162951535312, 1.000000000000000000, 0.9510565162951535312, 1.000000000000000000, 0.9510565162951535312, 1.000000000000000000, 0.9510565162951530871, 1.000000000000000444 ) ) 
 REPRESENTATION_ITEM ( '' )  );
#21131 = CARTESIAN_POINT ( 'NONE',  ( 96.84719886470459471, 83.56250000136560629, -3.152801135295383084 ) ) ;
#21132 = CARTESIAN_POINT ( 'NONE',  ( -13.14518615778179900, 33.36015625108393579, -5.444914386472297529 ) ) ;
#21133 = CARTESIAN_POINT ( 'NONE',  ( -9.295050272127046043, 39.06523437608392868, -9.295050272127046043 ) ) ;
#21134 = LINE ( 'NONE', #3752, #23801 ) ;
#21135 = ORIENTED_EDGE ( 'NONE', *, *, #25892, .T. ) ;
#21136 = CARTESIAN_POINT ( 'NONE',  ( 65.00000000000000000, 38.91640625216786731, 13.57481594606304576 ) ) ;
#21137 = FACE_OUTER_BOUND ( 'NONE', #19297, .T. ) ;
#21138 = CARTESIAN_POINT ( 'NONE',  ( 99.99999999999998579, 91.12499999726880162, -4.999999999999997335 ) ) ;
#21139 = CARTESIAN_POINT ( 'NONE',  ( 104.9952793366501709, 103.1245878333314323, -55.17499999726882720 ) ) ;
#21140 = CARTESIAN_POINT ( 'NONE',  ( 120.4011555911795455, 39.61093750216787868, 9.598844408820459861 ) ) ;
#21141 = VERTEX_POINT ( 'NONE', #18521 ) ;
#21142 = CARTESIAN_POINT ( 'NONE',  ( 70.44491438647229131, 38.61875000108392442, 13.14518615778179189 ) ) ;
#21143 = CARTESIAN_POINT ( 'NONE',  ( 2.493653234604083739E-15, 32.56640625216787299, 13.57481594606304576 ) ) ;
#21144 = CARTESIAN_POINT ( 'NONE',  ( 74.18017581364799184, 55.00000000000000000, -14.99999999999999822 ) ) ;
#21145 = EDGE_CURVE ( 'NONE', #12415, #11020, #25073, .T. ) ;
#21146 = EDGE_LOOP ( 'NONE', ( #186, #9420, #14095, #518 ) ) ;
#21147 = FACE_OUTER_BOUND ( 'NONE', #23315, .T. ) ;
#21148 = VECTOR ( 'NONE', #26979, 1000.000000000000000 ) ;
#21149 = CARTESIAN_POINT ( 'NONE',  ( -0.7238719380229414746, 53.51529642094998707, -14.99999999999999645 ) ) ;
#21150 = CARTESIAN_POINT ( 'NONE',  ( 194.1578924045353745, 53.50112910130381749, 14.99999999999995204 ) ) ;
#21151 = CARTESIAN_POINT ( 'NONE',  ( 143.5748159460630404, 34.30273437716787299, 5.622872871577869525 ) ) ;
#21152 = CARTESIAN_POINT ( 'NONE',  ( 103.5355339059327093, 81.50000000273119838, 3.535533905932726206 ) ) ;
#21153 = EDGE_CURVE ( 'NONE', #5951, #10805, #7645, .T. ) ;
#21154 = CARTESIAN_POINT ( 'NONE',  ( -15.00000000000000178, 80.00000000000000000, 1.734723475976807489E-15 ) ) ;
#21155 = CARTESIAN_POINT ( 'NONE',  ( 181.8548138422181921, 38.32109375108394289, -5.444914386472297529 ) ) ;
#21156 = EDGE_LOOP ( 'NONE', ( #2722, #19959, #21891, #1921 ) ) ;
#21157 = EDGE_CURVE ( 'NONE', #2581, #16704, #12524, .T. ) ;
#21158 = ORIENTED_EDGE ( 'NONE', *, *, #648, .F. ) ;
#21159 =( NAMED_UNIT ( * ) PLANE_ANGLE_UNIT ( ) SI_UNIT ( $, .RADIAN. ) );
#21160 = DIRECTION ( 'NONE',  ( 0.000000000000000000, -1.000000000000000000, 0.000000000000000000 ) ) ;
#21161 = CARTESIAN_POINT ( 'NONE',  ( 13.57481594606304576, 33.55859375216787299, -1.662435489736055892E-15 ) ) ;
#21162 = ADVANCED_FACE ( 'NONE', ( #1422 ), #3970, .T. ) ;
#21163 = DIRECTION ( 'NONE',  ( -0.000000000000000000, -1.000000000000000000, -0.000000000000000000 ) ) ;
#21164 = CYLINDRICAL_SURFACE ( 'NONE', #798, 2.499999999999995115 ) ;
#21165 = DIRECTION ( 'NONE',  ( 5.782411586589357392E-17, -0.000000000000000000, 1.000000000000000000 ) ) ;
#21166 = DIRECTION ( 'NONE',  ( -0.000000000000000000, -0.000000000000000000, -1.000000000000000000 ) ) ;
#21167 = VECTOR ( 'NONE', #23874, 1000.000000000000000 ) ;
#21168 = CARTESIAN_POINT ( 'NONE',  ( 13.49550141231717859, 35.99999999999999289, -0.9550757908088484127 ) ) ;
#21169 = DIRECTION ( 'NONE',  ( -5.782411586589357392E-17, 0.000000000000000000, -1.000000000000000000 ) ) ;
#21170 = CARTESIAN_POINT ( 'NONE',  ( 65.00000000000000000, -7.395377635281828788, -13.57481594606305109 ) ) ;
#21171 = EDGE_CURVE ( 'NONE', #8092, #15512, #15289, .T. ) ;
#21172 = ORIENTED_EDGE ( 'NONE', *, *, #23634, .F. ) ;
#21173 =( BOUNDED_CURVE ( )  B_SPLINE_CURVE ( 2, ( #25143, #7620, #27574 ),
 .UNSPECIFIED., .F., .T. ) 
 B_SPLINE_CURVE_WITH_KNOTS ( ( 3, 3 ),
 ( 0.5208333333333332593, 0.5249747582430949189 ),
 .UNSPECIFIED. ) 
 CURVE ( )  GEOMETRIC_REPRESENTATION_ITEM ( )  RATIONAL_B_SPLINE_CURVE ( ( 1.000000000000000888, 0.9697362687807569159, 0.9635368518655843539 ) ) 
 REPRESENTATION_ITEM ( '' )  );
#21174 = CARTESIAN_POINT ( 'NONE',  ( 3.755638155860017591, 31.78804748261757140, -13.14518615778179367 ) ) ;
#21175 = CARTESIAN_POINT ( 'NONE',  ( -13.14518615778179900, 40.50390625108394005, -5.444914386472297529 ) ) ;
#21176 = CARTESIAN_POINT ( 'NONE',  ( 99.99999999999995737, 5.000000000000018652, 3.875000002731185056 ) ) ;
#21177 = CARTESIAN_POINT ( 'NONE',  ( 116.8548138422182063, 39.11484375108394573, -5.444914386472297529 ) ) ;
#21178 = CARTESIAN_POINT ( 'NONE',  ( 70.44491438647230552, 38.42031250108393436, 13.14518615778179189 ) ) ;
#21179 = CARTESIAN_POINT ( 'NONE',  ( 204.2950502721270425, 39.66054687608393436, -9.295050272127046043 ) ) ;
#21180 = CARTESIAN_POINT ( 'NONE',  ( 57.22149563187823418, 36.00000000000000000, 10.60546543669440034 ) ) ;
#21181 = CARTESIAN_POINT ( 'NONE',  ( -13.14518615778179900, 34.15390625108393863, -5.444914386472297529 ) ) ;
#21182 = CARTESIAN_POINT ( 'NONE',  ( 55.40115559117954547, 36.13828124999999147, -9.598844408820458085 ) ) ;
#21183 = ADVANCED_FACE ( 'NONE', ( #19064, #3554 ), #12630, .T. ) ;
#21184 = DIRECTION ( 'NONE',  ( -0.000000000000000000, -1.000000000000000000, -0.000000000000000000 ) ) ;
#21185 = VECTOR ( 'NONE', #3843, 1000.000000000000000 ) ;
#21186 = CARTESIAN_POINT ( 'NONE',  ( 9.295050272127046043, 37.08085937608393579, -9.295050272127046043 ) ) ;
#21187 = LINE ( 'NONE', #7657, #12881 ) ;
#21188 = CARTESIAN_POINT ( 'NONE',  ( 98.96446609406727646, 123.2500000000000000, -2.499999999999997780 ) ) ;
#21189 = CARTESIAN_POINT ( 'NONE',  ( 4.157286354961724939, 36.00000000000000000, -12.92256159328856135 ) ) ;
#21190 = CARTESIAN_POINT ( 'NONE',  ( 101.4615807364564546, 123.6500000010924651, -1.461580736456474794 ) ) ;
#21191 = ADVANCED_FACE ( 'NONE', ( #27909 ), #5985, .F. ) ;
#21192 = CARTESIAN_POINT ( 'NONE',  ( 189.3771271284220745, 39.36289062716787157, -13.57481594606297293 ) ) ;
#21193 = CARTESIAN_POINT ( 'NONE',  ( 95.54126587499995082, -1.846868145590724986, 11.50000000136559208 ) ) ;
#21194 = DIRECTION ( 'NONE',  ( 0.000000000000000000, 0.000000000000000000, 1.000000000000000000 ) ) ;
#21195 = AXIS2_PLACEMENT_3D ( 'NONE', #2870, #5301, #13965 ) ;
#21196 = ORIENTED_EDGE ( 'NONE', *, *, #2308, .T. ) ;
#21197 = CARTESIAN_POINT ( 'NONE',  ( 99.20899822134843760, 123.0000000000000000, -1.909647267044714436 ) ) ;
#21198 = CARTESIAN_POINT ( 'NONE',  ( 5.444914386472302859, 32.26875000108393721, 13.14518615778179189 ) ) ;
#21199 = CARTESIAN_POINT ( 'NONE',  ( -13.14518615778179544, 33.40976562608393863, 0.000000000000000000 ) ) ;
#21200 = EDGE_CURVE ( 'NONE', #22694, #14819, #1672, .T. ) ;
#21201 = CARTESIAN_POINT ( 'NONE',  ( -9.598844408820454532, 32.46718750216787441, 9.598844408820459861 ) ) ;
#21202 = CARTESIAN_POINT ( 'NONE',  ( 181.4251840539369596, 36.28710937716787299, -5.622872871577872189 ) ) ;
#21203 = CARTESIAN_POINT ( 'NONE',  ( 104.4587341249999781, 84.25000000136559208, -1.846868145590750299 ) ) ;
#21204 = CARTESIAN_POINT ( 'NONE',  ( 78.14518615778179367, 39.61093750108393863, -5.444914386472297529 ) ) ;
#21205 = CARTESIAN_POINT ( 'NONE',  ( 95.00472066334982912, 103.1245878333314323, -49.07500000273118701 ) ) ;
#21206 = CARTESIAN_POINT ( 'NONE',  ( -13.14518615778179722, 40.50390625108394005, -5.444914386472297529 ) ) ;
#21207 = CARTESIAN_POINT ( 'NONE',  ( 102.0669872999999939, 124.3000000010924566, 0.8561741729129311862 ) ) ;
#21208 = CARTESIAN_POINT ( 'NONE',  ( 2.493653234604083739E-15, 34.15390625216787157, 13.57481594606304576 ) ) ;
#21209 = CARTESIAN_POINT ( 'NONE',  ( 92.99999999999998579, 110.0000000000000000, -50.49999999453763877 ) ) ;
#21210 = CARTESIAN_POINT ( 'NONE',  ( 120.4011555911795455, 39.31328124999999574, -9.598844408820458085 ) ) ;
#21211 = ORIENTED_EDGE ( 'NONE', *, *, #27672, .T. ) ;
#21212 = CARTESIAN_POINT ( 'NONE',  ( -1.887528725876408409, 53.66306546785492060, -15.00000000000000355 ) ) ;
#21213 = DIRECTION ( 'NONE',  ( -0.000000000000000000, 1.000000000000000000, -0.000000000000000000 ) ) ;
#21214 =( BOUNDED_CURVE ( )  B_SPLINE_CURVE ( 2, ( #23326, #8343, #17029, #21605, #19884 ),
 .UNSPECIFIED., .F., .F. ) 
 B_SPLINE_CURVE_WITH_KNOTS ( ( 3, 2, 3 ),
 ( 0.000000000000000000, 0.04166666666666694885, 0.08333333333333389770 ),
 .UNSPECIFIED. ) 
 CURVE ( )  GEOMETRIC_REPRESENTATION_ITEM ( )  RATIONAL_B_SPLINE_CURVE ( ( 1.000000000000000000, 0.9238795325112867385, 1.000000000000000000, 0.9238795325112857393, 1.000000000000001110 ) ) 
 REPRESENTATION_ITEM ( '' )  );
#21215 = ADVANCED_FACE ( 'NONE', ( #1350 ), #25272, .F. ) ;
#21216 = CARTESIAN_POINT ( 'NONE',  ( 95.00000000000000000, 94.43750000000001421, -2.071067811865479058 ) ) ;
#21217 = CARTESIAN_POINT ( 'NONE',  ( 78.57481594606304043, 38.27148437716787299, 5.622872871577869525 ) ) ;
#21218 = CARTESIAN_POINT ( 'NONE',  ( 95.00472066334982912, 103.1245878333314323, -55.32499999726881157 ) ) ;
#21219 = CARTESIAN_POINT ( 'NONE',  ( 5.622872871577871301, 35.29492187716788720, -13.57481594606304753 ) ) ;
#21220 = VECTOR ( 'NONE', #2210, 1000.000000000000000 ) ;
#21221 = EDGE_LOOP ( 'NONE', ( #18455, #10118, #1181, #1043 ) ) ;
#21222 = CARTESIAN_POINT ( 'NONE',  ( 94.99999999999995737, -2.071067811865466624, 10.06249999999999822 ) ) ;
#21223 = VERTEX_POINT ( 'NONE', #14838 ) ;
#21224 = CARTESIAN_POINT ( 'NONE',  ( 208.1451861577817795, 36.23750000108393010, -5.444914386472297529 ) ) ;
#21225 = DIRECTION ( 'NONE',  ( -0.000000000000000000, 1.000000000000000000, -0.000000000000000000 ) ) ;
#21226 = EDGE_CURVE ( 'NONE', #28031, #3171, #3476, .T. ) ;
#21227 = CARTESIAN_POINT ( 'NONE',  ( 116.8548138422182205, 36.63437500108393863, 5.444914386472304635 ) ) ;
#21228 = CYLINDRICAL_SURFACE ( 'NONE', #23280, 13.57481594606304398 ) ;
#21229 = CARTESIAN_POINT ( 'NONE',  ( 99.99999999999998579, 138.0000000000000000, -5.204170427930421283E-15 ) ) ;
#21230 = CARTESIAN_POINT ( 'NONE',  ( 98.15313185440923860, 94.62499999863439371, -4.458734124999994997 ) ) ;
#21231 = DIRECTION ( 'NONE',  ( -0.000000000000000000, -0.000000000000000000, 1.000000000000000000 ) ) ;
#21232 = VECTOR ( 'NONE', #7526, 1000.000000000000000 ) ;
#21233 = CARTESIAN_POINT ( 'NONE',  ( 9.295050272127047819, 39.26367187608393294, 9.295050272127046043 ) ) ;
#21234 = CARTESIAN_POINT ( 'NONE',  ( 195.0000000000000000, 38.81718749999999574, 13.57481594606304576 ) ) ;
#21235 = PRODUCT_CONTEXT ( 'NONE', #20076, 'mechanical' ) ;
#21236 = CARTESIAN_POINT ( 'NONE',  ( 99.99999999999995737, -4.999999999999990230, 8.375000002731185944 ) ) ;
#21237 = CARTESIAN_POINT ( 'NONE',  ( 99.99999999999995737, 4.458734125000016313, 4.437500001365592084 ) ) ;
#21238 = CARTESIAN_POINT ( 'NONE',  ( 59.55508561352770158, 39.11484375108394573, 13.14518615778179722 ) ) ;
#21239 = CARTESIAN_POINT ( 'NONE',  ( 103.1528011352953342, -3.152801135295355106, 4.812500001365592084 ) ) ;
#21240 = CYLINDRICAL_SURFACE ( 'NONE', #18234, 7.000000000000006217 ) ;
#21241 = CARTESIAN_POINT ( 'NONE',  ( 95.54126587499999346, 95.12499999863439371, 1.846868145590722543 ) ) ;
#21242 = AXIS2_PLACEMENT_3D ( 'NONE', #16436, #10143, #8300 ) ;
#21243 = DIRECTION ( 'NONE',  ( -0.000000000000000000, -0.000000000000000000, -1.000000000000000000 ) ) ;
#21244 = CARTESIAN_POINT ( 'NONE',  ( -13.57481594606304576, 38.66835937499999432, 5.622872871577880183 ) ) ;
#21245 = CARTESIAN_POINT ( 'NONE',  ( 116.8548138422182063, 40.00781250108393294, 5.444914386472304635 ) ) ;
#21246 = ORIENTED_EDGE ( 'NONE', *, *, #12984, .T. ) ;
#21247 = CARTESIAN_POINT ( 'NONE',  ( 95.54126587499995082, 82.62500000136560629, -1.846868145590750077 ) ) ;
#21248 = CARTESIAN_POINT ( 'NONE',  ( 98.96446609406724804, 124.1500000021849672, -2.499999999999992450 ) ) ;
#21249 = ORIENTED_EDGE ( 'NONE', *, *, #2022, .T. ) ;
#21250 = CARTESIAN_POINT ( 'NONE',  ( 102.1631189606246153, 116.6573956140660897, -45.60000000000001563 ) ) ;
#21251 = CARTESIAN_POINT ( 'NONE',  ( 51.85481384221820633, 35.24531250108393721, 5.444914386472304635 ) ) ;
#21252 = EDGE_LOOP ( 'NONE', ( #92, #11174, #26294, #10814 ) ) ;
#21253 = CIRCLE ( 'NONE', #24898, 7.000000000000006217 ) ;
#21254 = CARTESIAN_POINT ( 'NONE',  ( 5.622872871577786924, 32.51679687499999716, 13.57481594606313813 ) ) ;
#21255 = CARTESIAN_POINT ( 'NONE',  ( 104.4587341249999781, 1.846868145590750299, 6.250000001365592084 ) ) ;
#21256 = ORIENTED_EDGE ( 'NONE', *, *, #27057, .F. ) ;
#21257 = LINE ( 'NONE', #25945, #6585 ) ;
#21258 = CARTESIAN_POINT ( 'NONE',  ( 2.414731522848535132E-15, 32.81445312608393294, 13.14518615778179544 ) ) ;
#21259 = CARTESIAN_POINT ( 'NONE',  ( 208.5748159460630688, 38.32109375216786873, -1.662435489736055892E-15 ) ) ;
#21260 = CARTESIAN_POINT ( 'NONE',  ( -13.14518615778179189, 39.01562500108393294, 5.444914386472304635 ) ) ;
#21261 = DIRECTION ( 'NONE',  ( -0.000000000000000000, -1.000000000000000000, -0.000000000000000000 ) ) ;
#21262 = CARTESIAN_POINT ( 'NONE',  ( 198.6364962467981456, 51.46815297079464813, 14.99999999999995381 ) ) ;
#21263 = CARTESIAN_POINT ( 'NONE',  ( 124.5550856135277087, 40.60312500108393863, -13.14518615778179722 ) ) ;
#21264 = CARTESIAN_POINT ( 'NONE',  ( 9.295050272127046043, 39.66054687608393436, -9.295050272127046043 ) ) ;
#21265 = CARTESIAN_POINT ( 'NONE',  ( 74.59884440882045453, 39.11484374999999858, -9.598844408820458085 ) ) ;
#21266 = DIRECTION ( 'NONE',  ( -0.000000000000000000, 1.000000000000000000, -0.000000000000000000 ) ) ;
#21267 = DIRECTION ( 'NONE',  ( -0.8660254037844380415, 0.5000000000000013323, 0.000000000000000000 ) ) ;
#21268 = CARTESIAN_POINT ( 'NONE',  ( 104.4587341249999639, 1.442382525525748735E-14, 2.937500001365592528 ) ) ;
#21269 = CARTESIAN_POINT ( 'NONE',  ( 13.14518615778179900, 32.46718750108393436, -5.444914386472297529 ) ) ;
#21270 = CARTESIAN_POINT ( 'NONE',  ( 96.84719886470459471, 3.152801135295383084, 1.562500001365592972 ) ) ;
#21271 = CIRCLE ( 'NONE', #818, 2.999999999999989786 ) ;
#21272 = CARTESIAN_POINT ( 'NONE',  ( 98.15313185440923860, 84.50000000136560629, -4.458734125000016313 ) ) ;
#21273 = CARTESIAN_POINT ( 'NONE',  ( 5.444914386472297529, 32.36796875108393579, -13.14518615778179900 ) ) ;
#21274 = CARTESIAN_POINT ( 'NONE',  ( 5.444914386472302859, 40.20625000108394431, 13.14518615778179189 ) ) ;
#21275 = CYLINDRICAL_SURFACE ( 'NONE', #20166, 13.57481594606304398 ) ;
#21276 = ORIENTED_EDGE ( 'NONE', *, *, #25620, .F. ) ;
#21277 = CARTESIAN_POINT ( 'NONE',  ( 3.755639919285892248, 31.78804746655075775, -13.14518615778179544 ) ) ;
#21278 = CARTESIAN_POINT ( 'NONE',  ( 94.33688103937535629, 105.8855032339526758, -54.29999999453764303 ) ) ;
#21279 = DIRECTION ( 'NONE',  ( -1.000000000000000000, -0.000000000000000000, 2.385244779468110248E-16 ) ) ;
#21280 = CARTESIAN_POINT ( 'NONE',  ( 100.0000000000000000, 110.0000000000000000, -45.00000000000000711 ) ) ;
#21281 = CARTESIAN_POINT ( 'NONE',  ( 97.50236033167490746, 102.3130555110000159, -53.47499999726882436 ) ) ;
#21282 = EDGE_CURVE ( 'NONE', #14317, #947, #18391, .T. ) ;
#21283 = CARTESIAN_POINT ( 'NONE',  ( 99.99999999999995737, 80.75000000000000000, -5.000000000000018652 ) ) ;
#21284 = ORIENTED_EDGE ( 'NONE', *, *, #18072, .F. ) ;
#21285 = CARTESIAN_POINT ( 'NONE',  ( 59.55508561352770158, 38.22187500108393721, -13.14518615778179722 ) ) ;
#21286 = CARTESIAN_POINT ( 'NONE',  ( 0.000000000000000000, 1.000000000000000000, 0.000000000000000000 ) ) ;
#21287 = CARTESIAN_POINT ( 'NONE',  ( 208.1451861577817795, 32.46718750108393436, -5.444914386472297529 ) ) ;
#21288 = VERTEX_POINT ( 'NONE', #25420 ) ;
#21289 = FACE_OUTER_BOUND ( 'NONE', #13737, .T. ) ;
#21290 = DIRECTION ( 'NONE',  ( 1.000000000000000000, 0.000000000000000000, 0.000000000000000000 ) ) ;
#21291 = CARTESIAN_POINT ( 'NONE',  ( 100.8561741729129295, 123.4000000010924794, 2.066987299999979211 ) ) ;
#21292 = AXIS2_PLACEMENT_3D ( 'NONE', #8700, #21828, #25805 ) ;
#21293 = VECTOR ( 'NONE', #4007, 1000.000000000000000 ) ;
#21294 = CARTESIAN_POINT ( 'NONE',  ( 139.5988444088204403, 35.24531250216787726, -9.598844408820458085 ) ) ;
#21295 =( BOUNDED_CURVE ( )  B_SPLINE_CURVE ( 2, ( #15158, #21751, #23463, #12742, #14882, #8487, #12600, #17453, #23325 ),
 .UNSPECIFIED., .F., .T. ) 
 B_SPLINE_CURVE_WITH_KNOTS ( ( 3, 2, 2, 2, 3 ),
 ( 0.2857142857142856984, 0.2946428571428571508, 0.3035714285714284921, 0.3124999999999999445, 0.3214285714285713969 ),
 .UNSPECIFIED. ) 
 CURVE ( )  GEOMETRIC_REPRESENTATION_ITEM ( )  RATIONAL_B_SPLINE_CURVE ( ( 1.000000000000000000, 0.9238795325112867385, 1.000000000000000000, 0.9238795325112867385, 1.000000000000000000, 0.9238795325112867385, 1.000000000000000000, 0.9238795325112871826, 0.9999999999999995559 ) ) 
 REPRESENTATION_ITEM ( '' )  );
#21296 = CARTESIAN_POINT ( 'NONE',  ( 102.0710678118654329, 81.81250000273118417, -4.999999999999992006 ) ) ;
#21297 = CARTESIAN_POINT ( 'NONE',  ( 84.99999999999998579, 118.0000000000000000, -43.00000000000000000 ) ) ;
#21298 = CARTESIAN_POINT ( 'NONE',  ( 200.4449143864723055, 37.32890625108393579, -13.14518615778179900 ) ) ;
#21299 = ORIENTED_EDGE ( 'NONE', *, *, #27513, .T. ) ;
#21300 = EDGE_LOOP ( 'NONE', ( #7567, #7145, #3198, #4717, #7916 ) ) ;
#21301 = CARTESIAN_POINT ( 'NONE',  ( -13.14518615778179189, 34.25312500108393010, 5.444914386472304635 ) ) ;
#21302 = CARTESIAN_POINT ( 'NONE',  ( -2.921131288499653970E-15, 21.36169591142201440, -23.85284712729792389 ) ) ;
#21303 = CARTESIAN_POINT ( 'NONE',  ( 13.57481594606304753, 38.27148437500000711, -5.622872871577873966 ) ) ;
#21304 = CARTESIAN_POINT ( 'NONE',  ( 98.15313185440923860, 84.25000000136559208, -4.458734125000016313 ) ) ;
#21305 = CARTESIAN_POINT ( 'NONE',  ( 78.57481594606305464, 39.85898437716787157, 5.622872871577868636 ) ) ;
#21306 = DIRECTION ( 'NONE',  ( -0.000000000000000000, -1.000000000000000000, -0.000000000000000000 ) ) ;
#21307 = DIRECTION ( 'NONE',  ( 0.000000000000000000, 0.000000000000000000, -1.000000000000000000 ) ) ;
#21308 = CARTESIAN_POINT ( 'NONE',  ( 103.5355339059327093, -3.535533905932726206, 6.374999999999999112 ) ) ;
#21309 = CARTESIAN_POINT ( 'NONE',  ( 102.4976396683250783, 102.3130555110000159, -47.02499999726882152 ) ) ;
#21310 = VECTOR ( 'NONE', #17909, 1000.000000000000000 ) ;
#21311 = EDGE_LOOP ( 'NONE', ( #6133, #12427, #14632, #1879 ) ) ;
#21312 = CARTESIAN_POINT ( 'NONE',  ( -9.598844408820454532, 40.30546874999999574, 9.598844408820459861 ) ) ;
#21313 = CARTESIAN_POINT ( 'NONE',  ( 13.14518615778179544, 39.36289062608393152, -1.609821015232357215E-15 ) ) ;
#21314 = PRODUCT_DEFINITION_FORMATION_WITH_SPECIFIED_SOURCE ( 'ANY', '', #11714, .NOT_KNOWN. ) ;
#21315 = CARTESIAN_POINT ( 'NONE',  ( 103.1528011352953342, 3.152801135295383084, 14.06250000136559208 ) ) ;
#21316 = CARTESIAN_POINT ( 'NONE',  ( 143.1451861577818079, 39.51171875108392584, 5.444914386472293977 ) ) ;
#21317 = EDGE_CURVE ( 'NONE', #3877, #16151, #7817, .T. ) ;
#21318 = CARTESIAN_POINT ( 'NONE',  ( 51.85481384221820633, 38.22187500108393010, 5.444914386472304635 ) ) ;
#21319 = CARTESIAN_POINT ( 'NONE',  ( 204.2950502721270425, 39.46210937608393721, 9.295050272127046043 ) ) ;
#21320 = EDGE_CURVE ( 'NONE', #7134, #4950, #3621, .T. ) ;
#21321 = ORIENTED_EDGE ( 'NONE', *, *, #5151, .T. ) ;
#21322 = CARTESIAN_POINT ( 'NONE',  ( -15.00000000000000000, 55.00000000000000000, 9.999999999999998224 ) ) ;
#21323 = CARTESIAN_POINT ( 'NONE',  ( -5.444914386472299306, 36.73359375108393010, 13.14518615778179722 ) ) ;
#21324 = CARTESIAN_POINT ( 'NONE',  ( 188.5294363033335685, 36.00000000000000711, -11.78199955157030487 ) ) ;
#21325 = DIRECTION ( 'NONE',  ( 0.000000000000000000, 0.8660254037844380415, 0.5000000000000009992 ) ) ;
#21326 = CARTESIAN_POINT ( 'NONE',  ( 124.3771271284220745, 40.05742187499998863, -13.57481594606297293 ) ) ;
#21327 = CARTESIAN_POINT ( 'NONE',  ( -9.295050272127046043, 39.66054687608393436, -9.295050272127046043 ) ) ;
#21328 = CARTESIAN_POINT ( 'NONE',  ( 6.079080020518838445, 54.65154858643462177, 14.99999999999999645 ) ) ;
#21329 = CARTESIAN_POINT ( 'NONE',  ( 102.4999999999999858, 123.8069999999781459, -9.847140817659276890E-15 ) ) ;
#21330 = AXIS2_PLACEMENT_3D ( 'NONE', #26469, #15617, #10910 ) ;
#21331 = AXIS2_PLACEMENT_3D ( 'NONE', #16128, #27131, #16417 ) ;
#21332 = EDGE_CURVE ( 'NONE', #11286, #20591, #4737, .T. ) ;
#21333 = CARTESIAN_POINT ( 'NONE',  ( 97.93301269999999192, 124.7000000010924623, -0.8561741729129505041 ) ) ;
#21334 = CARTESIAN_POINT ( 'NONE',  ( 99.99999999999998579, 123.7500000010924737, -2.066987299999998751 ) ) ;
#21335 = AXIS2_PLACEMENT_3D ( 'NONE', #5148, #13812, #22534 ) ;
#21336 = CARTESIAN_POINT ( 'NONE',  ( 104.9999999999999716, 1.449011120738813565E-14, 12.49999999999999822 ) ) ;
#21337 = CARTESIAN_POINT ( 'NONE',  ( 103.5355339059327093, -3.535533905932726206, 13.50000000273118417 ) ) ;
#21338 = ORIENTED_EDGE ( 'NONE', *, *, #21370, .T. ) ;
#21339 = CARTESIAN_POINT ( 'NONE',  ( 95.67376207875072680, 104.0454443415356991, -53.69999999999999574 ) ) ;
#21340 = CARTESIAN_POINT ( 'NONE',  ( 3.755638155860017591, 31.78804748261757140, -13.14518615778179367 ) ) ;
#21341 = CARTESIAN_POINT ( 'NONE',  ( 195.0000000000000000, -7.395377635281828788, -13.57481594606306707 ) ) ;
#21342 = CARTESIAN_POINT ( 'NONE',  ( -9.598844408820454532, 34.05468750216788010, 9.598844408820459861 ) ) ;
#21343 = DIRECTION ( 'NONE',  ( -0.000000000000000000, -1.000000000000000000, -0.000000000000000000 ) ) ;
#21344 = CARTESIAN_POINT ( 'NONE',  ( 104.4587341249999781, 79.87500000136559208, 1.846868145590721655 ) ) ;
#21345 = CARTESIAN_POINT ( 'NONE',  ( 55.70494972787295751, 38.46992187608393721, 9.295050272127047819 ) ) ;
#21346 =( BOUNDED_SURFACE ( )  B_SPLINE_SURFACE ( 3, 2, ( 
 ( #24027, #17323, #13020 ),
 ( #13305, #26019, #21473 ),
 ( #19887, #4505, #13162 ),
 ( #373, #2087, #23606 ),
 ( #2234, #2375, #15164 ),
 ( #9057, #17749, #19742 ),
 ( #4085, #10618, #226 ),
 ( #19324, #28026, #8492 ),
 ( #25884, #6353, #15026 ),
 ( #7473, #17890, #18319 ),
 ( #2925, #945, #7332 ),
 ( #20464, #24592, #5074 ),
 ( #9196, #11739, #1088 ),
 ( #5357, #13736, #2791 ),
 ( #9616, #11596, #26597 ),
 ( #27027, #9755, #22460 ),
 ( #16168, #2651, #24446 ),
 ( #15742, #22745, #11456 ),
 ( #11314, #18026, #18465 ),
 ( #7183, #24877, #20316 ) ),
 .UNSPECIFIED., .F., .F., .F. ) 
 B_SPLINE_SURFACE_WITH_KNOTS ( ( 4, 2, 2, 2, 2, 2, 2, 2, 2, 4 ),
 ( 3, 3 ),
 ( 0.009073803551359463371, 0.01139250602759181788, 0.01371120850382417239, 0.01602991098005652690, 0.01834861345628888141, 0.01950796469440505693, 0.02066731593252123592, 0.02298601840875359043, 0.02530472088498594146, 0.02762342336121829597 ),
 ( 0.000000000000000000, 1.000000000000000000 ),
 .UNSPECIFIED. ) 
 GEOMETRIC_REPRESENTATION_ITEM ( )  RATIONAL_B_SPLINE_SURFACE ( (
 ( 1.000000000000000000, 0.7071067811865473507, 1.000000000000000000),
 ( 1.000000000000000000, 0.7344871497828887597, 1.000000000000000000),
 ( 1.000000000000000000, 0.7612510203318868518, 1.000000000000000000),
 ( 1.000000000000000000, 0.8116663633844006798, 1.000000000000000000),
 ( 1.000000000000000000, 0.8353358059751632148, 1.000000000000000000),
 ( 1.000000000000000000, 0.8764699612586239752, 1.000000000000000000),
 ( 1.000000000000000000, 0.8939017358720021678, 1.000000000000000000),
 ( 1.000000000000000000, 0.9185314935646265999, 1.000000000000000000),
 ( 1.000000000000000000, 0.9256439951239476827, 1.000000000000000000),
 ( 1.000000000000000000, 0.9261623622476511386, 1.000000000000000000),
 ( 1.000000000000000000, 0.9246301385978846765, 1.000000000000000000),
 ( 1.000000000000000000, 0.9183304321348021437, 1.000000000000000000),
 ( 1.000000000000000000, 0.9135987334168410579, 1.000000000000000000),
 ( 1.000000000000000000, 0.8954110486039674743, 1.000000000000000000),
 ( 1.000000000000000000, 0.8779877431163538581, 1.000000000000000000),
 ( 1.000000000000000000, 0.8366182664709980177, 1.000000000000000000),
 ( 1.000000000000000000, 0.8126941604015293086, 1.000000000000000000),
 ( 1.000000000000000000, 0.7617527316305964247, 1.000000000000000000),
 ( 1.000000000000000000, 0.7347103785791970765, 1.000000000000000000),
 ( 1.000000000000000000, 0.7071067811865467956, 1.000000000000000000) ) ) 
 REPRESENTATION_ITEM ( '' )  SURFACE ( )  );
#21347 = CARTESIAN_POINT ( 'NONE',  ( 104.9952793366501851, 116.8754121666685393, -48.07500000273119412 ) ) ;
#21348 = CARTESIAN_POINT ( 'NONE',  ( 13.14518615778179544, 40.15664062608393436, -1.609821015232357215E-15 ) ) ;
#21349 = ORIENTED_EDGE ( 'NONE', *, *, #15599, .T. ) ;
#21350 = CARTESIAN_POINT ( 'NONE',  ( 101.4615807364564546, 124.2500000010924737, 1.461580736456455476 ) ) ;
#21351 = CARTESIAN_POINT ( 'NONE',  ( 51.42518405393695957, 38.71796875216787726, 0.000000000000000000 ) ) ;
#21352 = CARTESIAN_POINT ( 'NONE',  ( 92.99999999999998579, 110.0000000000000000, -54.49999999453763877 ) ) ;
#21353 = CARTESIAN_POINT ( 'NONE',  ( 143.5748159460630688, 40.60312499999999858, -1.662435489736055892E-15 ) ) ;
#21354 = ORIENTED_EDGE ( 'NONE', *, *, #26500, .F. ) ;
#21355 = CARTESIAN_POINT ( 'NONE',  ( 99.99999999999997158, 102.6397644303321215, -51.99999999453763877 ) ) ;
#21356 = CARTESIAN_POINT ( 'NONE',  ( 99.99999999999995737, 85.00000000000000000, -1.387778780781445676E-14 ) ) ;
#21357 = CARTESIAN_POINT ( 'NONE',  ( 9.598844408820459861, 39.80937500216786873, 9.598844408820456309 ) ) ;
#21358 = CARTESIAN_POINT ( 'NONE',  ( 124.5550856135277087, 39.90859375108393436, 13.14518615778179722 ) ) ;
#21359 = EDGE_CURVE ( 'NONE', #25944, #8379, #5902, .T. ) ;
#21360 = CARTESIAN_POINT ( 'NONE',  ( 78.57481594606304043, 35.89023437716787868, 5.622872871577869525 ) ) ;
#21361 = CARTESIAN_POINT ( 'NONE',  ( 108.0825317500000011, 110.0000000000000000, -54.62499999726882294 ) ) ;
#21362 = CARTESIAN_POINT ( 'NONE',  ( -13.57481594606304576, 37.13046875216787868, 0.000000000000000000 ) ) ;
#21363 = EDGE_LOOP ( 'NONE', ( #19728, #5625, #1489, #11284 ) ) ;
#21364 = AXIS2_PLACEMENT_3D ( 'NONE', #19548, #19403, #21554 ) ;
#21365 = EDGE_CURVE ( 'NONE', #14731, #25689, #4391, .T. ) ;
#21366 = CARTESIAN_POINT ( 'NONE',  ( 97.92893218813451028, 5.000000000000018652, 4.812500000000000000 ) ) ;
#21367 = VERTEX_POINT ( 'NONE', #21283 ) ;
#21368 = CARTESIAN_POINT ( 'NONE',  ( 195.0000000000000000, 37.97382812608393721, -13.14518615778179544 ) ) ;
#21369 = CARTESIAN_POINT ( 'NONE',  ( 99.99999999999998579, 110.0000000000000000, -145.0000000000000284 ) ) ;
#21370 = EDGE_CURVE ( 'NONE', #3896, #13477, #15626, .T. ) ;
#21371 = CARTESIAN_POINT ( 'NONE',  ( 143.1451861577818363, 38.51953125108393294, 5.444914386472293977 ) ) ;
#21372 = LINE ( 'NONE', #12914, #14505 ) ;
#21373 = FACE_OUTER_BOUND ( 'NONE', #24170, .T. ) ;
#21374 = CARTESIAN_POINT ( 'NONE',  ( 104.4587341249999923, 94.24999999863439371, 1.846868145590726318 ) ) ;
#21375 = DIRECTION ( 'NONE',  ( -0.000000000000000000, -1.000000000000000000, -0.000000000000000000 ) ) ;
#21376 = CARTESIAN_POINT ( 'NONE',  ( 5.444914386472297529, 39.51171875108392584, -13.14518615778179900 ) ) ;
#21377 = CARTESIAN_POINT ( 'NONE',  ( 200.6228728715778686, 36.78320312499999289, -13.57481594606304753 ) ) ;
#21378 = APPLICATION_PROTOCOL_DEFINITION ( 'draft international standard', 'automotive_design', 1998, #10768 ) ;
#21379 = CARTESIAN_POINT ( 'NONE',  ( 97.92893218813451028, -4.999999999999989342, 8.312500002731185944 ) ) ;
#21380 = CARTESIAN_POINT ( 'NONE',  ( 95.54126587499995082, -1.846868145590724986, 4.750000001365592084 ) ) ;
#21381 = CARTESIAN_POINT ( 'NONE',  ( 78.14518615778179367, 40.15664062608393436, -1.609821015232357215E-15 ) ) ;
#21382 = CARTESIAN_POINT ( 'NONE',  ( 103.1528011352953342, -3.152801135295355106, 7.812500001365592084 ) ) ;
#21383 = CARTESIAN_POINT ( 'NONE',  ( 95.67376207875072680, 104.0454443415356991, -44.20000000546236407 ) ) ;
#21384 = PRESENTATION_LAYER_ASSIGNMENT (  '', '', ( #5458 ) ) ;
#21385 = CARTESIAN_POINT ( 'NONE',  ( 103.1528011352953484, 93.43749999863440792, -3.152801135295366208 ) ) ;
#21386 = CIRCLE ( 'NONE', #450, 13.57481594606304398 ) ;
#21387 = CARTESIAN_POINT ( 'NONE',  ( 130.0000000000000000, 39.21406249999999716, -13.57481594606304576 ) ) ;
#21388 = CARTESIAN_POINT ( 'NONE',  ( 13.57481594606304931, 38.17226562499999432, 5.622872871577869525 ) ) ;
#21389 = CARTESIAN_POINT ( 'NONE',  ( 93.00000000000000000, 107.7255621263696668, -45.90000000000000568 ) ) ;
#21390 = ORIENTED_EDGE ( 'NONE', *, *, #2971, .T. ) ;
#21391 = CARTESIAN_POINT ( 'NONE',  ( 104.4587341249999781, 84.12500000136560629, 1.846868145590721655 ) ) ;
#21392 = CARTESIAN_POINT ( 'NONE',  ( -13.57481594606304753, 31.52460937716787370, -5.622872871577872189 ) ) ;
#21393 = ORIENTED_EDGE ( 'NONE', *, *, #18203, .F. ) ;
#21394 = VECTOR ( 'NONE', #16746, 1000.000000000000000 ) ;
#21395 = CARTESIAN_POINT ( 'NONE',  ( 99.99999999999997158, 102.6397644303321215, -46.50000000000001421 ) ) ;
#21396 = CARTESIAN_POINT ( 'NONE',  ( 74.29505027212704249, 34.89804687608393863, -9.295050272127046043 ) ) ;
#21397 = EDGE_LOOP ( 'NONE', ( #26565, #16859, #18290, #10362 ) ) ;
#21398 = DIRECTION ( 'NONE',  ( -0.000000000000000000, -0.000000000000000000, -1.000000000000000000 ) ) ;
#21399 = ADVANCED_FACE ( 'NONE', ( #14430 ), #1085, .T. ) ;
#21400 = CARTESIAN_POINT ( 'NONE',  ( 103.1528011352953342, 3.152801135295383084, 2.312500001365592084 ) ) ;
#21401 = EDGE_LOOP ( 'NONE', ( #25811, #27845, #25402, #17870 ) ) ;
#21402 = CARTESIAN_POINT ( 'NONE',  ( -13.09590655363597733, 35.99999999999999289, 1.137167824541468031 ) ) ;
#21403 = CARTESIAN_POINT ( 'NONE',  ( 5.444914386472302859, 34.45156250108393436, 13.14518615778179189 ) ) ;
#21404 = CARTESIAN_POINT ( 'NONE',  ( 185.4011555911795313, 38.61875000216787157, -9.598844408820458085 ) ) ;
#21405 = CARTESIAN_POINT ( 'NONE',  ( -13.14518615778179722, 38.12265625108393863, -5.444914386472297529 ) ) ;
#21406 = CARTESIAN_POINT ( 'NONE',  ( 214.9999999999999716, 75.00000000000000000, 9.999999999999946709 ) ) ;
#21407 = CARTESIAN_POINT ( 'NONE',  ( 124.5550856135277087, 39.31328125108392868, 13.14518615778179722 ) ) ;
#21409 = AXIS2_PLACEMENT_3D ( 'NONE', #25202, #7527, #24782 ) ;
#21408 = CARTESIAN_POINT ( 'NONE',  ( -5.444914386472299306, 39.31328125108394289, 13.14518615778179722 ) ) ;
#21410 = ORIENTED_EDGE ( 'NONE', *, *, #27520, .F. ) ;
#21411 = CARTESIAN_POINT ( 'NONE',  ( 74.59884440882045453, 36.53515624999999289, 9.598844408820456309 ) ) ;
#21412 = DIRECTION ( 'NONE',  ( 0.000000000000000000, 0.000000000000000000, -1.000000000000000000 ) ) ;
#21413 = CARTESIAN_POINT ( 'NONE',  ( 101.8468681455906903, 4.458734125000016313, 1.125000001365592750 ) ) ;
#21414 = CARTESIAN_POINT ( 'NONE',  ( 5.622872871577912157, 38.17226562716787441, 13.57481594606301023 ) ) ;
#21415 = CARTESIAN_POINT ( 'NONE',  ( 101.8468681455906903, 4.458734125000016313, 5.125000001365592972 ) ) ;
#21416 = CARTESIAN_POINT ( 'NONE',  ( 99.99999999999998579, 118.4984768113314004, -51.62500000273119127 ) ) ;
#21417 = CARTESIAN_POINT ( 'NONE',  ( 96.84719886470459471, 3.152801135295383084, 2.562500001365592084 ) ) ;
#21418 = CARTESIAN_POINT ( 'NONE',  ( 104.4587341249999781, 80.12500000136560629, 1.846868145590721655 ) ) ;
#21419 = CARTESIAN_POINT ( 'NONE',  ( 13.14518615778179900, 33.06250000108393294, -5.444914386472297529 ) ) ;
#21420 = CARTESIAN_POINT ( 'NONE',  ( -9.295050272127046043, 40.65273437608393436, -9.295050272127046043 ) ) ;
#21421 = CARTESIAN_POINT ( 'NONE',  ( 108.0825317500000011, 110.0000000000000000, -46.87499999726882294 ) ) ;
#21422 = ORIENTED_EDGE ( 'NONE', *, *, #19587, .T. ) ;
#21423 = CARTESIAN_POINT ( 'NONE',  ( 195.0000000000000000, 50.00000000000000000, -2.255140518769849538E-14 ) ) ;
#21424 = CARTESIAN_POINT ( 'NONE',  ( 100.8561741729129295, 124.3000000010924850, -2.066987299999998751 ) ) ;
#21425 = CARTESIAN_POINT ( 'NONE',  ( 103.5355339059327093, 3.535533905932755072, 5.625000000000000000 ) ) ;
#21426 = CARTESIAN_POINT ( 'NONE',  ( -13.57481594606304753, 40.15664062499999432, -5.622872871577872189 ) ) ;
#21427 = VECTOR ( 'NONE', #1749, 1000.000000000000000 ) ;
#21428 = CARTESIAN_POINT ( 'NONE',  ( 181.8548138422181921, 38.91640625108393436, -5.444914386472297529 ) ) ;
#21429 = VERTEX_POINT ( 'NONE', #20873 ) ;
#21430 = CARTESIAN_POINT ( 'NONE',  ( 51.85481384221821344, 39.21406250108392300, 5.444914386472304635 ) ) ;
#21431 = DIRECTION ( 'NONE',  ( 0.000000000000000000, -1.000000000000000000, 0.000000000000000000 ) ) ;
#21432 = CARTESIAN_POINT ( 'NONE',  ( 130.0000000000000000, 36.13828125216787157, -13.57481594606304576 ) ) ;
#21433 = VERTEX_POINT ( 'NONE', #14574 ) ;
#21434 = CARTESIAN_POINT ( 'NONE',  ( 105.6631189606246295, 114.1144967660473242, -50.80000000000000426 ) ) ;
#21435 = CARTESIAN_POINT ( 'NONE',  ( 0.000000000000000000, 0.000000000000000000, 23.26794919243112858 ) ) ;
#21436 = CARTESIAN_POINT ( 'NONE',  ( 104.9999999999999716, 92.81249999726880162, 2.071067811865467956 ) ) ;
#21437 = CARTESIAN_POINT ( 'NONE',  ( 130.0000000000000000, 34.55078125216787299, -13.57481594606304576 ) ) ;
#21438 = CARTESIAN_POINT ( 'NONE',  ( 195.0000000000000000, 40.80156249999999574, -13.57481594606304576 ) ) ;
#21439 = CARTESIAN_POINT ( 'NONE',  ( -15.00000000000000355, 75.00000000000000000, -9.999999999999998224 ) ) ;
#21440 = VECTOR ( 'NONE', #14782, 1000.000000000000000 ) ;
#21441 = CARTESIAN_POINT ( 'NONE',  ( 189.5550856135277229, 33.45937500108394147, -13.14518615778179900 ) ) ;
#21442 = VERTEX_POINT ( 'NONE', #21432 ) ;
#21443 = ADVANCED_FACE ( 'NONE', ( #7756 ), #10021, .T. ) ;
#21444 = ORIENTED_EDGE ( 'NONE', *, *, #28153, .T. ) ;
#21445 = CARTESIAN_POINT ( 'NONE',  ( -9.295050272127046043, 38.27148437608393294, -9.295050272127046043 ) ) ;
#21446 = CARTESIAN_POINT ( 'NONE',  ( 103.1528011352953342, 3.152801135295383084, 14.31250000136559208 ) ) ;
#21447 = CARTESIAN_POINT ( 'NONE',  ( 78.14518615778179367, 39.36289062608393152, -1.609821015232357215E-15 ) ) ;
#21448 = CARTESIAN_POINT ( 'NONE',  ( 95.54126587499996504, 79.50000000136560629, 1.846868145590724986 ) ) ;
#21449 = CARTESIAN_POINT ( 'NONE',  ( 101.7677669209684552, 123.0000000000000000, 1.767766984964258992 ) ) ;
#21450 = CIRCLE ( 'NONE', #10504, 25.00000000000001066 ) ;
#21451 = DIRECTION ( 'NONE',  ( 1.000000000000000000, 0.000000000000000000, -5.782411586589357392E-17 ) ) ;
#21452 = CYLINDRICAL_SURFACE ( 'NONE', #28054, 13.57481594606304398 ) ;
#21453 = CARTESIAN_POINT ( 'NONE',  ( 181.8548138422182205, 39.90859375108393436, -5.444914386472297529 ) ) ;
#21454 = CARTESIAN_POINT ( 'NONE',  ( 91.91746824999998466, 110.0000000000000000, -45.62499999726882294 ) ) ;
#21455 = ORIENTED_EDGE ( 'NONE', *, *, #19965, .T. ) ;
#21456 = CARTESIAN_POINT ( 'NONE',  ( 13.57481594606304576, 40.60312499999999858, -1.662435489736055892E-15 ) ) ;
#21457 = CARTESIAN_POINT ( 'NONE',  ( -13.14518615778179544, 38.96601562608393721, 0.000000000000000000 ) ) ;
#21458 = CARTESIAN_POINT ( 'NONE',  ( 103.5355339059327093, 3.535533905932755072, 1.750000002731184834 ) ) ;
#21459 = CARTESIAN_POINT ( 'NONE',  ( 120.7049497278729575, 35.89023437608393152, -9.295050272127046043 ) ) ;
#21460 = CARTESIAN_POINT ( 'NONE',  ( 59.55508561352770158, 37.52734375108393294, 13.14518615778179722 ) ) ;
#21461 = CARTESIAN_POINT ( 'NONE',  ( 195.0000000000000000, 32.02070312608393010, 13.14518615778179544 ) ) ;
#21462 = EDGE_LOOP ( 'NONE', ( #3076, #26558, #22036, #14840 ) ) ;
#21463 = CARTESIAN_POINT ( 'NONE',  ( 65.27033697766381692, 35.99999999999999289, 13.14949859323921366 ) ) ;
#21464 = CARTESIAN_POINT ( 'NONE',  ( -13.14518615778179189, 35.84062500108394289, 5.444914386472304635 ) ) ;
#21465 = CARTESIAN_POINT ( 'NONE',  ( 123.8801563722988703, 51.28708186914935396, -14.99999999999929834 ) ) ;
#21466 =( BOUNDED_CURVE ( )  B_SPLINE_CURVE ( 2, ( #19286, #4318, #14987, #185, #8587, #8867, #17276, #4743, #6449 ),
 .UNSPECIFIED., .F., .T. ) 
 B_SPLINE_CURVE_WITH_KNOTS ( ( 3, 2, 2, 2, 3 ),
 ( 0.1041666666666664909, 0.1145833333333332732, 0.1250000000000000833, 0.1354166666666668517, 0.1458333333333336757 ),
 .UNSPECIFIED. ) 
 CURVE ( )  GEOMETRIC_REPRESENTATION_ITEM ( )  RATIONAL_B_SPLINE_CURVE ( ( 1.000000000000001332, 0.9238795325112854062, 1.000000000000000000, 0.9238795325112867385, 1.000000000000000000, 0.9238795325112867385, 1.000000000000000000, 0.9238795325112842960, 1.000000000000002442 ) ) 
 REPRESENTATION_ITEM ( '' )  );
#21467 = CARTESIAN_POINT ( 'NONE',  ( 130.0000000000000000, 50.00000000000000000, -1.503427012513233026E-14 ) ) ;
#21468 = DIRECTION ( 'NONE',  ( 1.000000000000000000, 0.000000000000000000, 0.000000000000000000 ) ) ;
#21469 = EDGE_LOOP ( 'NONE', ( #19854, #18791, #4778, #13587 ) ) ;
#21470 = CARTESIAN_POINT ( 'NONE',  ( 2.414731522848535132E-15, 39.95820312608393010, 13.14518615778179544 ) ) ;
#21471 = CARTESIAN_POINT ( 'NONE',  ( -0.8421075954646584094, 53.50112910130383170, 14.99999999999999645 ) ) ;
#21472 = CARTESIAN_POINT ( 'NONE',  ( 98.23223304703363112, 122.6000000021849559, -1.767766952966370209 ) ) ;
#21473 = CARTESIAN_POINT ( 'NONE',  ( 56.59768421877713251, 54.99999999485619639, 14.99999999999998401 ) ) ;
#21474 = CARTESIAN_POINT ( 'NONE',  ( 98.15313185440925281, -4.458734124999987891, 7.625000001365592084 ) ) ;
#21475 = CARTESIAN_POINT ( 'NONE',  ( 104.3262379212492590, 104.0454443415356991, -47.80000000546237260 ) ) ;
#21476 = CARTESIAN_POINT ( 'NONE',  ( 99.99999999999995737, 4.458734125000016313, 13.18750000136559208 ) ) ;
#21477 = CARTESIAN_POINT ( 'NONE',  ( 9.295050272127047819, 32.91367187608393152, 9.295050272127046043 ) ) ;
#21478 = CARTESIAN_POINT ( 'NONE',  ( -5.444914386472297529, 39.61093750108393152, -13.14518615778179900 ) ) ;
#21479 = CARTESIAN_POINT ( 'NONE',  ( 95.54126587499995082, 83.62500000136560629, -1.846868145590750077 ) ) ;
#21480 = CARTESIAN_POINT ( 'NONE',  ( 51.85481384221820633, 37.62656250108393863, 5.444914386472304635 ) ) ;
#21481 = CARTESIAN_POINT ( 'NONE',  ( 108.0825317500000011, 112.6261737610028320, -52.02500000273118985 ) ) ;
#21482 = CARTESIAN_POINT ( 'NONE',  ( 5.444914386472302859, 40.00781250108393294, 13.14518615778179189 ) ) ;
#21483 = CARTESIAN_POINT ( 'NONE',  ( 100.8561741729129153, 122.7000000010924623, -2.066987299999999195 ) ) ;
#21484 = CARTESIAN_POINT ( 'NONE',  ( 101.9991671059954683, 123.0000000000000142, 1.536366799937288974 ) ) ;
#21485 = CARTESIAN_POINT ( 'NONE',  ( 107.0000000000000000, 107.7255621263696668, -53.59999999453763309 ) ) ;
#21486 = CARTESIAN_POINT ( 'NONE',  ( 120.4011555911795455, 39.51171874999999289, 9.598844408820459861 ) ) ;
#21487 = VERTEX_POINT ( 'NONE', #18730 ) ;
#21488 = CARTESIAN_POINT ( 'NONE',  ( 94.33688103937535629, 105.8855032339526758, -56.29999999453763593 ) ) ;
#21489 = CARTESIAN_POINT ( 'NONE',  ( -9.295050272127046043, 39.06523437608392868, -9.295050272127046043 ) ) ;
#21490 = CARTESIAN_POINT ( 'NONE',  ( 104.4587341249999781, 80.00000000136559208, -1.846868145590750299 ) ) ;
#21491 = CARTESIAN_POINT ( 'NONE',  ( 139.2950502721270425, 36.88242187608393152, 9.295050272127046043 ) ) ;
#21492 = CARTESIAN_POINT ( 'NONE',  ( 74.59884440882045453, 38.22187500216787015, 9.598844408820456309 ) ) ;
#21493 = CARTESIAN_POINT ( 'NONE',  ( 93.46109445667489979, 105.2492070361643215, -51.42499999726882010 ) ) ;
#21494 = CARTESIAN_POINT ( 'NONE',  ( -13.57481594606304753, 37.08085937716786873, -5.622872871577873077 ) ) ;
#21495 = CARTESIAN_POINT ( 'NONE',  ( 103.5355339059327093, -3.535533905932726206, 3.374999999999999556 ) ) ;
#21496 = EDGE_LOOP ( 'NONE', ( #19283, #13077, #3377, #18935 ) ) ;
#21497 = ADVANCED_FACE ( 'NONE', ( #14843 ), #12561, .F. ) ;
#21498 = CARTESIAN_POINT ( 'NONE',  ( 185.7049497278729575, 37.47773437608393010, 9.295050272127047819 ) ) ;
#21499 = CYLINDRICAL_SURFACE ( 'NONE', #3307, 7.000000000000006217 ) ;
#21500 = VECTOR ( 'NONE', #7330, 1000.000000000000000 ) ;
#21501 = CARTESIAN_POINT ( 'NONE',  ( 124.5550856135277087, 38.81718750108393579, -13.14518615778179722 ) ) ;
#21502 = CARTESIAN_POINT ( 'NONE',  ( 9.598844408820459861, 35.74140624999999716, 9.598844408820456309 ) ) ;
#21503 =( BOUNDED_CURVE ( )  B_SPLINE_CURVE ( 2, ( #9271, #26676, #24101, #7268, #2592, #15387, #4579, #22254, #17967 ),
 .UNSPECIFIED., .F., .F. ) 
 B_SPLINE_CURVE_WITH_KNOTS ( ( 3, 2, 2, 2, 3 ),
 ( 0.3500000000000003109, 0.3750000000000003331, 0.4000000000000003553, 0.4250000000000003775, 0.4500000000000003997 ),
 .UNSPECIFIED. ) 
 CURVE ( )  GEOMETRIC_REPRESENTATION_ITEM ( )  RATIONAL_B_SPLINE_CURVE ( ( 0.9999999999999990008, 0.9238795325112877377, 1.000000000000000000, 0.9238795325112867385, 1.000000000000000000, 0.9238795325112867385, 1.000000000000000000, 0.9238795325112855172, 1.000000000000001110 ) ) 
 REPRESENTATION_ITEM ( '' )  );
#21504 = CARTESIAN_POINT ( 'NONE',  ( 96.46446609406721961, 3.535533905932755072, 5.000000002731185944 ) ) ;
#21505 = CARTESIAN_POINT ( 'NONE',  ( 96.84719886470463734, 93.93749999863440792, 3.152801135295351997 ) ) ;
#21506 = CARTESIAN_POINT ( 'NONE',  ( 97.83688103937537051, 103.3426043859339103, -48.60000000000000853 ) ) ;
#21507 = CARTESIAN_POINT ( 'NONE',  ( 13.14518615778179900, 37.13046875108393863, 5.444914386472293977 ) ) ;
#21508 = CARTESIAN_POINT ( 'NONE',  ( -13.14518615778179189, 38.22187500108393010, 5.444914386472304635 ) ) ;
#21509 = ADVANCED_FACE ( 'NONE', ( #25425 ), #8029, .F. ) ;
#21510 = CARTESIAN_POINT ( 'NONE',  ( 195.0000000000000000, 36.43593749999999432, 13.57481594606304576 ) ) ;
#21511 = CARTESIAN_POINT ( 'NONE',  ( 104.9952793366501709, 116.8754121666685393, -48.07500000273119412 ) ) ;
#21512 = CARTESIAN_POINT ( 'NONE',  ( 104.4587341249999781, 1.846868145590750299, 2.250000001365591640 ) ) ;
#21513 = CARTESIAN_POINT ( 'NONE',  ( 55.70494972787295751, 39.85898437608393152, 9.295050272127047819 ) ) ;
#21514 = EDGE_CURVE ( 'NONE', #34, #2000, #8885, .T. ) ;
#21515 = CARTESIAN_POINT ( 'NONE',  ( 101.8468681455907046, -4.458734124999987891, 5.750000001365591196 ) ) ;
#21516 = DIRECTION ( 'NONE',  ( 0.000000000000000000, -1.000000000000000000, 0.000000000000000000 ) ) ;
#21517 = CARTESIAN_POINT ( 'NONE',  ( 104.4587341249999781, 95.31249999863440792, -6.938893903907228378E-15 ) ) ;
#21518 = CARTESIAN_POINT ( 'NONE',  ( -5.569058551902509535, 36.00000000000000000, 11.91493531101285619 ) ) ;
#21519 = CARTESIAN_POINT ( 'NONE',  ( 5.622872871577878406, 39.66054687500000142, 13.57481594606304576 ) ) ;
#21520 = CARTESIAN_POINT ( 'NONE',  ( 116.8548138422182205, 40.75195312608393294, 0.000000000000000000 ) ) ;
#21521 = ORIENTED_EDGE ( 'NONE', *, *, #26203, .F. ) ;
#21522 = CARTESIAN_POINT ( 'NONE',  ( 97.92893218813451028, 84.18750000000000000, 4.999999999999989342 ) ) ;
#21523 = CARTESIAN_POINT ( 'NONE',  ( 98.15313185440925281, 91.99999999863439371, 4.458734124999979898 ) ) ;
#21524 = EDGE_LOOP ( 'NONE', ( #8040, #24194, #4521, #16948 ) ) ;
#21525 = VECTOR ( 'NONE', #15858, 1000.000000000000000 ) ;
#21526 = EDGE_CURVE ( 'NONE', #467, #16116, #3987, .T. ) ;
#21527 = LINE ( 'NONE', #7612, #3858 ) ;
#21528 = CARTESIAN_POINT ( 'NONE',  ( 51.85481384221819923, 35.93984375108393436, -5.444914386472297529 ) ) ;
#21529 = APPLICATION_CONTEXT ( 'automotive_design' ) ;
#21530 = VERTEX_POINT ( 'NONE', #5630 ) ;
#21531 = CARTESIAN_POINT ( 'NONE',  ( -8.312177448680279460E-16, 32.86406249999999574, -13.57481594606304576 ) ) ;
#21532 = CARTESIAN_POINT ( 'NONE',  ( 104.4587341249999639, 1.442382525525748735E-14, 1.187500001365592750 ) ) ;
#21533 = ORIENTED_EDGE ( 'NONE', *, *, #15375, .F. ) ;
#21534 = CARTESIAN_POINT ( 'NONE',  ( -13.14518615778179544, 35.99464330212367003, 0.5696516875508460531 ) ) ;
#21535 = CARTESIAN_POINT ( 'NONE',  ( 2.414731522848535132E-15, 38.56914062608393579, 13.14518615778179544 ) ) ;
#21536 = CARTESIAN_POINT ( 'NONE',  ( 185.4011555911795313, 36.23750000216787726, -9.598844408820458085 ) ) ;
#21537 = CARTESIAN_POINT ( 'NONE',  ( -9.295050272127044266, 36.68398437608392726, 9.295050272127047819 ) ) ;
#21538 = CARTESIAN_POINT ( 'NONE',  ( 130.0000000000000000, -7.395377635281828788, -1.503427012513233026E-14 ) ) ;
#21539 = CARTESIAN_POINT ( 'NONE',  ( 99.99999999999998579, 102.6397644303321215, -51.50000000000000711 ) ) ;
#21540 = EDGE_CURVE ( 'NONE', #27745, #7831, #14295, .T. ) ;
#21541 = CARTESIAN_POINT ( 'NONE',  ( 116.8548138422182205, 40.00781250108393294, 5.444914386472304635 ) ) ;
#21542 = ORIENTED_EDGE ( 'NONE', *, *, #294, .F. ) ;
#21543 = CARTESIAN_POINT ( 'NONE',  ( 13.14518615778179544, 39.56132812608393579, -1.609821015232357215E-15 ) ) ;
#21544 = CARTESIAN_POINT ( 'NONE',  ( 135.4449143864723055, 34.45156250108393436, 13.14518615778179189 ) ) ;
#21545 = CARTESIAN_POINT ( 'NONE',  ( 59.37712712842213136, 37.97382812499999716, 13.57481594606304753 ) ) ;
#21546 = CYLINDRICAL_SURFACE ( 'NONE', #11392, 13.57481594606304576 ) ;
#21547 = AXIS2_PLACEMENT_3D ( 'NONE', #23568, #12564, #7895 ) ;
#21548 = EDGE_CURVE ( 'NONE', #19008, #1080, #9994, .T. ) ;
#21549 = CARTESIAN_POINT ( 'NONE',  ( 99.99999999999995737, 4.458734125000016313, 14.43750000136559208 ) ) ;
#21550 = LINE ( 'NONE', #2024, #25797 ) ;
#21552 = EDGE_CURVE ( 'NONE', #22369, #19690, #21466, .T. ) ;
#21551 = CARTESIAN_POINT ( 'NONE',  ( 98.15313185440925281, 4.458734125000016313, 4.250000001365592084 ) ) ;
#21553 = CARTESIAN_POINT ( 'NONE',  ( 108.0825317500000011, 112.6261737610028320, -52.02500000273118985 ) ) ;
#21554 = DIRECTION ( 'NONE',  ( 0.000000000000000000, 0.000000000000000000, -1.000000000000000000 ) ) ;
#21555 = CARTESIAN_POINT ( 'NONE',  ( 95.54126587499996504, 80.75000000136560629, 1.846868145590724986 ) ) ;
#21556 = CARTESIAN_POINT ( 'NONE',  ( -9.295050272127046043, 34.10429687608393579, -9.295050272127046043 ) ) ;
#21557 = CARTESIAN_POINT ( 'NONE',  ( -13.14518615778179189, 40.00781250108393294, 5.444914386472304635 ) ) ;
#21558 = EDGE_CURVE ( 'NONE', #8379, #11095, #15553, .T. ) ;
#21559 = CARTESIAN_POINT ( 'NONE',  ( 108.0825317499999869, 112.6261737610028320, -46.77499999726882152 ) ) ;
#21560 = ORIENTED_EDGE ( 'NONE', *, *, #6927, .T. ) ;
#21561 = CARTESIAN_POINT ( 'NONE',  ( -9.295050272127046043, 32.71523437608393436, -9.295050272127046043 ) ) ;
#21562 = CARTESIAN_POINT ( 'NONE',  ( 94.99999999999998579, 110.0000000000000000, 15.00099999999999412 ) ) ;
#21563 = CARTESIAN_POINT ( 'NONE',  ( 104.9999999999999716, 1.449011120738813565E-14, 5.500000000000000000 ) ) ;
#21564 = CYLINDRICAL_SURFACE ( 'NONE', #14749, 7.000000000000006217 ) ;
#21565 = CARTESIAN_POINT ( 'NONE',  ( 204.2950502721270425, 38.46992187608393010, 9.295050272127046043 ) ) ;
#21566 = ORIENTED_EDGE ( 'NONE', *, *, #8099, .T. ) ;
#21567 = DIRECTION ( 'NONE',  ( -0.000000000000000000, 1.000000000000000000, -0.000000000000000000 ) ) ;
#21568 = CARTESIAN_POINT ( 'NONE',  ( 99.99999999999995737, 83.37500000273119838, 4.999999999999990230 ) ) ;
#21569 = CARTESIAN_POINT ( 'NONE',  ( 63.11247127412359958, 53.66306546785491349, -14.99999999999999822 ) ) ;
#21570 = AXIS2_PLACEMENT_3D ( 'NONE', #15198, #6521, #26343 ) ;
#21571 = ORIENTED_EDGE ( 'NONE', *, *, #24954, .F. ) ;
#21572 = CARTESIAN_POINT ( 'NONE',  ( 97.83688103937537051, 103.3426043859339103, -47.60000000000000142 ) ) ;
#21573 = CARTESIAN_POINT ( 'NONE',  ( 9.295050272127047819, 40.05742187608392868, 9.295050272127046043 ) ) ;
#21574 = CARTESIAN_POINT ( 'NONE',  ( 98.53841926354351699, 123.2500000010924737, 1.461580736456455920 ) ) ;
#21575 = CARTESIAN_POINT ( 'NONE',  ( 139.5988444088204403, 33.65781250216787157, -9.598844408820458085 ) ) ;
#21576 = CARTESIAN_POINT ( 'NONE',  ( 65.00000000000000000, 39.75976562608394005, -13.14518615778179544 ) ) ;
#21577 = CYLINDRICAL_SURFACE ( 'NONE', #20550, 7.000000000000006217 ) ;
#21578 = CARTESIAN_POINT ( 'NONE',  ( 195.0000000000000000, 34.60039062608393579, 13.14518615778179544 ) ) ;
#21579 = VERTEX_POINT ( 'NONE', #4180 ) ;
#21580 = ORIENTED_EDGE ( 'NONE', *, *, #9846, .T. ) ;
#21581 = CARTESIAN_POINT ( 'NONE',  ( 13.14518615778179900, 40.40468750108393436, -5.444914386472297529 ) ) ;
#21582 = SURFACE_SIDE_STYLE ('',( #3916 ) ) ;
#21583 = CARTESIAN_POINT ( 'NONE',  ( 99.99999999999995737, -4.458734124999988779, 10.93750000136559208 ) ) ;
#21584 = CARTESIAN_POINT ( 'NONE',  ( 13.57481594606304576, 38.22187499999999716, -1.662435489736055892E-15 ) ) ;
#21585 = CARTESIAN_POINT ( 'NONE',  ( 101.8468681455907046, 82.12500000136560629, -4.458734125000016313 ) ) ;
#21586 = CARTESIAN_POINT ( 'NONE',  ( 181.8548138422182205, 37.42812500108393436, 5.444914386472304635 ) ) ;
#21587 = CARTESIAN_POINT ( 'NONE',  ( 102.1829110464049535, 123.0000000000000284, 1.262593708336817500 ) ) ;
#21588 = PLANE ( 'NONE',  #6823 ) ;
#21589 = FACE_OUTER_BOUND ( 'NONE', #5733, .T. ) ;
#21590 = CARTESIAN_POINT ( 'NONE',  ( 195.0000000000000000, 40.55351562608393579, -13.14518615778179544 ) ) ;
#21591 = CARTESIAN_POINT ( 'NONE',  ( 93.46109445667489979, 114.7507929638356785, -51.82499999726881867 ) ) ;
#21592 = ORIENTED_EDGE ( 'NONE', *, *, #27304, .F. ) ;
#21593 = AXIS2_PLACEMENT_3D ( 'NONE', #24396, #2877, #18414 ) ;
#21594 = CARTESIAN_POINT ( 'NONE',  ( -13.57481594606304576, 35.44374999999999432, 0.000000000000000000 ) ) ;
#21595 = CARTESIAN_POINT ( 'NONE',  ( -9.295050272127046043, 37.27929687608393294, -9.295050272127046043 ) ) ;
#21596 = CARTESIAN_POINT ( 'NONE',  ( 95.54126587499996504, 1.387778780781445676E-14, 14.43750000136559208 ) ) ;
#21597 = CARTESIAN_POINT ( 'NONE',  ( 120.7049497278729575, 37.47773437608393010, -9.295050272127046043 ) ) ;
#21598 = CARTESIAN_POINT ( 'NONE',  ( 78.14518615778179367, 33.80664062608393294, -1.609821015232357215E-15 ) ) ;
#21599 = CARTESIAN_POINT ( 'NONE',  ( 204.2950502721270425, 37.27929687608394005, -9.295050272127046043 ) ) ;
#21600 = CARTESIAN_POINT ( 'NONE',  ( 104.9999999999999716, 1.449011120738813565E-14, 13.62500000273118417 ) ) ;
#21601 = CARTESIAN_POINT ( 'NONE',  ( -13.14518615778179544, 36.58476562608393579, 0.000000000000000000 ) ) ;
#21602 = CARTESIAN_POINT ( 'NONE',  ( 138.2685973283865621, 50.00000000054347993, -10.78867689284392561 ) ) ;
#21603 = FACE_OUTER_BOUND ( 'NONE', #12523, .T. ) ;
#21604 = CARTESIAN_POINT ( 'NONE',  ( 5.444914386472302859, 33.85625000108393579, 13.14518615778179189 ) ) ;
#21605 = CARTESIAN_POINT ( 'NONE',  ( 98.96446609406724804, 124.8499999999999943, -2.500000000000008438 ) ) ;
#21606 = CARTESIAN_POINT ( 'NONE',  ( 5.444914386472302859, 38.42031250108393436, 13.14518615778179189 ) ) ;
#21607 = CARTESIAN_POINT ( 'NONE',  ( 97.92893218813451028, 5.000000000000018652, 10.81250000000000000 ) ) ;
#21608 = CARTESIAN_POINT ( 'NONE',  ( 101.7677669529663547, 124.0000000021849615, -1.767766952966370209 ) ) ;
#21609 = CARTESIAN_POINT ( 'NONE',  ( 98.23223304703363112, 124.2999999999999972, 1.767766952966351557 ) ) ;
#21610 = AXIS2_PLACEMENT_3D ( 'NONE', #12563, #23014, #3345 ) ;
#21611 = ORIENTED_EDGE ( 'NONE', *, *, #25541, .T. ) ;
#21612 = CARTESIAN_POINT ( 'NONE',  ( 95.54126587499995082, -1.846868145590724986, 8.500000001365592084 ) ) ;
#21613 = CARTESIAN_POINT ( 'NONE',  ( 71.83113445730414526, 36.00000000000000000, 11.35217666746037679 ) ) ;
#21614 = ORIENTED_EDGE ( 'NONE', *, *, #12329, .F. ) ;
#21615 = PLANE ( 'NONE',  #11148 ) ;
#21616 = CARTESIAN_POINT ( 'NONE',  ( 103.1528011352953342, 3.152801135295383084, 10.06250000136559208 ) ) ;
#21617 = CARTESIAN_POINT ( 'NONE',  ( 123.0976214262113047, 51.13402819306929814, 14.99999999999867661 ) ) ;
#21618 = CARTESIAN_POINT ( 'NONE',  ( -8.049105076161786076E-16, 37.97382812608393721, -13.14518615778179544 ) ) ;
#21619 = FACE_OUTER_BOUND ( 'NONE', #19046, .T. ) ;
#21620 = CARTESIAN_POINT ( 'NONE',  ( 103.1528011352953342, 83.06250000136560629, 3.152801135295355106 ) ) ;
#21621 = CARTESIAN_POINT ( 'NONE',  ( 51.85481384221820633, 34.40195312608393152, 0.000000000000000000 ) ) ;
#21622 = CARTESIAN_POINT ( 'NONE',  ( 108.0825317500000011, 107.3738262389971538, -52.22500000273118559 ) ) ;
#21623 = CARTESIAN_POINT ( 'NONE',  ( 94.99999999999994316, 2.071067811865481278, 11.93750000000000000 ) ) ;
#21624 =( BOUNDED_CURVE ( )  B_SPLINE_CURVE ( 2, ( #24887, #14176, #24744, #13746, #7484, #26895, #20328, #5366, #9765 ),
 .UNSPECIFIED., .F., .T. ) 
 B_SPLINE_CURVE_WITH_KNOTS ( ( 3, 2, 2, 2, 3 ),
 ( 0.6785714285714284921, 0.6874999999999998890, 0.6964285714285712858, 0.7053571428571427937, 0.7142857142857141906 ),
 .UNSPECIFIED. ) 
 CURVE ( )  GEOMETRIC_REPRESENTATION_ITEM ( )  RATIONAL_B_SPLINE_CURVE ( ( 1.000000000000000888, 0.9238795325112857393, 1.000000000000000000, 0.9238795325112867385, 1.000000000000000000, 0.9238795325112867385, 1.000000000000000000, 0.9238795325112877377, 0.9999999999999990008 ) ) 
 REPRESENTATION_ITEM ( '' )  );
#21625 = ORIENTED_EDGE ( 'NONE', *, *, #27599, .T. ) ;
#21626 = CARTESIAN_POINT ( 'NONE',  ( 219.9999999999999716, 80.00000000000000000, 14.99999999999994316 ) ) ;
#21627 = LINE ( 'NONE', #24319, #14940 ) ;
#21628 = CARTESIAN_POINT ( 'NONE',  ( 95.67376207875072680, 115.9545556584642867, -49.30000000000000426 ) ) ;
#21629 = CARTESIAN_POINT ( 'NONE',  ( 143.5748159460630688, 39.80937499999999574, -1.662435489736055892E-15 ) ) ;
#21630 = ORIENTED_EDGE ( 'NONE', *, *, #5170, .T. ) ;
#21631 = LINE ( 'NONE', #4383, #6289 ) ;
#21632 = CARTESIAN_POINT ( 'NONE',  ( 13.14518615778179544, 37.18007812608393436, -1.609821015232357215E-15 ) ) ;
#21633 = CARTESIAN_POINT ( 'NONE',  ( -9.598844408820458085, 38.61875000216787157, -9.598844408820458085 ) ) ;
#21634 = CARTESIAN_POINT ( 'NONE',  ( 130.0000000000000000, 35.19570312608392726, 13.14518615778179544 ) ) ;
#21635 = CARTESIAN_POINT ( 'NONE',  ( 78.57481594606304043, 32.71523437716787441, 5.622872871577869525 ) ) ;
#21636 = PRODUCT_DEFINITION ( 'UNKNOWN', '', #386, #23178 ) ;
#21637 = ADVANCED_FACE ( 'NONE', ( #10713 ), #6311, .F. ) ;
#21638 = VECTOR ( 'NONE', #24343, 1000.000000000000000 ) ;
#21639 = CARTESIAN_POINT ( 'NONE',  ( 13.45411265623090280, 36.00000000000000000, 0.6772748633549623420 ) ) ;
#21640 = CARTESIAN_POINT ( 'NONE',  ( -5.622872871577873077, 36.98164062716787015, -13.57481594606304753 ) ) ;
#21641 = CARTESIAN_POINT ( 'NONE',  ( 103.5355339059327093, -3.535533905932726206, 4.374999999999999112 ) ) ;
#21642 = ORIENTED_EDGE ( 'NONE', *, *, #4427, .T. ) ;
#21643 = CARTESIAN_POINT ( 'NONE',  ( 208.1451861577817795, 37.72578125108393721, 5.444914386472293977 ) ) ;
#21644 = VECTOR ( 'NONE', #7263, 999.9999999999998863 ) ;
#21645 = CIRCLE ( 'NONE', #21195, 3.000000000000004441 ) ;
#21646 = DIRECTION ( 'NONE',  ( -1.000000000000000000, -0.000000000000000000, 2.385244779468110248E-16 ) ) ;
#21647 = SURFACE_STYLE_FILL_AREA ( #17785 ) ;
#21648 = DIRECTION ( 'NONE',  ( -0.000000000000000000, 1.000000000000000000, -0.000000000000000000 ) ) ;
#21649 = CARTESIAN_POINT ( 'NONE',  ( 103.5355339059327093, 3.535533905932755072, 4.750000002731185944 ) ) ;
#21650 = CARTESIAN_POINT ( 'NONE',  ( 13.57481594606304753, 36.68398437499999432, -5.622872871577873077 ) ) ;
#21651 = CARTESIAN_POINT ( 'NONE',  ( 94.99999999999995737, -2.071067811865466624, 12.18750000273118950 ) ) ;
#21652 = CARTESIAN_POINT ( 'NONE',  ( -5.444914386472299306, 36.13828125108393863, 13.14518615778179722 ) ) ;
#21653 = CARTESIAN_POINT ( 'NONE',  ( 5.444914386472297529, 40.30546875108393579, -13.14518615778179900 ) ) ;
#21654 = CARTESIAN_POINT ( 'NONE',  ( 181.4251840539369596, 33.85624999999999574, 0.000000000000000000 ) ) ;
#21655 = CARTESIAN_POINT ( 'NONE',  ( 91.91746824999999887, 110.0000000000000000, -47.37500000273119838 ) ) ;
#21656 = LINE ( 'NONE', #2132, #19243 ) ;
#21657 = CARTESIAN_POINT ( 'NONE',  ( 65.00000000000000000, 37.18007812608393436, -13.14518615778179544 ) ) ;
#21658 = CARTESIAN_POINT ( 'NONE',  ( 96.84719886470459471, -3.152801135295355994, 0.5625000013655921949 ) ) ;
#21659 = CARTESIAN_POINT ( 'NONE',  ( 107.0000000000000142, 107.7255621263696526, -45.60000000546237686 ) ) ;
#21660 = CARTESIAN_POINT ( 'NONE',  ( 98.15313185440925281, 91.62499999863440792, -4.458734124999994997 ) ) ;
#21661 = CARTESIAN_POINT ( 'NONE',  ( 101.7677669529663547, 123.8999999999999915, -1.767766952966370209 ) ) ;
#21662 = CARTESIAN_POINT ( 'NONE',  ( -8.312177448680279460E-16, 36.03906250000000000, -13.57481594606304576 ) ) ;
#21663 = CARTESIAN_POINT ( 'NONE',  ( 94.33688103937537051, 105.8855032339526758, -45.80000000000000426 ) ) ;
#21664 = B_SPLINE_CURVE_WITH_KNOTS ( 'NONE', 3,
 ( #1512, #23443, #12579, #10454 ),
 .UNSPECIFIED., .F., .F.,
 ( 4, 4 ),
 ( 0.000000000000000000, 1.000000000000000000 ),
 .UNSPECIFIED. ) ;
#21665 = ORIENTED_EDGE ( 'NONE', *, *, #15218, .T. ) ;
#21666 = CARTESIAN_POINT ( 'NONE',  ( 95.54126587499995082, 79.75000000136560629, 1.846868145590724986 ) ) ;
#21667 = VECTOR ( 'NONE', #25685, 1000.000000000000000 ) ;
#21668 = CARTESIAN_POINT ( 'NONE',  ( 104.9999999999999716, 90.06249999999998579, -2.071067811865478170 ) ) ;
#21669 = ORIENTED_EDGE ( 'NONE', *, *, #27136, .F. ) ;
#21670 = CARTESIAN_POINT ( 'NONE',  ( 92.99999999999998579, 110.0000000000000000, -49.00000000000001421 ) ) ;
#21671 = CARTESIAN_POINT ( 'NONE',  ( 78.14518615778179367, 36.38632812608393863, -1.609821015232357215E-15 ) ) ;
#21672 = ORIENTED_EDGE ( 'NONE', *, *, #2520, .F. ) ;
#21673 = ADVANCED_FACE ( 'NONE', ( #4597 ), #11793, .F. ) ;
#21674 = CARTESIAN_POINT ( 'NONE',  ( -13.57481594606304753, 33.11210937716787583, -5.622872871577872189 ) ) ;
#21675 = CARTESIAN_POINT ( 'NONE',  ( 95.54126587499995082, -1.846868145590724986, 4.750000001365592084 ) ) ;
#21676 = EDGE_CURVE ( 'NONE', #1287, #24831, #255, .T. ) ;
#21677 = ORIENTED_EDGE ( 'NONE', *, *, #7569, .T. ) ;
#21678 = CARTESIAN_POINT ( 'NONE',  ( -13.14518615778179722, 34.35234375108393579, -5.444914386472297529 ) ) ;
#21679 =( BOUNDED_SURFACE ( )  B_SPLINE_SURFACE ( 1, 2, ( 
 ( #19659, #15515, #2569, #2289, #19948, #13657, #573, #13219, #16986, #17658, #426, #10428, #12701, #8970, #22233, #26219, #22372, #19136, #26365, #24223, #8827, #10948, #2712, #17946, #21951, #9254, #6825, #11231, #4036, #25686, #26657, #4703, #11373, #141, #7104, #17517, #2429, #23559, #20095, #21813, #15802, #13364, #22092, #4849, #9112, #24506, #27842, #17807, #15661, #6169, #4993, #15365, #26510, #6679, #11090, #24081, #4557, #6966, #24361, #19801, #8298, #14836, #284, #13513, #13936, #3274, #13794, #2845, #24789, #15938, #9390, #22663, #27083, #1282, #11802, #20379, #1007, #5417, #2982, #16373, #5697 ),
 ( #12078, #16517, #26945, #7681, #24654, #18086, #3133, #715, #25074, #26798, #18378, #18662, #5562, #1149, #20802, #14225, #20526, #9948, #7247, #5271, #14364, #11514, #22517, #9676, #5127, #7536, #20232, #11656, #864, #27366, #9537, #18236, #7824, #16233, #7388, #16081, #24931, #9816, #14086, #22806, #22946, #11943, #20665, #18522, #27228, #3407, #25209, #16790, #3695, #10639, #18928, #23491, #3971, #14636, #27773, #27910, #23354, #8372, #12488, #1565, #12631, #1699, #28049, #19065, #27636, #19346, #12358, #14911, #25906, #25350, #12773, #21490, #10356, #1971, #21076, #1423, #6376, #8231, #23631, #8516, #10217 ) ),
 .UNSPECIFIED., .F., .F., .F. ) 
 B_SPLINE_SURFACE_WITH_KNOTS ( ( 2, 2 ),
 ( 3, 2, 2, 2, 2, 2, 2, 2, 2, 2, 2, 2, 2, 2, 2, 2, 2, 2, 2, 2, 2, 2, 2, 2, 2, 2, 2, 2, 2, 2, 2, 2, 2, 2, 2, 2, 2, 2, 2, 2, 3 ),
 ( 0.000000000000000000, 1.000000000000000000 ),
 ( 0.000000000000000000, 0.02500000000000000139, 0.05000000000000000278, 0.07499999999999999722, 0.1000000000000000056, 0.1250000000000000000, 0.1499999999999999944, 0.1749999999999999889, 0.2000000000000000111, 0.2250000000000000056, 0.2500000000000000000, 0.2750000000000000222, 0.2999999999999999889, 0.3250000000000000111, 0.3499999999999999778, 0.3750000000000000000, 0.4000000000000000222, 0.4249999999999999889, 0.4500000000000000111, 0.4749999999999999778, 0.5000000000000000000, 0.5250000000000000222, 0.5500000000000000444, 0.5749999999999999556, 0.5999999999999999778, 0.6250000000000000000, 0.6500000000000000222, 0.6750000000000000444, 0.6999999999999999556, 0.7249999999999999778, 0.7500000000000000000, 0.7750000000000000222, 0.8000000000000000444, 0.8249999999999999556, 0.8499999999999999778, 0.8750000000000000000, 0.9000000000000000222, 0.9250000000000000444, 0.9499999999999999556, 0.9749999999999999778, 1.000000000000000000 ),
 .UNSPECIFIED. ) 
 GEOMETRIC_REPRESENTATION_ITEM ( )  RATIONAL_B_SPLINE_SURFACE ( (
 ( 1.000000000000000000, 0.9238795325112867385, 1.000000000000000000, 0.9238795325112867385, 1.000000000000000000, 0.9238795325112867385, 1.000000000000000000, 0.9238795325112867385, 1.000000000000000000, 0.9238795325112867385, 1.000000000000000000, 0.9238795325112867385, 1.000000000000000000, 0.9238795325112867385, 1.000000000000000000, 0.9238795325112867385, 1.000000000000000000, 0.9238795325112867385, 1.000000000000000000, 0.9238795325112867385, 1.000000000000000000, 0.9238795325112867385, 1.000000000000000000, 0.9238795325112867385, 1.000000000000000000, 0.9238795325112867385, 1.000000000000000000, 0.9238795325112867385, 1.000000000000000000, 0.9238795325112867385, 1.000000000000000000, 0.9238795325112867385, 1.000000000000000000, 0.9238795325112867385, 1.000000000000000000, 0.9238795325112867385, 1.000000000000000000, 0.9238795325112867385, 1.000000000000000000, 0.9238795325112867385, 1.000000000000000000, 0.9238795325112867385, 1.000000000000000000, 0.9238795325112867385, 1.000000000000000000, 0.9238795325112867385, 1.000000000000000000, 0.9238795325112867385, 1.000000000000000000, 0.9238795325112867385, 1.000000000000000000, 0.9238795325112867385, 1.000000000000000000, 0.9238795325112867385, 1.000000000000000000, 0.9238795325112867385, 1.000000000000000000, 0.9238795325112867385, 1.000000000000000000, 0.9238795325112867385, 1.000000000000000000, 0.9238795325112867385, 1.000000000000000000, 0.9238795325112867385, 1.000000000000000000, 0.9238795325112867385, 1.000000000000000000, 0.9238795325112867385, 1.000000000000000000, 0.9238795325112867385, 1.000000000000000000, 0.9238795325112867385, 1.000000000000000000, 0.9238795325112867385, 1.000000000000000000, 0.9238795325112867385, 1.000000000000000000, 0.9238795325112867385, 1.000000000000000000, 0.9238795325112867385, 1.000000000000000000),
 ( 1.000000000000000000, 0.9238795325112867385, 1.000000000000000000, 0.9238795325112867385, 1.000000000000000000, 0.9238795325112867385, 1.000000000000000000, 0.9238795325112867385, 1.000000000000000000, 0.9238795325112867385, 1.000000000000000000, 0.9238795325112867385, 1.000000000000000000, 0.9238795325112867385, 1.000000000000000000, 0.9238795325112867385, 1.000000000000000000, 0.9238795325112867385, 1.000000000000000000, 0.9238795325112867385, 1.000000000000000000, 0.9238795325112867385, 1.000000000000000000, 0.9238795325112867385, 1.000000000000000000, 0.9238795325112867385, 1.000000000000000000, 0.9238795325112867385, 1.000000000000000000, 0.9238795325112867385, 1.000000000000000000, 0.9238795325112867385, 1.000000000000000000, 0.9238795325112867385, 1.000000000000000000, 0.9238795325112867385, 1.000000000000000000, 0.9238795325112867385, 1.000000000000000000, 0.9238795325112867385, 1.000000000000000000, 0.9238795325112867385, 1.000000000000000000, 0.9238795325112867385, 1.000000000000000000, 0.9238795325112867385, 1.000000000000000000, 0.9238795325112867385, 1.000000000000000000, 0.9238795325112867385, 1.000000000000000000, 0.9238795325112867385, 1.000000000000000000, 0.9238795325112867385, 1.000000000000000000, 0.9238795325112867385, 1.000000000000000000, 0.9238795325112867385, 1.000000000000000000, 0.9238795325112867385, 1.000000000000000000, 0.9238795325112867385, 1.000000000000000000, 0.9238795325112867385, 1.000000000000000000, 0.9238795325112867385, 1.000000000000000000, 0.9238795325112867385, 1.000000000000000000, 0.9238795325112867385, 1.000000000000000000, 0.9238795325112867385, 1.000000000000000000, 0.9238795325112867385, 1.000000000000000000, 0.9238795325112867385, 1.000000000000000000, 0.9238795325112867385, 1.000000000000000000, 0.9238795325112867385, 1.000000000000000000) ) ) 
 REPRESENTATION_ITEM ( '' )  SURFACE ( )  );
#21680 = CARTESIAN_POINT ( 'NONE',  ( -8.049105076161786076E-16, 38.96601562608393721, -13.14518615778179544 ) ) ;
#21681 = CARTESIAN_POINT ( 'NONE',  ( 195.0000000000000000, 38.51953125216787299, -13.57481594606304576 ) ) ;
#21682 = CARTESIAN_POINT ( 'NONE',  ( 5.444914386472302859, 37.62656250108393152, 13.14518615778179189 ) ) ;
#21683 = FACE_OUTER_BOUND ( 'NONE', #4377, .T. ) ;
#21684 = CARTESIAN_POINT ( 'NONE',  ( 195.3969994146466149, 51.45716825712325004, 14.99999999999927702 ) ) ;
#21685 = CARTESIAN_POINT ( 'NONE',  ( 135.4449143864723339, 36.53515625108394715, -13.14518615778179722 ) ) ;
#21686 = CARTESIAN_POINT ( 'NONE',  ( -13.14518615778179900, 36.73359375108393010, -5.444914386472297529 ) ) ;
#21687 = CARTESIAN_POINT ( 'NONE',  ( 116.8548138422182205, 33.40976562608393863, 0.000000000000000000 ) ) ;
#21688 = CARTESIAN_POINT ( 'NONE',  ( 59.37712712842213136, 33.70742187500000142, -13.57481594606304753 ) ) ;
#21689 = VECTOR ( 'NONE', #24653, 1000.000000000000000 ) ;
#21690 = CARTESIAN_POINT ( 'NONE',  ( 97.71650635000000307, 124.4250000016387219, -9.540979117872439019E-15 ) ) ;
#21691 = EDGE_CURVE ( 'NONE', #26276, #21956, #18205, .T. ) ;
#21692 = CARTESIAN_POINT ( 'NONE',  ( 95.54126587499995082, 1.846868145590750077, 13.62500000136559386 ) ) ;
#21693 = CARTESIAN_POINT ( 'NONE',  ( 114.9999999999999858, 95.00000000000000000, -15.00000000000000711 ) ) ;
#21694 = CARTESIAN_POINT ( 'NONE',  ( 104.4587341249999781, 1.846868145590750521, 13.00000000136559386 ) ) ;
#21695 = CARTESIAN_POINT ( 'NONE',  ( 106.5389055433251002, 114.7507929638356785, -53.92500000273119554 ) ) ;
#21696 = CARTESIAN_POINT ( 'NONE',  ( 101.0355339059327093, 123.6500000000000057, 2.499999999999984457 ) ) ;
#21697 = FACE_OUTER_BOUND ( 'NONE', #6959, .T. ) ;
#21698 = CARTESIAN_POINT ( 'NONE',  ( 95.00472066334981491, 103.1245878333314465, -47.32499999726881867 ) ) ;
#21699 = CARTESIAN_POINT ( 'NONE',  ( 13.14518615778179900, 37.92421875108392726, 5.444914386472293977 ) ) ;
#21700 = CARTESIAN_POINT ( 'NONE',  ( 91.91746824999997045, 112.6261737610028320, -45.97499999726882436 ) ) ;
#21701 = ORIENTED_EDGE ( 'NONE', *, *, #26904, .F. ) ;
#21702 = CARTESIAN_POINT ( 'NONE',  ( 100.8561741729129437, 124.2000000010924623, 2.066987299999979655 ) ) ;
#21703 = AXIS2_PLACEMENT_3D ( 'NONE', #563, #18227, #24781 ) ;
#21704 = CARTESIAN_POINT ( 'NONE',  ( 116.4251840539369738, 37.18007812716787441, 5.622872871577880183 ) ) ;
#21705 = CARTESIAN_POINT ( 'NONE',  ( 185.4011555911795313, 36.13828124999999147, -9.598844408820458085 ) ) ;
#21706 = EDGE_CURVE ( 'NONE', #2910, #2056, #22384, .T. ) ;
#21707 = CARTESIAN_POINT ( 'NONE',  ( 195.0000000000000000, 37.57695312608392868, 13.14518615778179544 ) ) ;
#21708 = AXIS2_PLACEMENT_3D ( 'NONE', #11957, #16387, #16931 ) ;
#21709 = ORIENTED_EDGE ( 'NONE', *, *, #24980, .T. ) ;
#21710 = CARTESIAN_POINT ( 'NONE',  ( 94.99999999999995737, 1.387778780781445676E-14, 7.125000002731185056 ) ) ;
#21711 = CARTESIAN_POINT ( 'NONE',  ( 96.46446609406721961, 83.25000000273119838, 3.535533905932727539 ) ) ;
#21712 = CIRCLE ( 'NONE', #17134, 4.999999999999999112 ) ;
#21713 = CARTESIAN_POINT ( 'NONE',  ( 95.54126587499995082, -1.846868145590724986, 13.75000000136559208 ) ) ;
#21714 = ORIENTED_EDGE ( 'NONE', *, *, #19063, .T. ) ;
#21715 = CARTESIAN_POINT ( 'NONE',  ( 104.3262379212492590, 104.0454443415356991, -53.29999999999999716 ) ) ;
#21716 = CARTESIAN_POINT ( 'NONE',  ( -13.14518615778179189, 38.22187500108393010, 5.444914386472304635 ) ) ;
#21717 = CARTESIAN_POINT ( 'NONE',  ( 100.8561741729129153, 123.7000000010924765, -2.066987299999999195 ) ) ;
#21718 = EDGE_CURVE ( 'NONE', #18166, #25525, #17130, .T. ) ;
#21719 = CARTESIAN_POINT ( 'NONE',  ( 143.1451861577818079, 40.20625000108393010, -5.444914386472297529 ) ) ;
#21720 = DIRECTION ( 'NONE',  ( 1.000000000000000000, 0.000000000000000000, -0.000000000000000000 ) ) ;
#21721 = CARTESIAN_POINT ( 'NONE',  ( 95.00000000000000000, 92.37499999726880162, -7.551217303480904118E-15 ) ) ;
#21722 = VECTOR ( 'NONE', #1207, 1000.000000000000000 ) ;
#21723 = CARTESIAN_POINT ( 'NONE',  ( 65.00000000000000000, 40.15664062608393436, 13.14518615778179544 ) ) ;
#21724 = CYLINDRICAL_SURFACE ( 'NONE', #20093, 2.500000000000008882 ) ;
#21725 = CARTESIAN_POINT ( 'NONE',  ( 208.1451861577817795, 34.05468750108394005, -5.444914386472297529 ) ) ;
#21726 = ORIENTED_EDGE ( 'NONE', *, *, #26948, .F. ) ;
#21727 = ORIENTED_EDGE ( 'NONE', *, *, #21676, .F. ) ;
#21728 = ORIENTED_EDGE ( 'NONE', *, *, #24502, .F. ) ;
#21729 = CARTESIAN_POINT ( 'NONE',  ( -13.14518615778179544, 39.16445312608393436, 0.000000000000000000 ) ) ;
#21730 = CARTESIAN_POINT ( 'NONE',  ( 98.15313185440923860, -4.458734124999987891, 9.875000001365593860 ) ) ;
#21731 = CARTESIAN_POINT ( 'NONE',  ( 2.493653234604083739E-15, 38.02343749999999289, 13.57481594606304576 ) ) ;
#21732 = CARTESIAN_POINT ( 'NONE',  ( 95.54126587499996504, 81.43750000136559208, -1.387778780781445676E-14 ) ) ;
#21733 = CARTESIAN_POINT ( 'NONE',  ( 208.1451861577818079, 37.82500000108392868, -5.444914386472297529 ) ) ;
#21734 = CARTESIAN_POINT ( 'NONE',  ( 9.295050272127047819, 38.66835937608393436, 9.295050272127046043 ) ) ;
#21735 = CARTESIAN_POINT ( 'NONE',  ( 188.0976214262265671, 51.13402819307177793, 14.99999999999995559 ) ) ;
#21736 = DIRECTION ( 'NONE',  ( -0.000000000000000000, -1.000000000000000000, -0.000000000000000000 ) ) ;
#21737 = CARTESIAN_POINT ( 'NONE',  ( 93.00000000000000000, 110.0000000000000000, -50.00000000000000711 ) ) ;
#21738 = CARTESIAN_POINT ( 'NONE',  ( 93.46109445667489979, 105.2492070361643215, -53.42499999726882720 ) ) ;
#21739 = EDGE_LOOP ( 'NONE', ( #610, #357, #19385, #1661 ) ) ;
#21740 = CARTESIAN_POINT ( 'NONE',  ( -13.57481594606304753, 35.39414062499999147, -5.622872871577873077 ) ) ;
#21741 = CARTESIAN_POINT ( 'NONE',  ( -9.295050272127044266, 35.89023437608393152, 9.295050272127047819 ) ) ;
#21742 = CLOSED_SHELL ( 'NONE', ( #2167, #1561, #9467, #13270, #25032, #19180, #7242, #3405, #20700, #13993, #27837, #4190, #11393, #16957, #11549, #1205, #7141, #10856, #23786, #16809, #13596, #13522, #20005, #18729, #16999, #3771, #1983, #6044, #25110, #26160, #25397, #16266, #25725, #22421, #7210, #15973, #7898, #23250, #9470, #6208, #25341, #812, #27471, #6362, #23800, #17662, #4499, #12771, #8439, #12616, #27297, #22152, #14883, #5851, #23279, #10674, #10363, #20772, #20833, #21162, #2107, #22941, #21443, #16231, #22921, #9827, #10549, #793, #21011, #277, #4621, #20501, #19294, #23111, #6861, #7251, #2179, #8633, #3009, #19920, #12764, #20461, #13145, #20475, #8835, #12445, #15504, #22390, #24166, #1357, #10149, #13123, #8625, #26421, #16482, #16391, #15449, #14173, #18044, #22236, #8205, #7737, #14384, #26980, #17828, #15051, #4076, #18740, #19938, #7574, #16305, #2252, #20299, #10401, #12260, #21870, #14857, #2499, #3760, #5515, #22868, #9890, #1666, #10519, #26618, #2144, #8721, #96, #5345, #12245, #26082, #16737, #24141, #2393, #26246, #27331, #9867, #15740, #26585, #11064, #3919, #3044, #27086, #21497, #21399, #17841, #15608, #9480, #24458, #16823, #15336, #8094, #25019, #11025 ) ) ;
#21743 = CARTESIAN_POINT ( 'NONE',  ( 96.84719886470459471, 3.152801135295383084, 14.31250000136559208 ) ) ;
#21744 = CARTESIAN_POINT ( 'NONE',  ( 124.5550856135277087, 36.63437500108393152, -13.14518615778179900 ) ) ;
#21745 = CARTESIAN_POINT ( 'NONE',  ( 78.14518615778179367, 32.16953125108393152, 5.444914386472293977 ) ) ;
#21746 = CARTESIAN_POINT ( 'NONE',  ( 189.5550856135277229, 36.63437500108393152, -13.14518615778179900 ) ) ;
#21747 = DIRECTION ( 'NONE',  ( 0.000000000000000000, 0.000000000000000000, 1.000000000000000000 ) ) ;
#21748 = CARTESIAN_POINT ( 'NONE',  ( -13.14518615778179189, 32.66562500108393863, 5.444914386472304635 ) ) ;
#21749 = CARTESIAN_POINT ( 'NONE',  ( 126.0201855542024418, 50.00000000123280586, -13.01613927313105634 ) ) ;
#21750 = EDGE_CURVE ( 'NONE', #27310, #5488, #16681, .T. ) ;
#21751 = CARTESIAN_POINT ( 'NONE',  ( 94.99999999999995737, 2.071067811865491493, 10.06250000273118417 ) ) ;
#21752 = LINE ( 'NONE', #24022, #5884 ) ;
#21753 = DIRECTION ( 'NONE',  ( 0.000000000000000000, -0.000000000000000000, 1.000000000000000000 ) ) ;
#21754 = CARTESIAN_POINT ( 'NONE',  ( 5.444914386472297529, 34.74921875108394431, -13.14518615778179900 ) ) ;
#21755 = CARTESIAN_POINT ( 'NONE',  ( -13.57481594606304398, 34.69960937499999432, 5.622872871577880183 ) ) ;
#21756 = CARTESIAN_POINT ( 'NONE',  ( 97.50000000000000000, 122.7000000021849502, -9.540979117872439019E-15 ) ) ;
#21757 = CARTESIAN_POINT ( 'NONE',  ( 99.99999999999998579, 110.0000000000000000, -45.00000000000000711 ) ) ;
#21758 = LINE ( 'NONE', #8771, #1790 ) ;
#21759 = CARTESIAN_POINT ( 'NONE',  ( 99.99999999999995737, -4.458734124999988779, 10.68750000136559208 ) ) ;
#21760 = ORIENTED_EDGE ( 'NONE', *, *, #28145, .F. ) ;
#21761 = CARTESIAN_POINT ( 'NONE',  ( 100.8561741729129295, 123.2000000010924765, 2.066987299999979211 ) ) ;
#21762 = CARTESIAN_POINT ( 'NONE',  ( 96.84719886470459471, -3.152801135295355994, 11.56250000136559208 ) ) ;
#21763 = CARTESIAN_POINT ( 'NONE',  ( 130.3969994146466433, 51.45716825712460007, 15.00000000000097522 ) ) ;
#21764 = CARTESIAN_POINT ( 'NONE',  ( 13.14518615778179544, 40.15664062608393436, -1.609821015232357215E-15 ) ) ;
#21765 = CARTESIAN_POINT ( 'NONE',  ( 195.0000000000000000, 36.00000000000000000, -2.255140518769849538E-14 ) ) ;
#21766 = CARTESIAN_POINT ( 'NONE',  ( 95.54126587499995082, 82.62500000136560629, -1.846868145590750077 ) ) ;
#21767 = CARTESIAN_POINT ( 'NONE',  ( 55.70494972787295751, 34.30273437608393294, -9.295050272127046043 ) ) ;
#21768 = CARTESIAN_POINT ( 'NONE',  ( 95.00472066334982912, 103.1245878333314323, -52.82500000273118701 ) ) ;
#21769 = CARTESIAN_POINT ( 'NONE',  ( 2.493653234604083739E-15, 37.22968749999999716, 13.57481594606304576 ) ) ;
#21770 = CARTESIAN_POINT ( 'NONE',  ( 65.00000000000000000, 36.43593749999999432, 13.57481594606304576 ) ) ;
#21771 = LINE ( 'NONE', #2249, #3136 ) ;
#21772 = CARTESIAN_POINT ( 'NONE',  ( 99.99999999999997158, 117.3602355696678643, -54.99999999453763166 ) ) ;
#21773 = CARTESIAN_POINT ( 'NONE',  ( 139.5988444088204403, 35.93984374999999432, -9.598844408820458085 ) ) ;
#21774 = ORIENTED_EDGE ( 'NONE', *, *, #9831, .T. ) ;
#21775 = FACE_OUTER_BOUND ( 'NONE', #8868, .T. ) ;
#21776 = CARTESIAN_POINT ( 'NONE',  ( -9.295050272127044266, 37.67617187608393436, 9.295050272127047819 ) ) ;
#21777 = CARTESIAN_POINT ( 'NONE',  ( 13.57481594606304576, 37.52734375216787299, -1.662435489736055892E-15 ) ) ;
#21778 = CARTESIAN_POINT ( 'NONE',  ( 124.5550856135277087, 37.22968750108393721, -13.14518615778179900 ) ) ;
#21779 = CARTESIAN_POINT ( 'NONE',  ( 55.40115559117954547, 33.85625000216787583, -9.598844408820458085 ) ) ;
#21780 = ORIENTED_EDGE ( 'NONE', *, *, #19238, .T. ) ;
#21781 = CARTESIAN_POINT ( 'NONE',  ( 12.07727640983550188, 36.00000000000000000, -6.197985357349471869 ) ) ;
#21782 = CARTESIAN_POINT ( 'NONE',  ( 3.878385410779738418, 31.34156310770110565, -13.57481594606304931 ) ) ;
#21783 = AXIS2_PLACEMENT_3D ( 'NONE', #26039, #17054, #107 ) ;
#21784 = CARTESIAN_POINT ( 'NONE',  ( 94.99999999999995737, -2.071067811865466624, 7.062499999999999112 ) ) ;
#21785 = CARTESIAN_POINT ( 'NONE',  ( 97.50236033167490746, 102.3130555110000159, -49.47499999726882436 ) ) ;
#21786 = AXIS2_PLACEMENT_3D ( 'NONE', #9699, #26966, #5152 ) ;
#21787 = CARTESIAN_POINT ( 'NONE',  ( 195.0000000000000000, 34.00507812608393721, -13.14518615778179544 ) ) ;
#21788 = CARTESIAN_POINT ( 'NONE',  ( 65.00000000000000000, 38.81718749999999574, 13.57481594606304576 ) ) ;
#21789 = CARTESIAN_POINT ( 'NONE',  ( 98.96446609406726225, 122.8500000021849416, 2.499999999999977796 ) ) ;
#21790 = CARTESIAN_POINT ( 'NONE',  ( 94.99999999999995737, 1.387778780781445676E-14, 9.125000002731184168 ) ) ;
#21791 = CARTESIAN_POINT ( 'NONE',  ( 104.3262379212492448, 104.0454443415356991, -47.79999999453763593 ) ) ;
#21792 = CARTESIAN_POINT ( 'NONE',  ( 13.57481594606304931, 37.37851562499999858, 5.622872871577869525 ) ) ;
#21793 =( BOUNDED_CURVE ( )  B_SPLINE_CURVE ( 2, ( #7451, #7601, #24421, #22861, #9174, #15718, #9592, #17867, #18295 ),
 .UNSPECIFIED., .F., .T. ) 
 B_SPLINE_CURVE_WITH_KNOTS ( ( 3, 2, 2, 2, 3 ),
 ( 0.8928571428571427937, 0.9017857142857141906, 0.9107142857142855874, 0.9196428571428569843, 0.9285714285714284921 ),
 .UNSPECIFIED. ) 
 CURVE ( )  GEOMETRIC_REPRESENTATION_ITEM ( )  RATIONAL_B_SPLINE_CURVE ( ( 1.000000000000000888, 0.9238795325112857393, 1.000000000000000000, 0.9238795325112867385, 1.000000000000000000, 0.9238795325112867385, 1.000000000000000000, 0.9238795325112877377, 0.9999999999999990008 ) ) 
 REPRESENTATION_ITEM ( '' )  );
#21794 = CARTESIAN_POINT ( 'NONE',  ( 4.157286354961724939, 36.00000000000000000, -12.92256159328856135 ) ) ;
#21795 = CARTESIAN_POINT ( 'NONE',  ( -13.14518615778179189, 38.42031250108393436, 5.444914386472304635 ) ) ;
#21796 = CARTESIAN_POINT ( 'NONE',  ( 99.99999999999998579, 123.2000000000000028, -2.499999999999997780 ) ) ;
#21797 = CARTESIAN_POINT ( 'NONE',  ( 204.5988444088204687, 34.15390624999999858, 9.598844408820456309 ) ) ;
#21798 = CARTESIAN_POINT ( 'NONE',  ( 99.99999999999998579, 118.4984768113314146, -47.87500000273119127 ) ) ;
#21799 = CARTESIAN_POINT ( 'NONE',  ( 0.000000000000000000, 40.99999999999999289, 0.000000000000000000 ) ) ;
#21800 = CARTESIAN_POINT ( 'NONE',  ( 65.00000000000000000, 35.59257812608393579, -13.14518615778179544 ) ) ;
#21801 = EDGE_CURVE ( 'NONE', #13724, #5134, #14696, .T. ) ;
#21802 = CARTESIAN_POINT ( 'NONE',  ( 98.15313185440923860, 4.458734125000016313, 2.250000001365592084 ) ) ;
#21803 = DIRECTION ( 'NONE',  ( -0.000000000000000000, 1.000000000000000000, -0.000000000000000000 ) ) ;
#21804 = CARTESIAN_POINT ( 'NONE',  ( 103.1528011352953484, 94.43749999863440792, -3.152801135295366208 ) ) ;
#21805 = CARTESIAN_POINT ( 'NONE',  ( 99.99999999999998579, 124.0000000000000000, -2.499999999999997780 ) ) ;
#21806 = CARTESIAN_POINT ( 'NONE',  ( -13.57481594606304576, 35.49335937499999005, 5.622872871577880183 ) ) ;
#21807 = CARTESIAN_POINT ( 'NONE',  ( 143.1451861577818079, 37.22968750108393721, -5.444914386472297529 ) ) ;
#21808 = VECTOR ( 'NONE', #3631, 1000.000000000000000 ) ;
#21809 = ORIENTED_EDGE ( 'NONE', *, *, #9004, .F. ) ;
#21810 = VERTEX_POINT ( 'NONE', #21049 ) ;
#21811 = CARTESIAN_POINT ( 'NONE',  ( 103.5355339059327093, 83.37500000000000000, 3.535533905932726206 ) ) ;
#21812 = AXIS2_PLACEMENT_3D ( 'NONE', #16806, #12092, #27651 ) ;
#21813 = CARTESIAN_POINT ( 'NONE',  ( 104.9999999999999574, 81.68750000273119838, -2.071067811865491937 ) ) ;
#21814 = CARTESIAN_POINT ( 'NONE',  ( 104.4587341249999923, 93.24999999863439371, 1.846868145590726318 ) ) ;
#21815 = CARTESIAN_POINT ( 'NONE',  ( 103.1528011352953484, 95.43749999863440792, 3.152801135295352886 ) ) ;
#21816 = ORIENTED_EDGE ( 'NONE', *, *, #18034, .F. ) ;
#21817 = CARTESIAN_POINT ( 'NONE',  ( 107.0000000000000000, 112.2744378736303332, -51.90000000000000568 ) ) ;
#21818 = CARTESIAN_POINT ( 'NONE',  ( 70.44491438647230552, 35.44375000108393436, 13.14518615778179189 ) ) ;
#21819 = ORIENTED_EDGE ( 'NONE', *, *, #26777, .F. ) ;
#21820 = CARTESIAN_POINT ( 'NONE',  ( 0.000000000000000000, 1.000000000000000000, 0.000000000000000000 ) ) ;
#21821 = CARTESIAN_POINT ( 'NONE',  ( 103.1528011352953342, -3.152801135295355106, 3.062500001365592528 ) ) ;
#21822 = ORIENTED_EDGE ( 'NONE', *, *, #25461, .F. ) ;
#21823 = CARTESIAN_POINT ( 'NONE',  ( -13.14518615778179189, 34.45156250108394147, 5.444914386472304635 ) ) ;
#21824 = CARTESIAN_POINT ( 'NONE',  ( -13.14518615778179544, 39.16445312608393436, 0.000000000000000000 ) ) ;
#21825 = UNCERTAINTY_MEASURE_WITH_UNIT (LENGTH_MEASURE( 1.000000000000000082E-05 ), #8294, 'distance_accuracy_value', 'NONE');
#21826 = CARTESIAN_POINT ( 'NONE',  ( 208.5748159460630120, 38.27148437716787299, 5.622872871577869525 ) ) ;
#21827 = CARTESIAN_POINT ( 'NONE',  ( 13.14518615778179722, 37.82500000108392868, -5.444914386472297529 ) ) ;
#21828 = DIRECTION ( 'NONE',  ( -0.000000000000000000, -0.000000000000000000, -1.000000000000000000 ) ) ;
#21829 = CARTESIAN_POINT ( 'NONE',  ( 120.7049497278729575, 36.08867187608393579, 9.295050272127047819 ) ) ;
#21830 = CARTESIAN_POINT ( 'NONE',  ( 13.14518615778179544, 37.18007812608393436, -1.609821015232357215E-15 ) ) ;
#21831 = PRESENTATION_LAYER_ASSIGNMENT (  '', '', ( #20468 ) ) ;
#21832 = CARTESIAN_POINT ( 'NONE',  ( 135.4449143864723055, 35.24531250108393010, 13.14518615778179189 ) ) ;
#21833 = CARTESIAN_POINT ( 'NONE',  ( 78.57481594606305464, 35.04687499999999289, -1.662435489736055892E-15 ) ) ;
#21834 = CARTESIAN_POINT ( 'NONE',  ( 51.42518405393695957, 39.51171875216787299, 0.000000000000000000 ) ) ;
#21835 = AXIS2_PLACEMENT_3D ( 'NONE', #23310, #21306, #8325 ) ;
#21836 = CARTESIAN_POINT ( 'NONE',  ( 99.99999999999995737, -4.458734124999988779, 11.93750000136559208 ) ) ;
#21837 = CARTESIAN_POINT ( 'NONE',  ( 0.000000000000000000, 0.000000000000000000, 0.000000000000000000 ) ) ;
#21838 = CARTESIAN_POINT ( 'NONE',  ( 104.4587341249999781, 1.846868145590750521, 14.00000000136559208 ) ) ;
#21839 = CARTESIAN_POINT ( 'NONE',  ( 108.0825317500000153, 110.0000000000000000, -54.12500000273119838 ) ) ;
#21840 = DIRECTION ( 'NONE',  ( -5.782411586589357392E-17, 0.000000000000000000, -1.000000000000000000 ) ) ;
#21841 = CARTESIAN_POINT ( 'NONE',  ( 103.1528011352953342, 81.06250000136559208, 3.152801135295355106 ) ) ;
#21842 = CARTESIAN_POINT ( 'NONE',  ( 99.99999999999997158, 101.5015231886685712, -49.12499999726882294 ) ) ;
#21843 = CARTESIAN_POINT ( 'NONE',  ( -5.444914386472297529, 37.42812500108394147, -13.14518615778179900 ) ) ;
#21844 = CARTESIAN_POINT ( 'NONE',  ( 97.50236033167490746, 117.6869444889999841, -50.27499999726882152 ) ) ;
#21845 = EDGE_LOOP ( 'NONE', ( #462, #22766, #22703, #8976 ) ) ;
#21846 = EDGE_CURVE ( 'NONE', #10395, #22131, #22635, .T. ) ;
#21847 = DIRECTION ( 'NONE',  ( -0.000000000000000000, -1.000000000000000000, -0.000000000000000000 ) ) ;
#21848 = CARTESIAN_POINT ( 'NONE',  ( 100.0000000000000000, 110.0000000000000000, -55.00000000000000711 ) ) ;
#21849 =( BOUNDED_CURVE ( )  B_SPLINE_CURVE ( 2, ( #12612, #21059, #25889, #6358, #18910 ),
 .UNSPECIFIED., .F., .F. ) 
 B_SPLINE_CURVE_WITH_KNOTS ( ( 3, 2, 3 ),
 ( 0.000000000000000000, 0.01041666666666679446, 0.02083333333333358892 ),
 .UNSPECIFIED. ) 
 CURVE ( )  GEOMETRIC_REPRESENTATION_ITEM ( )  RATIONAL_B_SPLINE_CURVE ( ( 1.000000000000000000, 0.9238795325112867385, 1.000000000000000000, 0.9238795325112848511, 1.000000000000001776 ) ) 
 REPRESENTATION_ITEM ( '' )  );
#21850 = CARTESIAN_POINT ( 'NONE',  ( 181.8548138422181921, 39.71015625108393010, -5.444914386472297529 ) ) ;
#21851 = ORIENTED_EDGE ( 'NONE', *, *, #12453, .T. ) ;
#21852 = CARTESIAN_POINT ( 'NONE',  ( 55.70494972787295751, 36.08867187608393579, 9.295050272127047819 ) ) ;
#21853 = CARTESIAN_POINT ( 'NONE',  ( 97.71650635000000307, 124.8750000005462368, -9.540979117872439019E-15 ) ) ;
#21854 = CARTESIAN_POINT ( 'NONE',  ( 64.67527568880393574, 53.49346745874647269, -14.99999999999999822 ) ) ;
#21855 = VERTEX_POINT ( 'NONE', #27054 ) ;
#21856 = CARTESIAN_POINT ( 'NONE',  ( 93.00000000000001421, 107.7255621263696668, -49.89999999999999858 ) ) ;
#21857 = CARTESIAN_POINT ( 'NONE',  ( 13.57481594606304753, 33.60820312716787583, -5.622872871577873966 ) ) ;
#21858 = CARTESIAN_POINT ( 'NONE',  ( 103.5355339059327235, 92.74999999726881583, 3.535533905932724874 ) ) ;
#21859 = CARTESIAN_POINT ( 'NONE',  ( 116.8548138422182063, 40.50390625108394005, -5.444914386472297529 ) ) ;
#21860 = CARTESIAN_POINT ( 'NONE',  ( -5.444914386472297529, 39.80937500108393579, -13.14518615778179722 ) ) ;
#21861 = ADVANCED_FACE ( 'NONE', ( #20770 ), #16345, .T. ) ;
#21862 = CARTESIAN_POINT ( 'NONE',  ( 96.46446609406726225, 95.24999999726881583, -3.535533905932738197 ) ) ;
#21863 = CARTESIAN_POINT ( 'NONE',  ( 55.70494972787295751, 37.67617187608393436, 9.295050272127047819 ) ) ;
#21864 = CARTESIAN_POINT ( 'NONE',  ( -20.00000000000000355, 80.00000000000000000, -10.00000000000000000 ) ) ;
#21865 = CARTESIAN_POINT ( 'NONE',  ( 200.4449143864723055, 35.74140625108393721, -13.14518615778179900 ) ) ;
#21866 = ORIENTED_EDGE ( 'NONE', *, *, #19253, .T. ) ;
#21867 = ORIENTED_EDGE ( 'NONE', *, *, #24397, .T. ) ;
#21868 = CARTESIAN_POINT ( 'NONE',  ( -9.295050272127044266, 37.67617187608393436, 9.295050272127047819 ) ) ;
#21869 = CARTESIAN_POINT ( 'NONE',  ( 101.8468681455907046, 4.458734125000016313, 11.37500000136559386 ) ) ;
#21870 = ADVANCED_FACE ( 'NONE', ( #14194 ), #20634, .T. ) ;
#21871 = CARTESIAN_POINT ( 'NONE',  ( -8.312177448680279460E-16, 38.42031249999999432, -13.57481594606304576 ) ) ;
#21872 = CARTESIAN_POINT ( 'NONE',  ( 98.15313185440923860, 81.62500000136560629, 4.458734124999987891 ) ) ;
#21873 = CARTESIAN_POINT ( 'NONE',  ( 204.2950502721270425, 38.66835937608393436, -9.295050272127046043 ) ) ;
#21874 = EDGE_CURVE ( 'NONE', #6277, #8833, #6217, .T. ) ;
#21875 = CARTESIAN_POINT ( 'NONE',  ( -13.14518615778179722, 36.73359375108393010, -5.444914386472297529 ) ) ;
#21876 = CARTESIAN_POINT ( 'NONE',  ( -8.312177448680279460E-16, 39.31328125216787583, -13.57481594606304576 ) ) ;
#21877 = LINE ( 'NONE', #2353, #15745 ) ;
#21878 = CARTESIAN_POINT ( 'NONE',  ( 65.00000000000000000, 40.00781250000000000, -13.57481594606304576 ) ) ;
#21879 = CARTESIAN_POINT ( 'NONE',  ( 93.46109445667489979, 105.2492070361643215, -51.42499999726882010 ) ) ;
#21880 = ADVANCED_FACE ( 'NONE', ( #1532 ), #18766, .F. ) ;
#21881 = ORIENTED_EDGE ( 'NONE', *, *, #21317, .F. ) ;
#21882 = VECTOR ( 'NONE', #6490, 1000.000000000000000 ) ;
#21883 = CARTESIAN_POINT ( 'NONE',  ( -13.57481594606304576, 35.49335937499999005, 5.622872871577880183 ) ) ;
#21884 = CARTESIAN_POINT ( 'NONE',  ( -13.14518615778179544, 36.58476562608393579, 0.000000000000000000 ) ) ;
#21885 =( BOUNDED_SURFACE ( )  B_SPLINE_SURFACE ( 1, 2, ( 
 ( #19564, #48, #10851, #6871, #2612, #13407, #11274, #17562, #17709, #2190, #21573, #26552, #2332, #15556, #19994, #4322, #13120, #15267, #9017, #17421, #23986, #14990, #10990, #19702, #28125, #24265, #4601, #2048, #26266, #21992, #26412, #474, #23707, #26120, #6726, #25982, #15412, #19844, #24128, #13260, #4747, #331, #10716, #17279, #6452, #15123, #12980, #21716, #18131, #15703, #20568, #14126, #22705, #7292, #13977, #20273, #24695, #2754, #5457, #13555, #3173, #5173, #9432, #7007, #11845, #13836, #7580, #20136, #9720, #26697, #17988, #26987, #22562, #26843, #2885, #24550, #11985, #7432, #9291, #20709, #22847, #22416, #9577, #16274, #3314, #5033, #15981, #615, #24972, #7147, #18422, #3028, #11697, #1048, #16127, #27130, #24404, #4892, #1191, #9859, #20422, #906, #18566, #18281, #22279, #24834, #11417, #15841, #13699, #11556, #5316, #758, #3598, #1464, #10120, #5876, #9991, #27268, #20983, #12119, #4011, #21116, #23535, #21403, #12395, #14546, #27677, #1603, #23261, #14674, #1881, #6010, #25249, #10544, #18969, #7724, #3735, #19111, #16416, #10259, #12256, #8140, #16834, #14810, #16558, #1739, #18833, #10405, #25113, #27540, #27819, #12677, #3868, #12530, #7997, #8272, #21258, #7864, #25530, #22986, #23395, #5600, #5739, #16963, #16696, #25663, #6145, #3454, #25395, #14266, #20846, #1324, #18700, #14406, #27403, #23123, #12812, #4568, #4287, #10816, #6689, #25946, #8410 ),
 ( #22104, #23809, #12944, #15090, #11101, #26379, #17671, #6835, #4433, #21961, #6421, #25802, #2582, #6553, #19813, #15525, #28092, #17388, #19531, #13085, #8555, #19251, #27953, #26086, #8981, #2300, #17244, #19671, #2440, #13, #10960, #13229, #21824, #8697, #297, #15378, #21680, #24233, #15233, #4714, #154, #2011, #23951, #13374, #21535, #8839, #17529, #2154, #10680, #4152, #17099, #19387, #26231, #6279, #24093, #14955, #23675, #1019, #20389, #9690, #7113, #20536, #24941, #18389, #5427, #15813, #15672, #9547, #11384, #13805, #9399, #2856, #4859, #24664, #26957, #2995, #22245, #876, #2723, #6976, #5005, #22815, #19960, #11814, #27095, #18098, #7400, #727, #26667, #14096, #24518, #13668, #22382, #3146, #7548, #16244, #11242, #5139, #13947, #11523, #17816, #437, #26811, #9123, #26520, #20106, #7259, #20242, #22528, #584, #24371, #13525, #15949, #9262, #11668, #17956, #18249, #22674, #16093, #24801, #5283, #25362, #12222, #3835, #18936, #16526, #10751, #27509, #19462, #5842, #14235, #10090, #16800, #25083, #20950, #18803, #25218, #5571, #16384, #21604, #22957, #14511, #26014, #3419, #11954, #1431, #2082, #12366, #28159, #27373, #12874, #17315, #8626, #6485, #7832, #7693, #1573, #12087, #23228, #7965, #23089, #20810, #16666, #27645, #3705, #1290, #21085, #9959, #27237, #5708, #15159, #20677, #3283, #1160, #14374, #14644, #9825, #3563, #23363, #18532, #8106, #25497, #10226 ) ),
 .UNSPECIFIED., .F., .F., .F. ) 
 B_SPLINE_SURFACE_WITH_KNOTS ( ( 2, 2 ),
 ( 3, 2, 2, 2, 2, 2, 2, 2, 2, 2, 2, 2, 2, 2, 2, 2, 2, 2, 2, 2, 2, 2, 2, 2, 2, 2, 2, 2, 2, 2, 2, 2, 2, 2, 2, 2, 2, 2, 2, 2, 2, 2, 2, 2, 2, 2, 2, 2, 2, 2, 2, 2, 2, 2, 2, 2, 2, 2, 2, 2, 2, 2, 2, 2, 2, 2, 2, 2, 2, 2, 2, 2, 2, 2, 2, 2, 2, 2, 2, 2, 2, 2, 2, 2, 2, 2, 2, 2, 2, 2, 2, 3 ),
 ( 0.000000000000000000, 1.000000000000000000 ),
 ( 0.000000000000000000, 0.01041666666666666609, 0.02083333333333333218, 0.03125000000000000000, 0.04166666666666666435, 0.05208333333333333565, 0.06250000000000000000, 0.07291666666666667129, 0.08333333333333332871, 0.09375000000000000000, 0.1041666666666666713, 0.1145833333333333287, 0.1250000000000000000, 0.1354166666666666574, 0.1458333333333333426, 0.1562500000000000000, 0.1666666666666666574, 0.1770833333333333426, 0.1875000000000000000, 0.1979166666666666574, 0.2083333333333333426, 0.2187500000000000000, 0.2291666666666666574, 0.2395833333333333426, 0.2500000000000000000, 0.2604166666666666852, 0.2708333333333333148, 0.2812500000000000000, 0.2916666666666666852, 0.3020833333333333148, 0.3125000000000000000, 0.3229166666666666852, 0.3333333333333333148, 0.3437500000000000000, 0.3541666666666666852, 0.3645833333333333148, 0.3750000000000000000, 0.3854166666666666852, 0.3958333333333333148, 0.4062500000000000000, 0.4166666666666666852, 0.4270833333333333148, 0.4375000000000000000, 0.4479166666666666852, 0.4583333333333333148, 0.4687500000000000000, 0.4791666666666666852, 0.4895833333333333148, 0.5000000000000000000, 0.5104166666666666297, 0.5208333333333333703, 0.5312500000000000000, 0.5416666666666666297, 0.5520833333333333703, 0.5625000000000000000, 0.5729166666666666297, 0.5833333333333333703, 0.5937500000000000000, 0.6041666666666666297, 0.6145833333333333703, 0.6250000000000000000, 0.6354166666666666297, 0.6458333333333333703, 0.6562500000000000000, 0.6666666666666666297, 0.6770833333333333703, 0.6875000000000000000, 0.6979166666666666297, 0.7083333333333333703, 0.7187500000000000000, 0.7291666666666666297, 0.7395833333333333703, 0.7500000000000000000, 0.7604166666666666297, 0.7708333333333333703, 0.7812500000000000000, 0.7916666666666666297, 0.8020833333333333703, 0.8125000000000000000, 0.8229166666666666297, 0.8333333333333333703, 0.8437500000000000000, 0.8541666666666666297, 0.8645833333333333703, 0.8750000000000000000, 0.8854166666666666297, 0.8958333333333333703, 0.9062500000000000000, 0.9166666666666666297, 0.9270833333333333703, 0.9375000000000000000, 0.9448587001587775980 ),
 .UNSPECIFIED. ) 
 GEOMETRIC_REPRESENTATION_ITEM ( )  RATIONAL_B_SPLINE_SURFACE ( (
 ( 1.000000000000000000, 0.9238795325112867385, 1.000000000000000000, 0.9238795325112867385, 1.000000000000000000, 0.9238795325112867385, 1.000000000000000000, 0.9238795325112867385, 1.000000000000000000, 0.9238795325112867385, 1.000000000000000000, 0.9238795325112867385, 1.000000000000000000, 0.9238795325112867385, 1.000000000000000000, 0.9238795325112867385, 1.000000000000000000, 0.9238795325112867385, 1.000000000000000000, 0.9238795325112867385, 1.000000000000000000, 0.9238795325112867385, 1.000000000000000000, 0.9238795325112867385, 1.000000000000000000, 0.9238795325112867385, 1.000000000000000000, 0.9238795325112867385, 1.000000000000000000, 0.9238795325112867385, 1.000000000000000000, 0.9238795325112867385, 1.000000000000000000, 0.9238795325112867385, 1.000000000000000000, 0.9238795325112867385, 1.000000000000000000, 0.9238795325112867385, 1.000000000000000000, 0.9238795325112867385, 1.000000000000000000, 0.9238795325112867385, 1.000000000000000000, 0.9238795325112867385, 1.000000000000000000, 0.9238795325112867385, 1.000000000000000000, 0.9238795325112867385, 1.000000000000000000, 0.9238795325112867385, 1.000000000000000000, 0.9238795325112867385, 1.000000000000000000, 0.9238795325112867385, 1.000000000000000000, 0.9238795325112867385, 1.000000000000000000, 0.9238795325112867385, 1.000000000000000000, 0.9238795325112867385, 1.000000000000000000, 0.9238795325112867385, 1.000000000000000000, 0.9238795325112867385, 1.000000000000000000, 0.9238795325112867385, 1.000000000000000000, 0.9238795325112867385, 1.000000000000000000, 0.9238795325112867385, 1.000000000000000000, 0.9238795325112867385, 1.000000000000000000, 0.9238795325112867385, 1.000000000000000000, 0.9238795325112867385, 1.000000000000000000, 0.9238795325112867385, 1.000000000000000000, 0.9238795325112867385, 1.000000000000000000, 0.9238795325112867385, 1.000000000000000000, 0.9238795325112867385, 1.000000000000000000, 0.9238795325112867385, 1.000000000000000000, 0.9238795325112867385, 1.000000000000000000, 0.9238795325112867385, 1.000000000000000000, 0.9238795325112867385, 1.000000000000000000, 0.9238795325112867385, 1.000000000000000000, 0.9238795325112867385, 1.000000000000000000, 0.9238795325112867385, 1.000000000000000000, 0.9238795325112867385, 1.000000000000000000, 0.9238795325112867385, 1.000000000000000000, 0.9238795325112867385, 1.000000000000000000, 0.9238795325112867385, 1.000000000000000000, 0.9238795325112867385, 1.000000000000000000, 0.9238795325112867385, 1.000000000000000000, 0.9238795325112867385, 1.000000000000000000, 0.9238795325112867385, 1.000000000000000000, 0.9238795325112867385, 1.000000000000000000, 0.9238795325112867385, 1.000000000000000000, 0.9238795325112867385, 1.000000000000000000, 0.9238795325112867385, 1.000000000000000000, 0.9238795325112867385, 1.000000000000000000, 0.9238795325112867385, 1.000000000000000000, 0.9238795325112867385, 1.000000000000000000, 0.9238795325112867385, 1.000000000000000000, 0.9238795325112867385, 1.000000000000000000, 0.9238795325112867385, 1.000000000000000000, 0.9238795325112867385, 1.000000000000000000, 0.9238795325112867385, 1.000000000000000000, 0.9238795325112867385, 1.000000000000000000, 0.9238795325112867385, 1.000000000000000000, 0.9238795325112867385, 1.000000000000000000, 0.9238795325112867385, 1.000000000000000000, 0.9238795325112867385, 1.000000000000000000, 0.9238795325112867385, 1.000000000000000000, 0.9238795325112867385, 1.000000000000000000, 0.9238795325112867385, 1.000000000000000000, 0.9238795325112867385, 1.000000000000000000, 0.9238795325112867385, 1.000000000000000000, 0.9238795325112867385, 1.000000000000000000, 0.9238795325112867385, 1.000000000000000000, 0.9238795325112867385, 1.000000000000000000, 0.9238795325112867385, 1.000000000000000000, 0.9238795325112867385, 1.000000000000000000, 0.9238795325112867385, 1.000000000000000000, 0.9238795325112867385, 1.000000000000000000, 0.9238795325112867385, 1.000000000000000000, 0.9238795325112867385, 1.000000000000000000, 0.9238795325112867385, 1.000000000000000000, 0.9238795325112867385, 1.000000000000000000, 0.9462258211652395667, 0.9684275895297407288),
 ( 1.000000000000000000, 0.9238795325112867385, 1.000000000000000000, 0.9238795325112867385, 1.000000000000000000, 0.9238795325112867385, 1.000000000000000000, 0.9238795325112867385, 1.000000000000000000, 0.9238795325112867385, 1.000000000000000000, 0.9238795325112867385, 1.000000000000000000, 0.9238795325112867385, 1.000000000000000000, 0.9238795325112867385, 1.000000000000000000, 0.9238795325112867385, 1.000000000000000000, 0.9238795325112867385, 1.000000000000000000, 0.9238795325112867385, 1.000000000000000000, 0.9238795325112867385, 1.000000000000000000, 0.9238795325112867385, 1.000000000000000000, 0.9238795325112867385, 1.000000000000000000, 0.9238795325112867385, 1.000000000000000000, 0.9238795325112867385, 1.000000000000000000, 0.9238795325112867385, 1.000000000000000000, 0.9238795325112867385, 1.000000000000000000, 0.9238795325112867385, 1.000000000000000000, 0.9238795325112867385, 1.000000000000000000, 0.9238795325112867385, 1.000000000000000000, 0.9238795325112867385, 1.000000000000000000, 0.9238795325112867385, 1.000000000000000000, 0.9238795325112867385, 1.000000000000000000, 0.9238795325112867385, 1.000000000000000000, 0.9238795325112867385, 1.000000000000000000, 0.9238795325112867385, 1.000000000000000000, 0.9238795325112867385, 1.000000000000000000, 0.9238795325112867385, 1.000000000000000000, 0.9238795325112867385, 1.000000000000000000, 0.9238795325112867385, 1.000000000000000000, 0.9238795325112867385, 1.000000000000000000, 0.9238795325112867385, 1.000000000000000000, 0.9238795325112867385, 1.000000000000000000, 0.9238795325112867385, 1.000000000000000000, 0.9238795325112867385, 1.000000000000000000, 0.9238795325112867385, 1.000000000000000000, 0.9238795325112867385, 1.000000000000000000, 0.9238795325112867385, 1.000000000000000000, 0.9238795325112867385, 1.000000000000000000, 0.9238795325112867385, 1.000000000000000000, 0.9238795325112867385, 1.000000000000000000, 0.9238795325112867385, 1.000000000000000000, 0.9238795325112867385, 1.000000000000000000, 0.9238795325112867385, 1.000000000000000000, 0.9238795325112867385, 1.000000000000000000, 0.9238795325112867385, 1.000000000000000000, 0.9238795325112867385, 1.000000000000000000, 0.9238795325112867385, 1.000000000000000000, 0.9238795325112867385, 1.000000000000000000, 0.9238795325112867385, 1.000000000000000000, 0.9238795325112867385, 1.000000000000000000, 0.9238795325112867385, 1.000000000000000000, 0.9238795325112867385, 1.000000000000000000, 0.9238795325112867385, 1.000000000000000000, 0.9238795325112867385, 1.000000000000000000, 0.9238795325112867385, 1.000000000000000000, 0.9238795325112867385, 1.000000000000000000, 0.9238795325112867385, 1.000000000000000000, 0.9238795325112867385, 1.000000000000000000, 0.9238795325112867385, 1.000000000000000000, 0.9238795325112867385, 1.000000000000000000, 0.9238795325112867385, 1.000000000000000000, 0.9238795325112867385, 1.000000000000000000, 0.9238795325112867385, 1.000000000000000000, 0.9238795325112867385, 1.000000000000000000, 0.9238795325112867385, 1.000000000000000000, 0.9238795325112867385, 1.000000000000000000, 0.9238795325112867385, 1.000000000000000000, 0.9238795325112867385, 1.000000000000000000, 0.9238795325112867385, 1.000000000000000000, 0.9238795325112867385, 1.000000000000000000, 0.9238795325112867385, 1.000000000000000000, 0.9238795325112867385, 1.000000000000000000, 0.9238795325112867385, 1.000000000000000000, 0.9238795325112867385, 1.000000000000000000, 0.9238795325112867385, 1.000000000000000000, 0.9238795325112867385, 1.000000000000000000, 0.9238795325112867385, 1.000000000000000000, 0.9238795325112867385, 1.000000000000000000, 0.9238795325112867385, 1.000000000000000000, 0.9238795325112867385, 1.000000000000000000, 0.9238795325112867385, 1.000000000000000000, 0.9238795325112867385, 1.000000000000000000, 0.9238795325112867385, 1.000000000000000000, 0.9238795325112867385, 1.000000000000000000, 0.9238795325112867385, 1.000000000000000000, 0.9238795325112867385, 1.000000000000000000, 0.9238795325112867385, 1.000000000000000000, 0.9238795325112867385, 1.000000000000000000, 0.9462258211652395667, 0.9684275895297407288) ) ) 
 REPRESENTATION_ITEM ( '' )  SURFACE ( )  );
#21886 = CARTESIAN_POINT ( 'NONE',  ( 102.0710678118654329, 5.000000000000018652, 0.8125000027311859441 ) ) ;
#21887 = CARTESIAN_POINT ( 'NONE',  ( 130.0000000000000000, 35.79101562608394005, -13.14518615778179544 ) ) ;
#21888 = CARTESIAN_POINT ( 'NONE',  ( 74.29505027212704249, 33.90585937608393152, -9.295050272127046043 ) ) ;
#21889 = EDGE_CURVE ( 'NONE', #25660, #24967, #16234, .T. ) ;
#21890 = CARTESIAN_POINT ( 'NONE',  ( 181.8548138422181921, 38.42031250108393436, 5.444914386472304635 ) ) ;
#21891 = ORIENTED_EDGE ( 'NONE', *, *, #17322, .F. ) ;
#21892 = DIRECTION ( 'NONE',  ( 0.000000000000000000, -1.000000000000000000, 0.000000000000000000 ) ) ;
#21893 =( BOUNDED_CURVE ( )  B_SPLINE_CURVE ( 2, ( #18640, #7515, #14340, #23057, #20920, #27616, #12467, #21192, #1677 ),
 .UNSPECIFIED., .F., .F. ) 
 B_SPLINE_CURVE_WITH_KNOTS ( ( 3, 2, 2, 2, 3 ),
 ( 0.06250000000000004163, 0.07291666666666665741, 0.08333333333333325932, 0.09374999999999987510, 0.1041666666666664909 ),
 .UNSPECIFIED. ) 
 CURVE ( )  GEOMETRIC_REPRESENTATION_ITEM ( )  RATIONAL_B_SPLINE_CURVE ( ( 0.9999999999999996669, 0.9238795325112870716, 1.000000000000000000, 0.9238795325112867385, 1.000000000000000000, 0.9238795325112867385, 1.000000000000000000, 0.9238795325112880708, 0.9999999999999986677 ) ) 
 REPRESENTATION_ITEM ( '' )  );
#21894 = CARTESIAN_POINT ( 'NONE',  ( -13.14518615778179189, 33.45937500108392726, 5.444914386472304635 ) ) ;
#21895 = CARTESIAN_POINT ( 'NONE',  ( 2.493653234604083739E-15, 38.02343749999999289, 13.57481594606304576 ) ) ;
#21896 = CARTESIAN_POINT ( 'NONE',  ( 97.50000000000000000, 123.3999999999999915, -9.540979117872439019E-15 ) ) ;
#21897 = DIRECTION ( 'NONE',  ( 0.000000000000000000, 0.000000000000000000, -1.000000000000000000 ) ) ;
#21898 = LINE ( 'NONE', #23879, #19002 ) ;
#21899 = CARTESIAN_POINT ( 'NONE',  ( 0.3247243111960362305, 53.49346745874646558, 14.99999999999999822 ) ) ;
#21900 = CARTESIAN_POINT ( 'NONE',  ( 99.99999999999995737, 79.37500000273119838, 4.999999999999990230 ) ) ;
#21901 = CARTESIAN_POINT ( 'NONE',  ( 102.0710678118654329, -4.999999999999989342, 10.31249999999999822 ) ) ;
#21902 = VECTOR ( 'NONE', #16870, 1000.000000000000000 ) ;
#21903 = CARTESIAN_POINT ( 'NONE',  ( 104.4587341249999781, -1.846868145590721655, 8.875000001365593860 ) ) ;
#21904 = VERTEX_POINT ( 'NONE', #25316 ) ;
#21905 = CARTESIAN_POINT ( 'NONE',  ( 98.53841926354351699, 123.8500000010924680, 1.461580736456455920 ) ) ;
#21906 = CARTESIAN_POINT ( 'NONE',  ( 104.4587341249999781, -1.846868145590721655, 13.87500000136559208 ) ) ;
#21907 = CARTESIAN_POINT ( 'NONE',  ( 129.1610731307196147, 53.50081894914377045, 14.99999999999996447 ) ) ;
#21908 = CARTESIAN_POINT ( 'NONE',  ( 2.414731522848535132E-15, 39.95820312608393010, 13.14518615778179544 ) ) ;
#21909 = CARTESIAN_POINT ( 'NONE',  ( 13.57481594606304753, 32.71523437500000142, -5.622872871577873966 ) ) ;
#21910 = CARTESIAN_POINT ( 'NONE',  ( 96.84719886470459471, 82.81250000136560629, 3.152801135295355994 ) ) ;
#21911 = CARTESIAN_POINT ( 'NONE',  ( 55.70494972787295751, 36.68398437608393436, -9.295050272127046043 ) ) ;
#21912 = CARTESIAN_POINT ( 'NONE',  ( 95.00472066334982912, 103.1245878333314323, -48.82500000273118701 ) ) ;
#21913 = CARTESIAN_POINT ( 'NONE',  ( -5.444914386472299306, 37.52734375108393294, 13.14518615778179722 ) ) ;
#21914 = CARTESIAN_POINT ( 'NONE',  ( 107.5412658750000077, 110.0000000000000000, -54.68750000136559919 ) ) ;
#21915 = CARTESIAN_POINT ( 'NONE',  ( 124.3771271284221029, 36.08867187500000284, -13.57481594606300135 ) ) ;
#21916 = CARTESIAN_POINT ( 'NONE',  ( 94.33688103937534208, 114.1144967660473242, -54.69999999453764161 ) ) ;
#21917 = CARTESIAN_POINT ( 'NONE',  ( 124.3771271284221314, 37.18007812500000853, 13.57481594606304753 ) ) ;
#21918 = EDGE_CURVE ( 'NONE', #1909, #16468, #5527, .T. ) ;
#21919 = ORIENTED_EDGE ( 'NONE', *, *, #11787, .T. ) ;
#21920 = CARTESIAN_POINT ( 'NONE',  ( 104.3262379212492448, 104.0454443415356991, -55.79999999453763593 ) ) ;
#21921 = CARTESIAN_POINT ( 'NONE',  ( 5.444914386472297529, 35.74140625108393721, -13.14518615778179900 ) ) ;
#21922 = CARTESIAN_POINT ( 'NONE',  ( -13.57481594606304576, 38.76757812716787299, 5.622872871577880183 ) ) ;
#21923 = CARTESIAN_POINT ( 'NONE',  ( 135.4449143864723055, 35.54296875108393294, -13.14518615778179900 ) ) ;
#21924 = CARTESIAN_POINT ( 'NONE',  ( 59.37712712842213136, 33.01289062716787726, -13.57481594606304753 ) ) ;
#21925 = PLANE ( 'NONE',  #689 ) ;
#21926 = CARTESIAN_POINT ( 'NONE',  ( -13.14518615778179900, 40.50390625108394005, -5.444914386472297529 ) ) ;
#21927 = CARTESIAN_POINT ( 'NONE',  ( 102.0710678118654329, -4.999999999999989342, 5.312499999999999112 ) ) ;
#21928 = CARTESIAN_POINT ( 'NONE',  ( 93.46109445667489979, 114.7507929638356785, -46.07499999726881867 ) ) ;
#21929 = CARTESIAN_POINT ( 'NONE',  ( 181.8548138422181921, 33.45937500108392726, 5.444914386472304635 ) ) ;
#21930 = DIRECTION ( 'NONE',  ( -0.000000000000000000, 1.000000000000000000, -0.000000000000000000 ) ) ;
#21931 = CARTESIAN_POINT ( 'NONE',  ( 9.598844408820456309, 34.45156250216787441, -9.598844408820458085 ) ) ;
#21933 = EDGE_LOOP ( 'NONE', ( #11949, #19909, #11157, #11692 ) ) ;
#21932 = DIRECTION ( 'NONE',  ( 0.000000000000000000, 0.000000000000000000, 1.000000000000000000 ) ) ;
#21934 = CARTESIAN_POINT ( 'NONE',  ( 97.92893218813451028, 5.000000000000018652, 6.812499999999999112 ) ) ;
#21935 = CARTESIAN_POINT ( 'NONE',  ( 139.1801758136479918, 55.00000000000000000, 14.99999999999996270 ) ) ;
#21936 = CARTESIAN_POINT ( 'NONE',  ( 9.598844408820456309, 36.73359374999999716, -9.598844408820458085 ) ) ;
#21937 = CARTESIAN_POINT ( 'NONE',  ( 0.000000000000000000, 40.99999999999999289, 0.000000000000000000 ) ) ;
#21938 = CARTESIAN_POINT ( 'NONE',  ( -8.049105076161786076E-16, 37.37851562608393863, -13.14518615778179544 ) ) ;
#21939 = CARTESIAN_POINT ( 'NONE',  ( 9.295050272127047819, 36.88242187608393152, 9.295050272127046043 ) ) ;
#21940 = CARTESIAN_POINT ( 'NONE',  ( 208.5748159460630120, 35.89023437499999858, -5.622872871577873077 ) ) ;
#21941 = CARTESIAN_POINT ( 'NONE',  ( 91.91746824999998466, 112.6261737610028320, -45.47500000273119980 ) ) ;
#21942 = CARTESIAN_POINT ( 'NONE',  ( 96.84719886470459471, -3.152801135295355994, 0.8125000013655924169 ) ) ;
#21943 = CARTESIAN_POINT ( 'NONE',  ( 59.55508561352770158, 35.64218750108392442, -13.14518615778179900 ) ) ;
#21944 = CARTESIAN_POINT ( 'NONE',  ( 104.4587341249999639, 1.442382525525748735E-14, 2.937500001365592528 ) ) ;
#21945 = CARTESIAN_POINT ( 'NONE',  ( 97.49603539231829075, 123.0000000000000000, 0.01993142876900604391 ) ) ;
#21946 = CARTESIAN_POINT ( 'NONE',  ( 130.0000000000000000, -7.395377635281828788, -13.57481594606305997 ) ) ;
#21947 = CARTESIAN_POINT ( 'NONE',  ( -9.598844408820458085, 36.93203124999999432, -9.598844408820458085 ) ) ;
#21948 = CARTESIAN_POINT ( 'NONE',  ( 130.0000000000000000, 36.98164062608393721, 13.14518615778179544 ) ) ;
#21949 = VERTEX_POINT ( 'NONE', #3666 ) ;
#21950 = CARTESIAN_POINT ( 'NONE',  ( 104.9999999999999574, 82.56250000000002842, -2.071067811865491937 ) ) ;
#21951 = CARTESIAN_POINT ( 'NONE',  ( 104.9999999999999716, 82.62500000273119838, -1.449011120738813565E-14 ) ) ;
#21952 = CARTESIAN_POINT ( 'NONE',  ( 102.0710678118654613, 90.18749999999998579, -4.999999999999997335 ) ) ;
#21953 = CARTESIAN_POINT ( 'NONE',  ( 52.43349327520137138, 36.00000000000001421, -4.295155080288876270 ) ) ;
#21954 = CARTESIAN_POINT ( 'NONE',  ( 92.99999999999998579, 110.0000000000000000, -51.00000000000000711 ) ) ;
#21955 = CARTESIAN_POINT ( 'NONE',  ( 70.44491438647230552, 32.26875000108393721, 13.14518615778179189 ) ) ;
#21956 = VERTEX_POINT ( 'NONE', #14330 ) ;
#21957 = CARTESIAN_POINT ( 'NONE',  ( 5.622872871577924592, 32.61601562716786873, 13.57481594606299957 ) ) ;
#21958 = CARTESIAN_POINT ( 'NONE',  ( 95.54126587499995082, -1.846868145590724986, 1.750000001365591862 ) ) ;
#21959 = ORIENTED_EDGE ( 'NONE', *, *, #19889, .T. ) ;
#21960 = CARTESIAN_POINT ( 'NONE',  ( -13.14518615778179722, 32.76484375108393010, -5.444914386472297529 ) ) ;
#21961 = CARTESIAN_POINT ( 'NONE',  ( 13.14518615778179900, 40.30546875108393579, 5.444914386472293977 ) ) ;
#21962 = CARTESIAN_POINT ( 'NONE',  ( 204.5988444088204687, 34.25312500216787015, 9.598844408820456309 ) ) ;
#21963 =( BOUNDED_CURVE ( )  B_SPLINE_CURVE ( 2, ( #20560, #13548, #11548, #18272, #2746, #11408, #7138, #15833, #7283 ),
 .UNSPECIFIED., .F., .T. ) 
 B_SPLINE_CURVE_WITH_KNOTS ( ( 3, 2, 2, 2, 3 ),
 ( 0.9642857142857141906, 0.9732142857142855874, 0.9821428571428569843, 0.9910714285714286031, 1.000000000000000000 ),
 .UNSPECIFIED. ) 
 CURVE ( )  GEOMETRIC_REPRESENTATION_ITEM ( )  RATIONAL_B_SPLINE_CURVE ( ( 1.000000000000000888, 0.9238795325112857393, 1.000000000000000000, 0.9238795325112867385, 1.000000000000000000, 0.9238795325112867385, 1.000000000000000000, 0.9238795325112867385, 1.000000000000000000 ) ) 
 REPRESENTATION_ITEM ( '' )  );
#21964 = VERTEX_POINT ( 'NONE', #12328 ) ;
#21965 = CARTESIAN_POINT ( 'NONE',  ( 13.14518615778179544, 36.98164062608393010, -1.609821015232357215E-15 ) ) ;
#21966 = CARTESIAN_POINT ( 'NONE',  ( 99.99999999999998579, 110.0000000000000000, -43.00000000000000000 ) ) ;
#21967 = LINE ( 'NONE', #20111, #15249 ) ;
#21968 = CARTESIAN_POINT ( 'NONE',  ( 2.414731522848535132E-15, 35.39414062608393863, 13.14518615778179544 ) ) ;
#21969 = CARTESIAN_POINT ( 'NONE',  ( 143.1451861577818079, 35.44375000108393436, -5.444914386472297529 ) ) ;
#21970 = CARTESIAN_POINT ( 'NONE',  ( 70.62287287157788285, 34.10429687499999574, 13.57481594606304576 ) ) ;
#21971 = CARTESIAN_POINT ( 'NONE',  ( -13.57481594606304398, 34.69960937499999432, 5.622872871577880183 ) ) ;
#21972 = CARTESIAN_POINT ( 'NONE',  ( 104.4587341249999781, 1.846868145590750299, 11.25000000136559208 ) ) ;
#21973 = CARTESIAN_POINT ( 'NONE',  ( 2.493653234604083739E-15, 38.81718749999999574, 13.57481594606304576 ) ) ;
#21974 = CARTESIAN_POINT ( 'NONE',  ( 104.4587341249999781, -1.846868145590721655, 13.87500000136559208 ) ) ;
#21975 = CARTESIAN_POINT ( 'NONE',  ( 106.5389055433251002, 114.7507929638356785, -49.92500000273119554 ) ) ;
#21976 = DIRECTION ( 'NONE',  ( -1.000000000000000000, 0.000000000000000000, 0.000000000000000000 ) ) ;
#21977 = DIRECTION ( 'NONE',  ( -1.000000000000000000, 0.000000000000000000, 0.000000000000000000 ) ) ;
#21978 = CARTESIAN_POINT ( 'NONE',  ( 93.46109445667489979, 105.2492070361643215, -49.42499999726882010 ) ) ;
#21979 = CARTESIAN_POINT ( 'NONE',  ( -8.049105076161786076E-16, 35.79101562608394005, -13.14518615778179544 ) ) ;
#21980 = CARTESIAN_POINT ( 'NONE',  ( 93.46109445667489979, 105.2492070361643215, -51.67499999726882010 ) ) ;
#21981 = VERTEX_POINT ( 'NONE', #10184 ) ;
#21982 = CARTESIAN_POINT ( 'NONE',  ( 105.6631189606246295, 114.1144967660473242, -51.30000000546237970 ) ) ;
#21983 = CARTESIAN_POINT ( 'NONE',  ( 195.0000000000000000, 36.43593749999999432, 13.57481594606304576 ) ) ;
#21984 = CARTESIAN_POINT ( 'NONE',  ( 195.0000000000000000, 39.95820312608393010, 13.14518615778179544 ) ) ;
#21985 = ORIENTED_EDGE ( 'NONE', *, *, #3565, .F. ) ;
#21986 = CARTESIAN_POINT ( 'NONE',  ( 96.46446609406721961, -3.535533905932727539, 7.250000002731185056 ) ) ;
#21987 = DIRECTION ( 'NONE',  ( 0.000000000000000000, 1.000000000000000000, 0.000000000000000000 ) ) ;
#21988 = CARTESIAN_POINT ( 'NONE',  ( 98.15313185440925281, -4.458734124999987891, 13.87500000136559208 ) ) ;
#21989 = EDGE_CURVE ( 'NONE', #19945, #12986, #24545, .T. ) ;
#21990 = VERTEX_POINT ( 'NONE', #24905 ) ;
#21991 = CARTESIAN_POINT ( 'NONE',  ( 107.0000000000000142, 110.0000000000000000, -53.00000000000000711 ) ) ;
#21992 = CARTESIAN_POINT ( 'NONE',  ( -5.444914386472299306, 39.11484375108394573, 13.14518615778179722 ) ) ;
#21993 = CARTESIAN_POINT ( 'NONE',  ( 102.4999999999999858, 124.6000000000000085, -9.847140817659276890E-15 ) ) ;
#21994 = VECTOR ( 'NONE', #23442, 1000.000000000000000 ) ;
#21995 = CARTESIAN_POINT ( 'NONE',  ( 143.1451861577818079, 40.15664062608393436, -1.609821015232357215E-15 ) ) ;
#21996 = LINE ( 'NONE', #24408, #8898 ) ;
#21997 = CARTESIAN_POINT ( 'NONE',  ( 96.46446609406726225, 94.24999999726881583, -3.535533905932738197 ) ) ;
#21998 = CARTESIAN_POINT ( 'NONE',  ( 55.70494972787295751, 36.68398437608393436, -9.295050272127046043 ) ) ;
#21999 = CARTESIAN_POINT ( 'NONE',  ( 9.598844408820456309, 37.52734375000000000, -9.598844408820458085 ) ) ;
#22000 = EDGE_LOOP ( 'NONE', ( #27986, #7027, #2672, #24187, #24468, #10726, #20748, #6583, #10391 ) ) ;
#22001 = CARTESIAN_POINT ( 'NONE',  ( 208.1451861577817795, 36.33671875108394289, 5.444914386472293977 ) ) ;
#22002 = ORIENTED_EDGE ( 'NONE', *, *, #4310, .T. ) ;
#22003 = CARTESIAN_POINT ( 'NONE',  ( 2.414731522848535132E-15, 38.56914062608393579, 13.14518615778179544 ) ) ;
#22004 = CARTESIAN_POINT ( 'NONE',  ( 0.000000000000000000, 0.000000000000000000, 0.000000000000000000 ) ) ;
#22005 = CARTESIAN_POINT ( 'NONE',  ( 104.4587341249999781, 1.846868145590750521, 9.250000001365592084 ) ) ;
#22006 = CARTESIAN_POINT ( 'NONE',  ( 74.29505027212704249, 40.25585937608393294, -9.295050272127046043 ) ) ;
#22007 = CARTESIAN_POINT ( 'NONE',  ( 99.99999999999995737, 79.68750000136559208, 4.458734124999988779 ) ) ;
#22008 = CARTESIAN_POINT ( 'NONE',  ( 189.5550856135277229, 38.02343750108394005, -13.14518615778179722 ) ) ;
#22009 = CARTESIAN_POINT ( 'NONE',  ( -8.049105076161786076E-16, 37.37851562608393863, -13.14518615778179544 ) ) ;
#22010 = DIRECTION ( 'NONE',  ( 0.000000000000000000, -1.000000000000000000, 3.469446951953611231E-16 ) ) ;
#22011 = CARTESIAN_POINT ( 'NONE',  ( 0.000000000000000000, 40.99999999999999289, -13.57481594606304576 ) ) ;
#22012 = CARTESIAN_POINT ( 'NONE',  ( 99.99999999999998579, 102.6397644303321215, -49.50000000000000711 ) ) ;
#22013 = CARTESIAN_POINT ( 'NONE',  ( 97.50236033167490746, 117.6869444889999841, -54.02499999726882862 ) ) ;
#22014 = ORIENTED_EDGE ( 'NONE', *, *, #15137, .F. ) ;
#22015 = EDGE_CURVE ( 'NONE', #28147, #16548, #2888, .T. ) ;
#22016 = CARTESIAN_POINT ( 'NONE',  ( -9.598844408820458085, 36.13828124999999147, -9.598844408820458085 ) ) ;
#22017 = CARTESIAN_POINT ( 'NONE',  ( 9.295050272127047819, 38.46992187608393010, 9.295050272127046043 ) ) ;
#22018 = VERTEX_POINT ( 'NONE', #19032 ) ;
#22019 = CARTESIAN_POINT ( 'NONE',  ( 120.7049497278729575, 34.50117187608393721, 9.295050272127047819 ) ) ;
#22020 = CARTESIAN_POINT ( 'NONE',  ( 78.14518615778179367, 32.96328125108393436, 5.444914386472293977 ) ) ;
#22021 = CARTESIAN_POINT ( 'NONE',  ( 181.8548138422181921, 36.73359375108393010, -5.444914386472297529 ) ) ;
#22022 = ORIENTED_EDGE ( 'NONE', *, *, #4430, .F. ) ;
#22023 = CARTESIAN_POINT ( 'NONE',  ( 62.70203941399186931, 36.00000000000001421, 12.97104423350682900 ) ) ;
#22024 = CARTESIAN_POINT ( 'NONE',  ( -8.049105076161786076E-16, 32.41757812608393863, -13.14518615778179544 ) ) ;
#22025 = CARTESIAN_POINT ( 'NONE',  ( 127.4704160048206205, 49.99999999938359707, -13.34625891065716807 ) ) ;
#22026 = EDGE_CURVE ( 'NONE', #4003, #3976, #1943, .T. ) ;
#22027 = DIRECTION ( 'NONE',  ( 0.000000000000000000, 1.000000000000000000, 0.000000000000000000 ) ) ;
#22028 = DIRECTION ( 'NONE',  ( -1.000000000000000000, 0.000000000000000000, 7.228014483236696740E-18 ) ) ;
#22029 = EDGE_CURVE ( 'NONE', #27745, #26423, #21295, .T. ) ;
#22030 = LINE ( 'NONE', #3072, #3358 ) ;
#22031 = CARTESIAN_POINT ( 'NONE',  ( 99.99999999999998579, 123.3000000021849587, -2.499999999999997780 ) ) ;
#22032 = EDGE_CURVE ( 'NONE', #11248, #3337, #24424, .T. ) ;
#22033 = CARTESIAN_POINT ( 'NONE',  ( 97.92893218813451028, -4.999999999999989342, 10.18749999999999822 ) ) ;
#22034 = VERTEX_POINT ( 'NONE', #17028 ) ;
#22035 = CARTESIAN_POINT ( 'NONE',  ( 104.4587341249999781, 1.846868145590750299, 8.000000001365592084 ) ) ;
#22036 = ORIENTED_EDGE ( 'NONE', *, *, #22026, .T. ) ;
#22037 = CARTESIAN_POINT ( 'NONE',  ( 98.96446609406727646, 122.5500000021849587, -2.499999999999997780 ) ) ;
#22038 = CARTESIAN_POINT ( 'NONE',  ( 103.1528011352953342, 3.152801135295383084, 12.06250000136559208 ) ) ;
#22039 = CARTESIAN_POINT ( 'NONE',  ( 121.2416656076439949, 50.00000000000000000, 10.38725784494027238 ) ) ;
#22040 = EDGE_CURVE ( 'NONE', #6189, #25739, #8025, .T. ) ;
#22041 = CARTESIAN_POINT ( 'NONE',  ( 5.444914386472302859, 37.62656250108393863, 13.14518615778179189 ) ) ;
#22042 = DIRECTION ( 'NONE',  ( -5.782411586589357392E-17, 0.000000000000000000, -1.000000000000000000 ) ) ;
#22043 = CYLINDRICAL_SURFACE ( 'NONE', #2852, 11.57481594606304398 ) ;
#22044 = CARTESIAN_POINT ( 'NONE',  ( 59.55508561352770158, 33.75703125108393721, 13.14518615778179722 ) ) ;
#22045 = CARTESIAN_POINT ( 'NONE',  ( 102.4976396683250925, 102.3130555110000159, -52.52500000273119696 ) ) ;
#22046 = CARTESIAN_POINT ( 'NONE',  ( 5.444914386472302859, 36.83281250108392868, 13.14518615778179189 ) ) ;
#22047 = VECTOR ( 'NONE', #18825, 1000.000000000000000 ) ;
#22048 =( BOUNDED_CURVE ( )  B_SPLINE_CURVE ( 2, ( #20751, #25440, #18874, #1644, #5922, #23029, #3920, #12578, #8186 ),
 .UNSPECIFIED., .F., .F. ) 
 B_SPLINE_CURVE_WITH_KNOTS ( ( 3, 2, 2, 2, 3 ),
 ( 0.07142857142857149400, 0.08035714285714290472, 0.08928571428571430157, 0.09821428571428571230, 0.1071428571428571092 ),
 .UNSPECIFIED. ) 
 CURVE ( )  GEOMETRIC_REPRESENTATION_ITEM ( )  RATIONAL_B_SPLINE_CURVE ( ( 0.9999999999999994449, 0.9238795325112872936, 1.000000000000000000, 0.9238795325112867385, 1.000000000000000000, 0.9238795325112867385, 1.000000000000000000, 0.9238795325112869605, 0.9999999999999997780 ) ) 
 REPRESENTATION_ITEM ( '' )  );
#22049 = CARTESIAN_POINT ( 'NONE',  ( 0.000000000000000000, 40.99999999999999289, 0.000000000000000000 ) ) ;
#22050 = CARTESIAN_POINT ( 'NONE',  ( 99.99999999999995737, 1.387778780781445676E-14, 15.00000000000000000 ) ) ;
#22051 = CARTESIAN_POINT ( 'NONE',  ( 103.5355339059327093, 82.37500000000000000, 3.535533905932726206 ) ) ;
#22052 = CARTESIAN_POINT ( 'NONE',  ( 135.6228728715778971, 38.07304687499998863, 13.57481594606304576 ) ) ;
#22053 = EDGE_CURVE ( 'NONE', #138, #9928, #2157, .T. ) ;
#22054 = ORIENTED_EDGE ( 'NONE', *, *, #15930, .F. ) ;
#22055 = CARTESIAN_POINT ( 'NONE',  ( 95.67376207875072680, 104.0454443415356991, -56.19999999453762740 ) ) ;
#22056 = CARTESIAN_POINT ( 'NONE',  ( -13.14518615778179189, 37.62656250108393863, 5.444914386472304635 ) ) ;
#22057 = CARTESIAN_POINT ( 'NONE',  ( 5.622872871577878406, 35.79101562716787299, 13.57481594606304576 ) ) ;
#22058 = CARTESIAN_POINT ( 'NONE',  ( 103.5355339059327093, 3.535533905932755072, 7.750000002731185056 ) ) ;
#22059 = CARTESIAN_POINT ( 'NONE',  ( 143.1451861577818079, 36.18789062608393436, -1.609821015232357215E-15 ) ) ;
#22060 = CARTESIAN_POINT ( 'NONE',  ( 78.57481594606304043, 35.19570312716788152, -5.622872871577873077 ) ) ;
#22061 = EDGE_CURVE ( 'NONE', #18468, #25494, #6484, .T. ) ;
#22062 = VERTEX_POINT ( 'NONE', #1667 ) ;
#22063 = CARTESIAN_POINT ( 'NONE',  ( 8.193155644910682156, 35.99999999999998579, 10.45682415286346512 ) ) ;
#22064 = CARTESIAN_POINT ( 'NONE',  ( 13.57481594606304753, 32.81445312716787299, -5.622872871577873077 ) ) ;
#22065 = CARTESIAN_POINT ( 'NONE',  ( 94.99999999999995737, -2.071067811865466624, 3.062499999999999112 ) ) ;
#22066 = CARTESIAN_POINT ( 'NONE',  ( 102.4976396683250783, 117.6869444889999841, -48.47499999726882436 ) ) ;
#22067 = CIRCLE ( 'NONE', #24317, 1.000000000000000888 ) ;
#22068 = ADVANCED_FACE ( 'NONE', ( #28020 ), #10750, .F. ) ;
#22069 = CARTESIAN_POINT ( 'NONE',  ( 181.8548138422182205, 35.79101562608393294, 0.000000000000000000 ) ) ;
#22070 = ADVANCED_FACE ( 'NONE', ( #21603 ), #8765, .F. ) ;
#22071 = SURFACE_STYLE_USAGE ( .BOTH. , #17357 ) ;
#22072 = CARTESIAN_POINT ( 'NONE',  ( 0.000000000000000000, -7.395377635281828788, 0.000000000000000000 ) ) ;
#22073 = CARTESIAN_POINT ( 'NONE',  ( 130.0000000000000000, 36.13828125216787157, -13.57481594606304576 ) ) ;
#22074 = CARTESIAN_POINT ( 'NONE',  ( 97.83688103937537051, 103.3426043859339103, -48.09999999453764019 ) ) ;
#22075 = CARTESIAN_POINT ( 'NONE',  ( 5.622872871577878406, 36.48554687499999716, 13.57481594606304576 ) ) ;
#22076 = CARTESIAN_POINT ( 'NONE',  ( 95.67376207875072680, 115.9545556584642867, -45.30000000000000426 ) ) ;
#22077 = CARTESIAN_POINT ( 'NONE',  ( 2.414731522848535132E-15, 38.56914062608393579, 13.14518615778179544 ) ) ;
#22078 = CARTESIAN_POINT ( 'NONE',  ( -13.14518615778179544, 34.99726562608393721, 0.000000000000000000 ) ) ;
#22079 = CARTESIAN_POINT ( 'NONE',  ( 208.5748159460630120, 33.40976562499999858, 5.622872871577869525 ) ) ;
#22080 = CARTESIAN_POINT ( 'NONE',  ( 108.0825317500000011, 112.6261737610028320, -46.27500000273120406 ) ) ;
#22081 = DIRECTION ( 'NONE',  ( -0.000000000000000000, -1.000000000000000000, -0.000000000000000000 ) ) ;
#22082 = CARTESIAN_POINT ( 'NONE',  ( 59.55508561352770158, 34.84843750108393579, -13.14518615778179900 ) ) ;
#22083 = CARTESIAN_POINT ( 'NONE',  ( 104.4587341249999639, 1.442382525525748735E-14, 3.937500001365591640 ) ) ;
#22084 = CARTESIAN_POINT ( 'NONE',  ( 98.94657102337468757, 123.0000000000000284, -2.271811130025750192 ) ) ;
#22085 = CARTESIAN_POINT ( 'NONE',  ( 98.20479815727543382, 122.9999999999999432, -1.033452060272729067 ) ) ;
#22086 = CARTESIAN_POINT ( 'NONE',  ( -5.622872871577873077, 34.79882812499998579, 13.57481594606304753 ) ) ;
#22087 = CARTESIAN_POINT ( 'NONE',  ( 120.7049497278729575, 39.26367187608393294, 9.295050272127047819 ) ) ;
#22088 = ORIENTED_EDGE ( 'NONE', *, *, #21145, .T. ) ;
#22089 = CARTESIAN_POINT ( 'NONE',  ( 96.46446609406721961, 84.12500000000000000, 3.535533905932727539 ) ) ;
#22090 = VECTOR ( 'NONE', #16439, 1000.000000000000000 ) ;
#22091 = CARTESIAN_POINT ( 'NONE',  ( 195.0000000000000000, 36.93203125216787441, -13.57481594606304576 ) ) ;
#22092 = CARTESIAN_POINT ( 'NONE',  ( 103.5355339059327093, 81.50000000273119838, 3.535533905932726206 ) ) ;
#22093 = CARTESIAN_POINT ( 'NONE',  ( 104.4587341249999781, 93.31249999863440792, -6.938893903907228378E-15 ) ) ;
#22094 = CARTESIAN_POINT ( 'NONE',  ( 98.15313185440925281, 94.87499999863440792, -4.458734124999994997 ) ) ;
#22095 =( BOUNDED_CURVE ( )  B_SPLINE_CURVE ( 2, ( #7906, #14449, #25153, #21303, #23028, #3918, #27584, #16740, #1785 ),
 .UNSPECIFIED., .F., .F. ) 
 B_SPLINE_CURVE_WITH_KNOTS ( ( 3, 2, 2, 2, 3 ),
 ( 0.2708333333333330928, 0.2812499999999998890, 0.2916666666666666852, 0.3020833333333334259, 0.3125000000000002220 ),
 .UNSPECIFIED. ) 
 CURVE ( )  GEOMETRIC_REPRESENTATION_ITEM ( )  RATIONAL_B_SPLINE_CURVE ( ( 1.000000000000001554, 0.9238795325112850731, 1.000000000000000000, 0.9238795325112867385, 1.000000000000000000, 0.9238795325112867385, 1.000000000000000000, 0.9238795325112850731, 1.000000000000001554 ) ) 
 REPRESENTATION_ITEM ( '' )  );
#22096 = CARTESIAN_POINT ( 'NONE',  ( 102.1631189606246153, 116.6573956140660897, -49.60000000000001563 ) ) ;
#22097 = CARTESIAN_POINT ( 'NONE',  ( 78.57481594606305464, 40.60312499999999858, -1.662435489736055892E-15 ) ) ;
#22098 = ORIENTED_EDGE ( 'NONE', *, *, #1705, .T. ) ;
#22099 = CARTESIAN_POINT ( 'NONE',  ( 13.57481594606304576, 32.76484375216787015, -1.662435489736055892E-15 ) ) ;
#22100 = CARTESIAN_POINT ( 'NONE',  ( 99.99999999999995737, -4.999999999999990230, 14.24999999999999822 ) ) ;
#22101 = EDGE_CURVE ( 'NONE', #6975, #26723, #10470, .T. ) ;
#22102 = ORIENTED_EDGE ( 'NONE', *, *, #25973, .T. ) ;
#22103 = LINE ( 'NONE', #27200, #26161 ) ;
#22104 = CARTESIAN_POINT ( 'NONE',  ( -13.14518615778179544, 40.75195312608393294, 0.000000000000000000 ) ) ;
#22105 = CARTESIAN_POINT ( 'NONE',  ( 204.5988444088204687, 33.45937500216787441, 9.598844408820456309 ) ) ;
#22106 = CARTESIAN_POINT ( 'NONE',  ( -5.444914386472297529, 37.22968750108394431, -13.14518615778179722 ) ) ;
#22107 = CARTESIAN_POINT ( 'NONE',  ( 206.1048480505471048, 36.02027164848243501, -8.092840767093784748 ) ) ;
#22108 = CARTESIAN_POINT ( 'NONE',  ( 200.6228728715779539, 38.46992187716787726, -13.57481594606299247 ) ) ;
#22109 = CARTESIAN_POINT ( 'NONE',  ( 5.444914386472297529, 34.94765625108394147, -13.14518615778179900 ) ) ;
#22110 = CARTESIAN_POINT ( 'NONE',  ( 116.8548138422182205, 35.79101562608393294, 0.000000000000000000 ) ) ;
#22111 = CARTESIAN_POINT ( 'NONE',  ( 74.59884440882045453, 35.74140624999999716, 9.598844408820456309 ) ) ;
#22112 = CARTESIAN_POINT ( 'NONE',  ( 101.4615807364564546, 124.4500000010924765, -1.461580736456474794 ) ) ;
#22113 = CARTESIAN_POINT ( 'NONE',  ( 95.54126587499995082, 1.846868145590750077, 10.62500000136559208 ) ) ;
#22114 = CARTESIAN_POINT ( 'NONE',  ( 208.4955014123170827, 35.99999999999996447, -0.9550757908099977156 ) ) ;
#22115 = CARTESIAN_POINT ( 'NONE',  ( 95.54126587499996504, 1.846868145590750077, 14.37500000136559386 ) ) ;
#22116 = CARTESIAN_POINT ( 'NONE',  ( 91.91746824999998466, 107.3738262389971538, -47.02500000273118275 ) ) ;
#22117 = CARTESIAN_POINT ( 'NONE',  ( 102.4999999999999858, 123.7500000000000142, 1.035533905932722876 ) ) ;
#22118 = AXIS2_PLACEMENT_3D ( 'NONE', #5861, #14660, #12241 ) ;
#22119 = CARTESIAN_POINT ( 'NONE',  ( 99.99999999999995737, 83.37500000273119838, 4.999999999999990230 ) ) ;
#22120 = CARTESIAN_POINT ( 'NONE',  ( 108.0825317500000011, 110.0000000000000000, -46.62499999726882294 ) ) ;
#22121 = CARTESIAN_POINT ( 'NONE',  ( 13.14518615778179900, 37.13046875108393863, 5.444914386472293977 ) ) ;
#22122 = CARTESIAN_POINT ( 'NONE',  ( 102.1631189606246153, 116.6573956140660897, -47.09999999453764019 ) ) ;
#22123 = ORIENTED_EDGE ( 'NONE', *, *, #7781, .T. ) ;
#22124 = CARTESIAN_POINT ( 'NONE',  ( 94.99999999999995737, 1.387778780781445676E-14, 9.999999999999998224 ) ) ;
#22125 = CARTESIAN_POINT ( 'NONE',  ( 97.93301270000000613, 122.9000000010924794, -0.8561741729129506151 ) ) ;
#22126 = DIRECTION ( 'NONE',  ( -0.000000000000000000, 1.000000000000000000, -0.000000000000000000 ) ) ;
#22127 = CARTESIAN_POINT ( 'NONE',  ( 208.1451861577817795, 36.93203125108394147, 5.444914386472293977 ) ) ;
#22128 = ORIENTED_EDGE ( 'NONE', *, *, #4796, .T. ) ;
#22129 = CARTESIAN_POINT ( 'NONE',  ( 13.57481594606304576, 39.90859375216787441, -1.662435489736055892E-15 ) ) ;
#22130 = CARTESIAN_POINT ( 'NONE',  ( 98.15313185440925281, 4.458734125000016313, 11.50000000136559208 ) ) ;
#22131 = VERTEX_POINT ( 'NONE', #19597 ) ;
#22132 = CARTESIAN_POINT ( 'NONE',  ( 94.33688103937537051, 114.1144967660473242, -46.20000000000000284 ) ) ;
#22133 = CARTESIAN_POINT ( 'NONE',  ( 99.99999999999995737, 83.87500000273119838, -5.000000000000018652 ) ) ;
#22134 = CIRCLE ( 'NONE', #25765, 5.000000000000000000 ) ;
#22135 = CARTESIAN_POINT ( 'NONE',  ( 98.23223304703363112, 123.5000000000000000, 1.767766952966351557 ) ) ;
#22136 = CARTESIAN_POINT ( 'NONE',  ( 116.8548138422182205, 40.55351562608393579, 0.000000000000000000 ) ) ;
#22137 = CARTESIAN_POINT ( 'NONE',  ( 13.14518615778179722, 39.61093750108393863, -5.444914386472297529 ) ) ;
#22138 = CARTESIAN_POINT ( 'NONE',  ( 104.9999999999999716, 92.93749999726880162, -2.071067811865478170 ) ) ;
#22139 = CARTESIAN_POINT ( 'NONE',  ( 51.85481384221820633, 36.83281250108393579, 5.444914386472304635 ) ) ;
#22140 = CARTESIAN_POINT ( 'NONE',  ( 56.74038847111184936, 50.00000000056339644, -10.79618466885979799 ) ) ;
#22141 = CARTESIAN_POINT ( 'NONE',  ( 185.4011555911795597, 40.30546874999999574, 9.598844408820459861 ) ) ;
#22142 = CARTESIAN_POINT ( 'NONE',  ( 70.62287287157776916, 38.37070312499999858, -13.57481594606313990 ) ) ;
#22143 = VERTEX_POINT ( 'NONE', #12458 ) ;
#22144 = ORIENTED_EDGE ( 'NONE', *, *, #22680, .F. ) ;
#22145 = CARTESIAN_POINT ( 'NONE',  ( -5.444914386472299306, 36.93203125108394147, 13.14518615778179722 ) ) ;
#22146 = CARTESIAN_POINT ( 'NONE',  ( 101.8468681455907046, -4.458734124999987891, 13.00000000136559386 ) ) ;
#22147 = CYLINDRICAL_SURFACE ( 'NONE', #18056, 4.999999999999989342 ) ;
#22148 = CARTESIAN_POINT ( 'NONE',  ( 112.9999999999999858, 95.00000000000000000, 12.99999999999999289 ) ) ;
#22149 = CARTESIAN_POINT ( 'NONE',  ( 208.1451861577818079, 37.72578125108393010, 5.444914386472293977 ) ) ;
#22150 = ORIENTED_EDGE ( 'NONE', *, *, #14163, .F. ) ;
#22151 = CARTESIAN_POINT ( 'NONE',  ( 9.295050272127046043, 36.48554687608393721, -9.295050272127046043 ) ) ;
#22152 = ADVANCED_FACE ( 'NONE', ( #27743 ), #13838, .T. ) ;
#22153 = B_SPLINE_CURVE_WITH_KNOTS ( 'NONE', 3,
 ( #21794, #22214, #2693, #15349, #24065, #4541, #11354, #17642, #26349, #6808, #555, #27067, #9519, #25192, #7370, #7807, #3257, #20646, #18644, #25057, #16497, #1407, #3539, #12195, #18359, #5398, #22787, #18217, #22498, #14346, #12059 ),
 .UNSPECIFIED., .F., .F.,
 ( 4, 2, 2, 2, 2, 2, 2, 2, 2, 2, 1, 2, 2, 2, 2, 4 ),
 ( 0.000000000000000000, 0.001656255954913781435, 0.003312511909827562870, 0.004968767864741344305, 0.005796895842198234589, 0.006625023819655125740, 0.008281279774568908042, 0.009937535729482686875, 0.01325004763931025148, 0.01490630359422403031, 0.01656255954913780915, 0.01821881550405159145, 0.01987507145896537028, 0.02318758336879293835, 0.02484383932370672066, 0.02650009527862050296 ),
 .UNSPECIFIED. ) ;
#22154 = VECTOR ( 'NONE', #1281, 1000.000000000000000 ) ;
#22155 = CARTESIAN_POINT ( 'NONE',  ( 95.54126587500000767, 91.06249999863440792, -7.484931351350258973E-15 ) ) ;
#22156 = CARTESIAN_POINT ( 'NONE',  ( 185.7049497278729575, 39.06523437608392868, -9.295050272127046043 ) ) ;
#22157 = CARTESIAN_POINT ( 'NONE',  ( 91.91746824999997045, 107.3738262389971538, -53.52499999726882862 ) ) ;
#22158 = ORIENTED_EDGE ( 'NONE', *, *, #20853, .T. ) ;
#22159 = CARTESIAN_POINT ( 'NONE',  ( -13.57481594606304753, 36.98164062499999005, -5.622872871577873077 ) ) ;
#22160 = CARTESIAN_POINT ( 'NONE',  ( -13.14518615778179900, 37.32890625108393579, -5.444914386472297529 ) ) ;
#22161 = ORIENTED_EDGE ( 'NONE', *, *, #23487, .F. ) ;
#22162 = CARTESIAN_POINT ( 'NONE',  ( 143.1451861577818079, 33.95546875108393436, 5.444914386472293977 ) ) ;
#22163 = CARTESIAN_POINT ( 'NONE',  ( 78.14518615778179367, 33.85625000108393579, -5.444914386472297529 ) ) ;
#22164 = CARTESIAN_POINT ( 'NONE',  ( 200.4449143864723055, 37.32890625108393579, -13.14518615778179900 ) ) ;
#22165 = ORIENTED_EDGE ( 'NONE', *, *, #2181, .T. ) ;
#22166 = CARTESIAN_POINT ( 'NONE',  ( 101.4615807364564546, 124.2500000010924879, -1.461580736456474794 ) ) ;
#22167 = CARTESIAN_POINT ( 'NONE',  ( 5.444914386472297529, 33.95546875108393436, -13.14518615778179900 ) ) ;
#22168 = CARTESIAN_POINT ( 'NONE',  ( 101.0355339059327235, 123.7500000021849615, 2.499999999999987121 ) ) ;
#22169 = CIRCLE ( 'NONE', #14419, 23.26794919243112858 ) ;
#22170 = CARTESIAN_POINT ( 'NONE',  ( 116.4251840539369596, 39.56132812716787583, 5.622872871577880183 ) ) ;
#22171 = DIRECTION ( 'NONE',  ( -0.000000000000000000, -1.000000000000000000, -0.000000000000000000 ) ) ;
#22172 = DIRECTION ( 'NONE',  ( -1.000000000000000000, 0.000000000000000000, 0.000000000000000000 ) ) ;
#22173 = CARTESIAN_POINT ( 'NONE',  ( 130.0000000000000000, 38.02343749999999289, 13.57481594606304576 ) ) ;
#22174 = CARTESIAN_POINT ( 'NONE',  ( 200.4449143864723055, 39.71015625108393010, -13.14518615778179900 ) ) ;
#22175 = VERTEX_POINT ( 'NONE', #22707 ) ;
#22176 = CARTESIAN_POINT ( 'NONE',  ( 101.8468681455906903, -4.458734124999987891, 6.750000001365592972 ) ) ;
#22177 = ORIENTED_EDGE ( 'NONE', *, *, #13399, .T. ) ;
#22178 = CARTESIAN_POINT ( 'NONE',  ( 102.4999999999999716, 123.1500000021849672, -1.035533905932742638 ) ) ;
#22179 = CARTESIAN_POINT ( 'NONE',  ( 99.99999999999995737, -4.458734124999988779, 7.687500001365592084 ) ) ;
#22180 = CARTESIAN_POINT ( 'NONE',  ( 104.9999999999999716, 1.449011120738813565E-14, 8.499999999999998224 ) ) ;
#22181 = CARTESIAN_POINT ( 'NONE',  ( -9.295050272127046043, 36.48554687608393721, -9.295050272127046043 ) ) ;
#22182 = CARTESIAN_POINT ( 'NONE',  ( 65.00000000000000000, 39.31328125216787583, -13.57481594606304576 ) ) ;
#22183 = CARTESIAN_POINT ( 'NONE',  ( 96.84719886470459471, 81.56250000136559208, -3.152801135295383084 ) ) ;
#22184 = CARTESIAN_POINT ( 'NONE',  ( 51.85481384221820633, 35.98945312608393721, 0.000000000000000000 ) ) ;
#22185 = CARTESIAN_POINT ( 'NONE',  ( 106.5389055433251002, 105.2492070361643215, -44.32500000273119412 ) ) ;
#22186 = CARTESIAN_POINT ( 'NONE',  ( -8.049105076161786076E-16, 38.76757812608393294, -13.14518615778179544 ) ) ;
#22187 = CARTESIAN_POINT ( 'NONE',  ( 9.598844408820456309, 35.24531250216787726, -9.598844408820458085 ) ) ;
#22188 = CARTESIAN_POINT ( 'NONE',  ( -6.902378573780346471, 51.13402819306926261, 15.00000000000000178 ) ) ;
#22189 = CARTESIAN_POINT ( 'NONE',  ( 92.99999999999998579, 112.2744378736303190, -54.59999999453764019 ) ) ;
#22190 = CARTESIAN_POINT ( 'NONE',  ( 139.5988444088204403, 36.73359374999999716, -9.598844408820458085 ) ) ;
#22191 = VERTEX_POINT ( 'NONE', #761 ) ;
#22192 = ORIENTED_EDGE ( 'NONE', *, *, #21750, .F. ) ;
#22193 = PLANE ( 'NONE',  #14480 ) ;
#22194 = ADVANCED_FACE ( 'NONE', ( #11026 ), #13480, .F. ) ;
#22195 = CARTESIAN_POINT ( 'NONE',  ( 9.295050272127046043, 37.27929687608394005, -9.295050272127046043 ) ) ;
#22196 = CARTESIAN_POINT ( 'NONE',  ( -13.57481594606304576, 38.71796875216787726, 0.000000000000000000 ) ) ;
#22197 = CARTESIAN_POINT ( 'NONE',  ( 94.99999999999995737, 2.071067811865491048, 9.062500002731184168 ) ) ;
#22198 = CARTESIAN_POINT ( 'NONE',  ( 130.0000000000000000, 32.41757812608393863, -13.14518615778179544 ) ) ;
#22199 = CARTESIAN_POINT ( 'NONE',  ( 55.40115559117954547, 34.84843750216787583, 9.598844408820459861 ) ) ;
#22200 = ORIENTED_EDGE ( 'NONE', *, *, #4590, .F. ) ;
#22201 = CARTESIAN_POINT ( 'NONE',  ( 9.432006169634068016, 36.00000000000000711, 9.391769196590193047 ) ) ;
#22202 = CARTESIAN_POINT ( 'NONE',  ( -13.57481594606304576, 33.16171875216787868, 0.000000000000000000 ) ) ;
#22203 = CARTESIAN_POINT ( 'NONE',  ( 96.46446609406721961, 3.535533905932755072, 2.874999999999999112 ) ) ;
#22204 = CARTESIAN_POINT ( 'NONE',  ( -15.00000000000000000, 55.00000000000000000, 15.00000000000000178 ) ) ;
#22205 = CARTESIAN_POINT ( 'NONE',  ( -5.622872871577873077, 37.77539062716788010, -13.57481594606304753 ) ) ;
#22206 = CARTESIAN_POINT ( 'NONE',  ( 208.1451861577817795, 33.06250000108393294, -5.444914386472297529 ) ) ;
#22207 = CARTESIAN_POINT ( 'NONE',  ( -20.00000000000000000, 75.00000000000000000, 10.00000000000000000 ) ) ;
#22208 = DIRECTION ( 'NONE',  ( 0.000000000000000000, 0.000000000000000000, -1.000000000000000000 ) ) ;
#22209 = CARTESIAN_POINT ( 'NONE',  ( 9.598844408820459861, 34.25312500216787015, 9.598844408820456309 ) ) ;
#22210 = CARTESIAN_POINT ( 'NONE',  ( 95.00000000000000000, 94.31249999726880162, -2.071067811865479058 ) ) ;
#22211 = CYLINDRICAL_SURFACE ( 'NONE', #17691, 5.000000000000004441 ) ;
#22212 = CARTESIAN_POINT ( 'NONE',  ( 101.0355339059327235, 123.2500000021849615, -2.499999999999998668 ) ) ;
#22213 = CARTESIAN_POINT ( 'NONE',  ( 2.493653234604083739E-15, 36.43593749999999432, 13.57481594606304576 ) ) ;
#22214 = CARTESIAN_POINT ( 'NONE',  ( 3.628614293284873948, 36.00000000000000711, -13.08307257738123219 ) ) ;
#22215 =( BOUNDED_CURVE ( )  B_SPLINE_CURVE ( 2, ( #26448, #8907, #9054, #366, #11452, #13158, #26592, #17886, #222 ),
 .UNSPECIFIED., .F., .F. ) 
 B_SPLINE_CURVE_WITH_KNOTS ( ( 3, 2, 2, 2, 3 ),
 ( 0.02083333333333358892, 0.03125000000000020123, 0.04166666666666681007, 0.05208333333333342585, 0.06250000000000004163 ),
 .UNSPECIFIED. ) 
 CURVE ( )  GEOMETRIC_REPRESENTATION_ITEM ( )  RATIONAL_B_SPLINE_CURVE ( ( 0.9999999999999981126, 0.9238795325112886259, 1.000000000000000000, 0.9238795325112867385, 1.000000000000000000, 0.9238795325112867385, 1.000000000000000000, 0.9238795325112864054, 1.000000000000000222 ) ) 
 REPRESENTATION_ITEM ( '' )  );
#22216 = CARTESIAN_POINT ( 'NONE',  ( 13.14518615778179900, 33.16171875108393863, 5.444914386472293977 ) ) ;
#22217 = CARTESIAN_POINT ( 'NONE',  ( -9.295050272127046043, 35.69179687608393436, -9.295050272127046043 ) ) ;
#22218 = CARTESIAN_POINT ( 'NONE',  ( 181.4251840539369596, 34.64999999999999147, 0.000000000000000000 ) ) ;
#22219 = CARTESIAN_POINT ( 'NONE',  ( -8.312177448680279460E-16, 36.13828125216787157, -13.57481594606304576 ) ) ;
#22220 = CARTESIAN_POINT ( 'NONE',  ( 9.598844408820456309, 37.62656250216787157, -9.598844408820458085 ) ) ;
#22221 = CARTESIAN_POINT ( 'NONE',  ( 135.6228728715780107, 36.78320312499999289, -13.57481594606290898 ) ) ;
#22222 = CARTESIAN_POINT ( 'NONE',  ( 74.29505027212704249, 36.88242187608393152, 9.295050272127046043 ) ) ;
#22223 = CARTESIAN_POINT ( 'NONE',  ( 98.15313185440923860, -4.458734124999987891, 3.625000001365591196 ) ) ;
#22224 = CARTESIAN_POINT ( 'NONE',  ( 99.08087592991887504, 123.0000000000000426, -2.329274081706632415 ) ) ;
#22225 = ORIENTED_EDGE ( 'NONE', *, *, #5935, .T. ) ;
#22226 = EDGE_CURVE ( 'NONE', #21433, #21442, #22563, .T. ) ;
#22227 = CARTESIAN_POINT ( 'NONE',  ( 99.99999999999998579, 123.6000000000000085, 2.499999999999978684 ) ) ;
#22228 = CARTESIAN_POINT ( 'NONE',  ( 5.622872871577878406, 36.48554687499999716, 13.57481594606304576 ) ) ;
#22229 = CARTESIAN_POINT ( 'NONE',  ( 143.1451861577818079, 37.97382812608393721, -1.609821015232357215E-15 ) ) ;
#22230 = ORIENTED_EDGE ( 'NONE', *, *, #8596, .F. ) ;
#22231 = CARTESIAN_POINT ( 'NONE',  ( 95.67376207875072680, 115.9545556584642867, -50.30000000000000426 ) ) ;
#22232 = CARTESIAN_POINT ( 'NONE',  ( 87.00000000000000000, 102.0000000000000000, -43.00000000000000000 ) ) ;
#22233 = CARTESIAN_POINT ( 'NONE',  ( 96.46446609406721961, 83.25000000273119838, 3.535533905932727539 ) ) ;
#22234 = CARTESIAN_POINT ( 'NONE',  ( 102.0710678118654613, 91.81250000000000000, 4.999999999999983125 ) ) ;
#22235 = CARTESIAN_POINT ( 'NONE',  ( 96.84719886470463734, 94.93749999863440792, -3.152801135295366208 ) ) ;
#22236 = ADVANCED_FACE ( 'NONE', ( #13157 ), #16129, .T. ) ;
#22237 = AXIS2_PLACEMENT_3D ( 'NONE', #14908, #23629, #15331 ) ;
#22238 = CARTESIAN_POINT ( 'NONE',  ( 105.6631189606246153, 114.1144967660473242, -49.80000000000001137 ) ) ;
#22239 = CARTESIAN_POINT ( 'NONE',  ( 70.62287287157786864, 39.95820312499999716, -13.57481594606304753 ) ) ;
#22240 = ORIENTED_EDGE ( 'NONE', *, *, #1482, .F. ) ;
#22241 = CARTESIAN_POINT ( 'NONE',  ( 0.000000000000000000, 29.95886589889650509, 0.000000000000000000 ) ) ;
#22242 = CARTESIAN_POINT ( 'NONE',  ( 104.9999999999999574, -2.071067811865462627, 12.43750000000000000 ) ) ;
#22243 = EDGE_CURVE ( 'NONE', #20676, #16151, #9579, .T. ) ;
#22244 = VERTEX_POINT ( 'NONE', #11847 ) ;
#22245 = CARTESIAN_POINT ( 'NONE',  ( 2.414731522848535132E-15, 36.98164062608393721, 13.14518615778179544 ) ) ;
#22246 = CARTESIAN_POINT ( 'NONE',  ( 181.4251840539369596, 34.74921875216787726, 0.000000000000000000 ) ) ;
#22247 = VERTEX_POINT ( 'NONE', #20569 ) ;
#22248 = CARTESIAN_POINT ( 'NONE',  ( -9.295050272127046043, 33.31054687608393294, -9.295050272127046043 ) ) ;
#22249 = DIRECTION ( 'NONE',  ( 0.000000000000000000, 1.000000000000000000, 0.000000000000000000 ) ) ;
#22250 = CARTESIAN_POINT ( 'NONE',  ( 139.2950502721270425, 37.08085937608393579, 9.295050272127046043 ) ) ;
#22251 = CARTESIAN_POINT ( 'NONE',  ( 13.14518615778179900, 34.74921875108395142, 5.444914386472293977 ) ) ;
#22252 = CARTESIAN_POINT ( 'NONE',  ( 143.1451861577818079, 33.06250000108393294, -5.444914386472297529 ) ) ;
#22253 = CARTESIAN_POINT ( 'NONE',  ( 74.59884440882045453, 33.36015624999999574, 9.598844408820456309 ) ) ;
#22254 = CARTESIAN_POINT ( 'NONE',  ( 102.0710678118654329, 92.18749999999998579, -5.000000000000023093 ) ) ;
#22255 = CIRCLE ( 'NONE', #17229, 13.57481594606304398 ) ;
#22256 = VECTOR ( 'NONE', #20102, 1000.000000000000000 ) ;
#22257 = CARTESIAN_POINT ( 'NONE',  ( 98.15313185440925281, -4.458734124999987891, 11.87500000136559031 ) ) ;
#22258 = LINE ( 'NONE', #8995, #23991 ) ;
#22259 = CARTESIAN_POINT ( 'NONE',  ( 104.4587341249999781, -1.846868145590721655, 0.8750000013655926390 ) ) ;
#22260 = CARTESIAN_POINT ( 'NONE',  ( 108.0825317500000011, 112.6261737610028320, -48.02500000273118985 ) ) ;
#22261 = VECTOR ( 'NONE', #23154, 1000.000000000000227 ) ;
#22262 = CARTESIAN_POINT ( 'NONE',  ( 95.54126587500000767, 91.06249999863440792, -7.484931351350258973E-15 ) ) ;
#22263 = CARTESIAN_POINT ( 'NONE',  ( 181.4251840539369596, 40.99999999999999289, 0.000000000000000000 ) ) ;
#22264 = CARTESIAN_POINT ( 'NONE',  ( 108.0825317499999869, 112.6261737610028320, -50.52499999726881441 ) ) ;
#22265 = CARTESIAN_POINT ( 'NONE',  ( -9.295050272127044266, 36.88242187608393152, 9.295050272127047819 ) ) ;
#22266 = CARTESIAN_POINT ( 'NONE',  ( 92.99999999999998579, 110.0000000000000000, -46.49999999453763877 ) ) ;
#22267 = ORIENTED_EDGE ( 'NONE', *, *, #1710, .F. ) ;
#22268 = FACE_OUTER_BOUND ( 'NONE', #4854, .T. ) ;
#22269 =( BOUNDED_CURVE ( )  B_SPLINE_CURVE ( 2, ( #23188, #23461, #27742, #19031, #12326, #10469, #5135, #25591, #11664 ),
 .UNSPECIFIED., .F., .T. ) 
 B_SPLINE_CURVE_WITH_KNOTS ( ( 3, 2, 2, 2, 3 ),
 ( 0.3214285714285713969, 0.3303571428571427937, 0.3392857142857143016, 0.3482142857142856984, 0.3571428571428572063 ),
 .UNSPECIFIED. ) 
 CURVE ( )  GEOMETRIC_REPRESENTATION_ITEM ( )  RATIONAL_B_SPLINE_CURVE ( ( 1.000000000000000444, 0.9238795325112862944, 1.000000000000000000, 0.9238795325112867385, 1.000000000000000000, 0.9238795325112867385, 1.000000000000000000, 0.9238795325112862944, 1.000000000000000444 ) ) 
 REPRESENTATION_ITEM ( '' )  );
#22270 = CARTESIAN_POINT ( 'NONE',  ( 0.000000000000000000, 23.00000000000000000, 25.00000000000001066 ) ) ;
#22271 = CARTESIAN_POINT ( 'NONE',  ( 98.96446609406724804, 123.3500000021849274, -2.499999999999996447 ) ) ;
#22272 = EDGE_CURVE ( 'NONE', #2621, #20557, #17624, .T. ) ;
#22273 = CARTESIAN_POINT ( 'NONE',  ( 195.0000000000000000, 35.19570312608392726, 13.14518615778179544 ) ) ;
#22274 = VERTEX_POINT ( 'NONE', #19882 ) ;
#22275 = CARTESIAN_POINT ( 'NONE',  ( 194.6752756888038505, 53.49346745874645137, -14.99999999999999822 ) ) ;
#22276 = CARTESIAN_POINT ( 'NONE',  ( 104.4587341249999781, -1.846868145590721655, 9.125000001365592084 ) ) ;
#22277 = ORIENTED_EDGE ( 'NONE', *, *, #10019, .F. ) ;
#22278 = CARTESIAN_POINT ( 'NONE',  ( 97.50236033167492167, 117.6869444889999841, -53.77500000273119696 ) ) ;
#22279 = CARTESIAN_POINT ( 'NONE',  ( 13.14518615778179544, 35.39414062608393152, -1.609821015232357215E-15 ) ) ;
#22280 = CARTESIAN_POINT ( 'NONE',  ( 98.23223304703363112, 124.8999999999999915, -1.767766952966370209 ) ) ;
#22281 = CARTESIAN_POINT ( 'NONE',  ( 124.5550856135277087, 39.61093750108393152, -13.14518615778179900 ) ) ;
#22282 = LINE ( 'NONE', #2472, #14343 ) ;
#22283 = CARTESIAN_POINT ( 'NONE',  ( 2.414731522848535132E-15, 35.98945312608393010, 13.14518615778179544 ) ) ;
#22284 = CARTESIAN_POINT ( 'NONE',  ( 99.99999999999998579, 94.62499999726881583, 4.999999999999984013 ) ) ;
#22285 = CARTESIAN_POINT ( 'NONE',  ( 51.85481384221820633, 37.62656250108393863, 5.444914386472304635 ) ) ;
#22286 = CARTESIAN_POINT ( 'NONE',  ( 56.60406125870027694, 54.99999999495823033, -15.00000000000000000 ) ) ;
#22287 = CARTESIAN_POINT ( 'NONE',  ( 95.00472066334981491, 116.8754121666685393, -49.67500000273119554 ) ) ;
#22288 = CARTESIAN_POINT ( 'NONE',  ( 189.3771271284221314, 39.56132812499999574, 13.57481594606304753 ) ) ;
#22289 = CARTESIAN_POINT ( 'NONE',  ( 99.99999999999995737, 85.00000000000000000, -1.387778780781445676E-14 ) ) ;
#22290 = CARTESIAN_POINT ( 'NONE',  ( 13.14518615778179900, 35.54296875108394715, 5.444914386472293977 ) ) ;
#22291 = CARTESIAN_POINT ( 'NONE',  ( 95.54126587499996504, 1.846868145590750077, 6.625000001365592084 ) ) ;
#22292 = CARTESIAN_POINT ( 'NONE',  ( 70.44491438647229131, 36.83281250108392868, 13.14518615778179189 ) ) ;
#22293 = CYLINDRICAL_SURFACE ( 'NONE', #1976, 13.57481594606304398 ) ;
#22294 = CARTESIAN_POINT ( 'NONE',  ( 185.7049497278729575, 36.68398437608392726, 9.295050272127047819 ) ) ;
#22295 = ORIENTED_EDGE ( 'NONE', *, *, #10321, .F. ) ;
#22296 = CARTESIAN_POINT ( 'NONE',  ( -9.295050272127044266, 36.88242187608393152, 9.295050272127047819 ) ) ;
#22297 = CARTESIAN_POINT ( 'NONE',  ( 95.54126587499999346, 91.12499999863439371, 1.846868145590722543 ) ) ;
#22298 = CONICAL_SURFACE ( 'NONE', #8632, 25.00000000000000711, 0.5235987755983000369 ) ;
#22299 = CARTESIAN_POINT ( 'NONE',  ( 195.0000000000000000, 37.37851562608393863, -13.14518615778179544 ) ) ;
#22300 = CARTESIAN_POINT ( 'NONE',  ( 91.91746824999997045, 112.6261737610028320, -49.97499999726881725 ) ) ;
#22301 = VERTEX_POINT ( 'NONE', #24836 ) ;
#22302 = CARTESIAN_POINT ( 'NONE',  ( 13.57481594606304753, 32.71523437500000142, -5.622872871577873077 ) ) ;
#22303 = CARTESIAN_POINT ( 'NONE',  ( 9.295050272127046043, 35.49335937608393010, -9.295050272127046043 ) ) ;
#22304 = ORIENTED_EDGE ( 'NONE', *, *, #11675, .F. ) ;
#22305 = CARTESIAN_POINT ( 'NONE',  ( 143.1451861577818079, 33.21132812608393436, -1.609821015232357215E-15 ) ) ;
#22306 = CARTESIAN_POINT ( 'NONE',  ( 74.29505027212704249, 40.25585937608393294, 9.295050272127046043 ) ) ;
#22307 = VECTOR ( 'NONE', #12861, 1000.000000000000000 ) ;
#22308 = CARTESIAN_POINT ( 'NONE',  ( 181.8548138422182205, 34.40195312608393152, 0.000000000000000000 ) ) ;
#22309 = ORIENTED_EDGE ( 'NONE', *, *, #10510, .T. ) ;
#22310 = CARTESIAN_POINT ( 'NONE',  ( 94.99999999999995737, -2.071067811865466624, 13.06250000000000000 ) ) ;
#22311 = CARTESIAN_POINT ( 'NONE',  ( -5.444914386472299306, 31.97109375108393436, 13.14518615778179722 ) ) ;
#22312 = CARTESIAN_POINT ( 'NONE',  ( -13.36000105192242060, 40.87597656304196647, 0.000000000000000000 ) ) ;
#22313 = DIRECTION ( 'NONE',  ( -0.000000000000000000, -0.000000000000000000, -1.000000000000000000 ) ) ;
#22314 = CARTESIAN_POINT ( 'NONE',  ( 108.0825317500000153, 110.0000000000000000, -50.12500000273119127 ) ) ;
#22315 = ADVANCED_FACE ( 'NONE', ( #11987 ), #7294, .F. ) ;
#22316 = FACE_OUTER_BOUND ( 'NONE', #14051, .T. ) ;
#22317 = LINE ( 'NONE', #7182, #516 ) ;
#22318 = CARTESIAN_POINT ( 'NONE',  ( 200.4449143864723055, 40.50390625108394005, -13.14518615778179900 ) ) ;
#22319 = VECTOR ( 'NONE', #20655, 1000.000000000000227 ) ;
#22320 = ORIENTED_EDGE ( 'NONE', *, *, #3063, .F. ) ;
#22321 = CARTESIAN_POINT ( 'NONE',  ( 95.54126587499995082, -1.846868145590724986, 5.500000001365591196 ) ) ;
#22322 = ORIENTED_EDGE ( 'NONE', *, *, #23440, .T. ) ;
#22323 = CARTESIAN_POINT ( 'NONE',  ( 99.99999999999998579, 123.1500000010924794, 2.066987299999980099 ) ) ;
#22324 = CARTESIAN_POINT ( 'NONE',  ( 95.54126587499995082, -1.846868145590724986, 6.500000001365592084 ) ) ;
#22325 = CARTESIAN_POINT ( 'NONE',  ( 139.1801758136480203, 50.00000000000000000, 14.99999999999996980 ) ) ;
#22326 = CARTESIAN_POINT ( 'NONE',  ( 13.14518615778179544, 36.98164062608393010, -1.609821015232357215E-15 ) ) ;
#22327 = CARTESIAN_POINT ( 'NONE',  ( 195.0000000000000000, 40.00781250000000000, -13.57481594606304576 ) ) ;
#22328 = CARTESIAN_POINT ( 'NONE',  ( 70.62287287157778337, 37.37851562716787157, 13.57481594606313813 ) ) ;
#22329 = CARTESIAN_POINT ( 'NONE',  ( 98.15313185440925281, 92.99999999863439371, 4.458734124999979898 ) ) ;
#22330 = CARTESIAN_POINT ( 'NONE',  ( 108.0825317500000011, 107.3738262389971538, -46.22500000273118559 ) ) ;
#22332 = CARTESIAN_POINT ( 'NONE',  ( 13.14518615778179722, 38.51953125108393294, 5.444914386472293977 ) ) ;
#22331 = VECTOR ( 'NONE', #12464, 999.9999999999998863 ) ;
#22333 = LINE ( 'NONE', #11893, #5745 ) ;
#22334 = CARTESIAN_POINT ( 'NONE',  ( 0.9830651850993362695, 49.99999999949037033, 13.54930971656776073 ) ) ;
#22335 = CARTESIAN_POINT ( 'NONE',  ( 104.9999999999999858, 90.87499999726880162, -6.938893903907228378E-15 ) ) ;
#22336 = CARTESIAN_POINT ( 'NONE',  ( 116.4251840539369596, 36.28710937499999289, 5.622872871577880183 ) ) ;
#22337 = VERTEX_POINT ( 'NONE', #4640 ) ;
#22338 = CARTESIAN_POINT ( 'NONE',  ( -8.312177448680279460E-16, 33.65781249999999147, -13.57481594606304576 ) ) ;
#22339 = CARTESIAN_POINT ( 'NONE',  ( -13.14518615778179900, 33.55859375108393294, -5.444914386472297529 ) ) ;
#22340 = CARTESIAN_POINT ( 'NONE',  ( -5.622872871577873077, 35.69179687716786731, 13.57481594606304753 ) ) ;
#22341 = CARTESIAN_POINT ( 'NONE',  ( 102.0710678118654329, 5.000000000000018652, 10.81250000273118417 ) ) ;
#22342 = CARTESIAN_POINT ( 'NONE',  ( 116.8548138422182063, 34.15390625108393863, -5.444914386472297529 ) ) ;
#22343 = CARTESIAN_POINT ( 'NONE',  ( 51.85481384221820633, 39.80937500108392868, 5.444914386472304635 ) ) ;
#22344 = DIRECTION ( 'NONE',  ( 1.000000000000000000, 0.000000000000000000, 0.000000000000000000 ) ) ;
#22345 = CARTESIAN_POINT ( 'NONE',  ( -9.598844408820458085, 33.06250000216787299, -9.598844408820458085 ) ) ;
#22346 = DIRECTION ( 'NONE',  ( 0.000000000000000000, 1.000000000000000000, 0.000000000000000000 ) ) ;
#22347 = CARTESIAN_POINT ( 'NONE',  ( 91.91746824999997045, 112.6261737610028320, -45.97499999726882436 ) ) ;
#22348 = CARTESIAN_POINT ( 'NONE',  ( -13.57481594606304576, 39.51171875216787299, 0.000000000000000000 ) ) ;
#22349 = CARTESIAN_POINT ( 'NONE',  ( 208.1451861577817795, 34.55078125108393294, 5.444914386472293977 ) ) ;
#22350 = CYLINDRICAL_SURFACE ( 'NONE', #19219, 13.57481594606304576 ) ;
#22351 = CARTESIAN_POINT ( 'NONE',  ( 208.5748159460630688, 39.06523437499999574, -5.622872871577873966 ) ) ;
#22352 = DIRECTION ( 'NONE',  ( -0.000000000000000000, 1.000000000000000000, -0.000000000000000000 ) ) ;
#22353 = CARTESIAN_POINT ( 'NONE',  ( 5.622872871577878406, 35.69179687499999432, 13.57481594606304576 ) ) ;
#22354 = CARTESIAN_POINT ( 'NONE',  ( 130.0000000000000000, 38.42031249999999432, -13.57481594606304576 ) ) ;
#22355 = CARTESIAN_POINT ( 'NONE',  ( -13.14518615778179900, 34.35234375108393579, -5.444914386472297529 ) ) ;
#22356 = CARTESIAN_POINT ( 'NONE',  ( -9.295050272127046043, 34.89804687608393152, -9.295050272127046043 ) ) ;
#22357 = CARTESIAN_POINT ( 'NONE',  ( 2.414731522848535132E-15, 35.98945312608393010, 13.14518615778179544 ) ) ;
#22358 = AXIS2_PLACEMENT_3D ( 'NONE', #7082, #15780, #24485 ) ;
#22359 = CARTESIAN_POINT ( 'NONE',  ( 5.622872871577871301, 35.29492187716788720, -13.57481594606304753 ) ) ;
#22360 = CARTESIAN_POINT ( 'NONE',  ( 13.57481594606304931, 36.58476562499999574, 5.622872871577868636 ) ) ;
#22361 = CARTESIAN_POINT ( 'NONE',  ( 101.8468681455906903, 82.12500000136560629, -4.458734125000016313 ) ) ;
#22362 = CARTESIAN_POINT ( 'NONE',  ( 65.00000000000000000, 34.40195312608393152, 13.14518615778179544 ) ) ;
#22363 = CARTESIAN_POINT ( 'NONE',  ( 97.50236033167492167, 102.3130555110000159, -52.97500000273119980 ) ) ;
#22364 = CARTESIAN_POINT ( 'NONE',  ( 195.0000000000000000, -7.395377635281828788, 13.57481594606302266 ) ) ;
#22365 = ORIENTED_EDGE ( 'NONE', *, *, #12527, .T. ) ;
#22366 = FACE_OUTER_BOUND ( 'NONE', #14404, .T. ) ;
#22367 = CARTESIAN_POINT ( 'NONE',  ( -5.622872871577873077, 32.41757812499999858, 13.57481594606304753 ) ) ;
#22368 = CARTESIAN_POINT ( 'NONE',  ( 124.5550856135277087, 36.93203125108394147, 13.14518615778179722 ) ) ;
#22369 = VERTEX_POINT ( 'NONE', #26846 ) ;
#22370 = CARTESIAN_POINT ( 'NONE',  ( 106.9999999999999858, 112.2744378736303617, -50.90000000000000568 ) ) ;
#22371 = CARTESIAN_POINT ( 'NONE',  ( 9.598844408820459861, 34.94765624999999432, 9.598844408820456309 ) ) ;
#22372 = CARTESIAN_POINT ( 'NONE',  ( 94.99999999999995737, 83.12500000273119838, -1.387778780781445676E-14 ) ) ;
#22373 = CARTESIAN_POINT ( 'NONE',  ( 104.9999999999999858, 92.00000000000000000, -6.938893903907228378E-15 ) ) ;
#22374 = DIRECTION ( 'NONE',  ( -0.000000000000000000, 1.000000000000000000, -0.000000000000000000 ) ) ;
#22375 = EDGE_CURVE ( 'NONE', #16116, #25435, #10704, .T. ) ;
#22376 = CARTESIAN_POINT ( 'NONE',  ( 106.5389055433250860, 105.2492070361643215, -46.82499999726881867 ) ) ;
#22377 = CARTESIAN_POINT ( 'NONE',  ( 74.29505027212704249, 32.51679687608393721, -9.295050272127046043 ) ) ;
#22378 = ORIENTED_EDGE ( 'NONE', *, *, #8261, .T. ) ;
#22379 = DIRECTION ( 'NONE',  ( 0.000000000000000000, 0.000000000000000000, 1.000000000000000000 ) ) ;
#22380 = CARTESIAN_POINT ( 'NONE',  ( 102.0710678118654329, -4.999999999999989342, 13.31250000000000000 ) ) ;
#22381 = ORIENTED_EDGE ( 'NONE', *, *, #11040, .F. ) ;
#22382 = CARTESIAN_POINT ( 'NONE',  ( 2.414731522848535132E-15, 36.18789062608393436, 13.14518615778179544 ) ) ;
#22383 = CARTESIAN_POINT ( 'NONE',  ( 185.4011555911795597, 34.84843750216787583, 9.598844408820459861 ) ) ;
#22384 =( BOUNDED_CURVE ( )  B_SPLINE_CURVE ( 2, ( #4676, #26914, #7359, #18055, #544, #26771, #15633, #13338, #2543 ),
 .UNSPECIFIED., .F., .F. ) 
 B_SPLINE_CURVE_WITH_KNOTS ( ( 3, 2, 2, 2, 3 ),
 ( 0.08333333333333307891, 0.1249999999999999167, 0.1666666666666667407, 0.2083333333333335924, 0.2500000000000004441 ),
 .UNSPECIFIED. ) 
 CURVE ( )  GEOMETRIC_REPRESENTATION_ITEM ( )  RATIONAL_B_SPLINE_CURVE ( ( 1.000000000000000444, 0.9238795325112862944, 1.000000000000000000, 0.9238795325112867385, 1.000000000000000000, 0.9238795325112867385, 1.000000000000000000, 0.9238795325112859613, 1.000000000000000888 ) ) 
 REPRESENTATION_ITEM ( '' )  );
#22385 = EDGE_CURVE ( 'NONE', #15812, #15410, #8041, .T. ) ;
#22386 = CARTESIAN_POINT ( 'NONE',  ( 2.414731522848535132E-15, 32.02070312608393010, 13.14518615778179544 ) ) ;
#22387 = DIRECTION ( 'NONE',  ( -1.000000000000000000, 0.000000000000000000, 0.000000000000000000 ) ) ;
#22388 = CARTESIAN_POINT ( 'NONE',  ( 208.5748159460630688, 38.27148437716787299, 5.622872871577868636 ) ) ;
#22389 = CARTESIAN_POINT ( 'NONE',  ( 13.14518615778179544, 36.38632812608393863, -1.609821015232357215E-15 ) ) ;
#22390 = ADVANCED_FACE ( 'NONE', ( #1193 ), #24163, .T. ) ;
#22391 = CARTESIAN_POINT ( 'NONE',  ( 136.9444237971526945, 31.55306878032414986, -11.16113333171310451 ) ) ;
#22392 = CARTESIAN_POINT ( 'NONE',  ( 55.40115559117954547, 32.36796874999999574, 9.598844408820459861 ) ) ;
#22393 = FACE_OUTER_BOUND ( 'NONE', #23946, .T. ) ;
#22394 = EDGE_CURVE ( 'NONE', #20179, #18889, #5071, .T. ) ;
#22395 = CARTESIAN_POINT ( 'NONE',  ( 78.57481594606305464, 36.78320312716788010, -5.622872871577873966 ) ) ;
#22396 = CARTESIAN_POINT ( 'NONE',  ( 101.8468681455906903, 4.458734125000016313, 9.375000001365592084 ) ) ;
#22397 = CARTESIAN_POINT ( 'NONE',  ( 195.0000000000000000, 38.81718749999999574, 13.57481594606304576 ) ) ;
#22398 = CARTESIAN_POINT ( 'NONE',  ( 104.4587341249999781, 1.846868145590750521, 10.00000000136559208 ) ) ;
#22399 = CARTESIAN_POINT ( 'NONE',  ( 97.50236033167492167, 102.3130555110000159, -48.72500000273119269 ) ) ;
#22400 = CARTESIAN_POINT ( 'NONE',  ( 104.4587341249999781, 92.56249999863440792, -6.938893903907228378E-15 ) ) ;
#22401 = CARTESIAN_POINT ( 'NONE',  ( 102.0710678118654329, 5.000000000000018652, 3.687500000000000444 ) ) ;
#22402 = CARTESIAN_POINT ( 'NONE',  ( 91.91746824999997045, 112.6261737610028320, -53.72499999726881725 ) ) ;
#22403 = CARTESIAN_POINT ( 'NONE',  ( 13.14518615778179544, 34.79882812608394005, -1.609821015232357215E-15 ) ) ;
#22404 = EDGE_CURVE ( 'NONE', #5570, #11263, #16553, .T. ) ;
#22405 = ORIENTED_EDGE ( 'NONE', *, *, #13687, .T. ) ;
#22406 = CARTESIAN_POINT ( 'NONE',  ( 2.493653234604083739E-15, 34.94765625216787441, 13.57481594606304576 ) ) ;
#22407 = DIRECTION ( 'NONE',  ( -1.224646799147411139E-16, 0.000000000000000000, -1.000000000000000000 ) ) ;
#22408 = CARTESIAN_POINT ( 'NONE',  ( 97.50000000000000000, 123.5500000021849587, 1.035533905932725096 ) ) ;
#22409 = CARTESIAN_POINT ( 'NONE',  ( 195.0000000000000000, 36.38632812608393152, -13.14518615778179544 ) ) ;
#22410 = ORIENTED_EDGE ( 'NONE', *, *, #470, .T. ) ;
#22411 = DIRECTION ( 'NONE',  ( -0.000000000000000000, -1.000000000000000000, -0.000000000000000000 ) ) ;
#22412 = CARTESIAN_POINT ( 'NONE',  ( 96.84719886470459471, 3.152801135295383084, 10.56250000136559208 ) ) ;
#22413 = EDGE_CURVE ( 'NONE', #9474, #16468, #25286, .T. ) ;
#22414 = ORIENTED_EDGE ( 'NONE', *, *, #8600, .T. ) ;
#22415 = CARTESIAN_POINT ( 'NONE',  ( 107.0000000000000142, 107.7255621263696526, -45.10000000000001563 ) ) ;
#22416 = CARTESIAN_POINT ( 'NONE',  ( -13.14518615778179900, 36.53515625108392584, -5.444914386472297529 ) ) ;
#22417 = CARTESIAN_POINT ( 'NONE',  ( 102.4999999999999858, 123.7999999999999972, -9.847140817659276890E-15 ) ) ;
#22418 = CARTESIAN_POINT ( 'NONE',  ( 130.0000000000000000, 37.57695312608392868, 13.14518615778179544 ) ) ;
#22419 = CARTESIAN_POINT ( 'NONE',  ( 13.14518615778179722, 37.22968750108394431, -5.444914386472297529 ) ) ;
#22420 = CARTESIAN_POINT ( 'NONE',  ( 9.295050272127046043, 34.69960937608393436, -9.295050272127046043 ) ) ;
#22421 = ADVANCED_FACE ( 'NONE', ( #14237 ), #7695, .T. ) ;
#22422 = CARTESIAN_POINT ( 'NONE',  ( 104.4587341249999781, 90.56249999863440792, -6.938893903907228378E-15 ) ) ;
#22423 = CARTESIAN_POINT ( 'NONE',  ( 70.36549656804798758, 54.48174559707608466, -15.00000000000000000 ) ) ;
#22424 = CARTESIAN_POINT ( 'NONE',  ( 104.9952793366501709, 103.1245878333314465, -48.67500000273120264 ) ) ;
#22425 = EDGE_CURVE ( 'NONE', #27429, #4858, #4413, .T. ) ;
#22426 = AXIS2_PLACEMENT_3D ( 'NONE', #11636, #18215, #18503 ) ;
#22427 = CARTESIAN_POINT ( 'NONE',  ( 208.5748159460630688, 40.60312499999999858, -1.662435489736055892E-15 ) ) ;
#22428 = CARTESIAN_POINT ( 'NONE',  ( 102.4999999999999858, 123.0500000021849587, 1.035533905932722876 ) ) ;
#22429 =( BOUNDED_CURVE ( )  B_SPLINE_CURVE ( 2, ( #3991, #3847, #12654, #16939, #21236, #21379, #1858, #1718, #10380 ),
 .UNSPECIFIED., .F., .F. ) 
 B_SPLINE_CURVE_WITH_KNOTS ( ( 3, 2, 2, 2, 3 ),
 ( 0.3928571428571428492, 0.4017857142857143016, 0.4107142857142856984, 0.4196428571428571508, 0.4285714285714285476 ),
 .UNSPECIFIED. ) 
 CURVE ( )  GEOMETRIC_REPRESENTATION_ITEM ( )  RATIONAL_B_SPLINE_CURVE ( ( 1.000000000000000000, 0.9238795325112867385, 1.000000000000000000, 0.9238795325112867385, 1.000000000000000000, 0.9238795325112867385, 1.000000000000000000, 0.9238795325112867385, 1.000000000000000000 ) ) 
 REPRESENTATION_ITEM ( '' )  );
#22430 = ORIENTED_EDGE ( 'NONE', *, *, #5622, .T. ) ;
#22431 = CARTESIAN_POINT ( 'NONE',  ( 13.14518615778179544, 37.18007812608393436, -1.609821015232357215E-15 ) ) ;
#22432 = CARTESIAN_POINT ( 'NONE',  ( 96.84719886470459471, 3.152801135295383084, 7.562500001365592084 ) ) ;
#22433 = CARTESIAN_POINT ( 'NONE',  ( 51.85481384221820633, 38.12265625108393863, -5.444914386472297529 ) ) ;
#22434 = PRODUCT_DEFINITION_SHAPE ( 'NONE', 'NONE',  #28209 ) ;
#22435 = DIRECTION ( 'NONE',  ( 1.000000000000000000, -0.000000000000000000, -5.782411586589357392E-17 ) ) ;
#22436 = CARTESIAN_POINT ( 'NONE',  ( 97.92893218813451028, -4.999999999999989342, 14.18749999999999645 ) ) ;
#22437 = CARTESIAN_POINT ( 'NONE',  ( 9.295050272127046043, 33.31054687608394005, -9.295050272127046043 ) ) ;
#22438 = EDGE_LOOP ( 'NONE', ( #4193, #10861, #15976, #24429 ) ) ;
#22439 = CARTESIAN_POINT ( 'NONE',  ( 102.0669872999999797, 123.3500000010924680, -9.794112055954760458E-15 ) ) ;
#22440 = CARTESIAN_POINT ( 'NONE',  ( 5.622872871577780707, 34.40195312499999858, -13.57481594606313990 ) ) ;
#22441 = CARTESIAN_POINT ( 'NONE',  ( 208.1451861577818079, 37.22968750108394431, -5.444914386472297529 ) ) ;
#22442 = CARTESIAN_POINT ( 'NONE',  ( 108.0825317499999869, 112.6261737610028320, -46.77499999726882152 ) ) ;
#22443 = ORIENTED_EDGE ( 'NONE', *, *, #25389, .T. ) ;
#22444 = CARTESIAN_POINT ( 'NONE',  ( 99.99999999999995737, 1.387778780781445676E-14, 0.000000000000000000 ) ) ;
#22445 = CARTESIAN_POINT ( 'NONE',  ( 9.295050272127047819, 33.70742187608393436, 9.295050272127046043 ) ) ;
#22446 = ORIENTED_EDGE ( 'NONE', *, *, #15415, .T. ) ;
#22447 = CARTESIAN_POINT ( 'NONE',  ( 130.0000000000000000, 34.60039062608393579, 13.14518615778179544 ) ) ;
#22448 = CARTESIAN_POINT ( 'NONE',  ( 96.46446609406721961, -3.535533905932727539, 0.2500000027311852779 ) ) ;
#22449 = CARTESIAN_POINT ( 'NONE',  ( 204.2950502721270425, 35.69179687608394147, -9.295050272127046043 ) ) ;
#22450 = ORIENTED_EDGE ( 'NONE', *, *, #23604, .F. ) ;
#22451 = CARTESIAN_POINT ( 'NONE',  ( 98.53841926354351699, 123.0500000010924850, 1.461580736456455920 ) ) ;
#22452 = CARTESIAN_POINT ( 'NONE',  ( 6.117759945537829758, 54.65941425414898447, -14.99999999999999822 ) ) ;
#22453 = APPLICATION_CONTEXT ( 'automotive_design' ) ;
#22454 = LINE ( 'NONE', #5208, #10390 ) ;
#22455 = CARTESIAN_POINT ( 'NONE',  ( 124.3771271284221314, 37.27929687716787299, 13.57481594606304753 ) ) ;
#22456 = EDGE_CURVE ( 'NONE', #15410, #15812, #13016, .T. ) ;
#22457 = CARTESIAN_POINT ( 'NONE',  ( 108.0825317500000011, 107.3738262389971680, -46.22500000273118559 ) ) ;
#22458 = CARTESIAN_POINT ( 'NONE',  ( 99.99999999999995737, 1.387778780781445676E-14, 34.79898987322334136 ) ) ;
#22459 = CARTESIAN_POINT ( 'NONE',  ( -8.312177448680279460E-16, 33.75703125216787726, -13.57481594606304576 ) ) ;
#22460 = CARTESIAN_POINT ( 'NONE',  ( 70.32379096396013551, 54.47170356488336296, 14.99999999999997868 ) ) ;
#22461 =( NAMED_UNIT ( * ) PLANE_ANGLE_UNIT ( ) SI_UNIT ( $, .RADIAN. ) );
#22462 = CARTESIAN_POINT ( 'NONE',  ( 99.99999999999995737, 4.458734125000016313, 3.187500001365592972 ) ) ;
#22463 = EDGE_LOOP ( 'NONE', ( #12446, #2855, #25080, #14043 ) ) ;
#22464 = CARTESIAN_POINT ( 'NONE',  ( 94.99999999999995737, 1.387778780781445676E-14, 13.12500000273118417 ) ) ;
#22465 = CARTESIAN_POINT ( 'NONE',  ( 103.1528011352953342, -3.152801135295355106, 8.812500001365592084 ) ) ;
#22466 = CARTESIAN_POINT ( 'NONE',  ( 204.5988444088204687, 38.12265624999999858, 9.598844408820456309 ) ) ;
#22467 = CARTESIAN_POINT ( 'NONE',  ( -5.444914386472299306, 34.35234375108392868, 13.14518615778179722 ) ) ;
#22468 = DIRECTION ( 'NONE',  ( -1.000000000000000000, 0.000000000000000000, 0.000000000000000000 ) ) ;
#22469 = CARTESIAN_POINT ( 'NONE',  ( 78.14518615778179367, 33.26093750108393721, -5.444914386472297529 ) ) ;
#22470 = AXIS2_PLACEMENT_3D ( 'NONE', #19356, #13195, #17634 ) ;
#22471 = CARTESIAN_POINT ( 'NONE',  ( 104.9999999999999858, 91.87499999726880162, -6.938893903907228378E-15 ) ) ;
#22472 = CARTESIAN_POINT ( 'NONE',  ( 108.0825317500000011, 112.6261737610028320, -46.02500000273120406 ) ) ;
#22473 = CARTESIAN_POINT ( 'NONE',  ( 13.14518615778179722, 37.72578125108393010, 5.444914386472293977 ) ) ;
#22474 = DIRECTION ( 'NONE',  ( -0.000000000000000000, -1.000000000000000000, -0.000000000000000000 ) ) ;
#22475 = DIRECTION ( 'NONE',  ( -0.5282856486898074300, 0.000000000000000000, 0.8490667072665075699 ) ) ;
#22476 = CARTESIAN_POINT ( 'NONE',  ( 99.99999999999998579, 91.12499999726880162, -4.999999999999997335 ) ) ;
#22477 = CARTESIAN_POINT ( 'NONE',  ( 116.4251840539369596, 33.85624999999999574, 0.000000000000000000 ) ) ;
#22478 = EDGE_LOOP ( 'NONE', ( #21809, #22165, #15997, #3661 ) ) ;
#22479 = CARTESIAN_POINT ( 'NONE',  ( 0.000000000000000000, 52.00000000000000711, 0.000000000000000000 ) ) ;
#22480 = CARTESIAN_POINT ( 'NONE',  ( -13.14518615778179900, 32.76484375108393010, -5.444914386472297529 ) ) ;
#22481 = CARTESIAN_POINT ( 'NONE',  ( 13.57481594606304753, 33.60820312716787583, -5.622872871577873077 ) ) ;
#22482 = CARTESIAN_POINT ( 'NONE',  ( 96.46446609406721961, 3.535533905932755072, 11.00000000273118594 ) ) ;
#22483 = CARTESIAN_POINT ( 'NONE',  ( 139.2950502721270425, 32.91367187608393152, 9.295050272127046043 ) ) ;
#22484 = CARTESIAN_POINT ( 'NONE',  ( 55.70494972787295751, 38.86679687608393863, -9.295050272127046043 ) ) ;
#22485 = DIRECTION ( 'NONE',  ( 0.000000000000000000, 0.000000000000000000, -1.000000000000000000 ) ) ;
#22486 = CARTESIAN_POINT ( 'NONE',  ( 13.14518615778179900, 40.20625000108393010, -5.444914386472297529 ) ) ;
#22487 = CARTESIAN_POINT ( 'NONE',  ( 103.5355339059327093, -3.535533905932726206, 2.374999999999998668 ) ) ;
#22488 = CARTESIAN_POINT ( 'NONE',  ( 95.00472066334981491, 103.1245878333314465, -55.57499999726882578 ) ) ;
#22489 = CARTESIAN_POINT ( 'NONE',  ( 2.493653234604083739E-15, 39.71015625216787015, 13.57481594606304576 ) ) ;
#22490 = DIRECTION ( 'NONE',  ( 8.659560562354941486E-17, 0.7071067811865469066, -0.7071067811865482389 ) ) ;
#22491 = CARTESIAN_POINT ( 'NONE',  ( 0.000000000000000000, 50.00000000000000000, 0.000000000000000000 ) ) ;
#22492 = DIRECTION ( 'NONE',  ( 0.000000000000000000, 0.000000000000000000, -1.000000000000000000 ) ) ;
#22493 = CARTESIAN_POINT ( 'NONE',  ( 101.4615807364564546, 124.2500000010924879, -1.461580736456474794 ) ) ;
#22494 = CARTESIAN_POINT ( 'NONE',  ( 99.99999999999995737, 85.00000000000000000, -5.000000000000018652 ) ) ;
#22495 = DIRECTION ( 'NONE',  ( -0.000000000000000000, -1.000000000000000000, -0.000000000000000000 ) ) ;
#22496 = FACE_OUTER_BOUND ( 'NONE', #3441, .T. ) ;
#22497 = CARTESIAN_POINT ( 'NONE',  ( 5.622872871577871301, 32.81445312499999289, -13.57481594606304753 ) ) ;
#22498 = CARTESIAN_POINT ( 'NONE',  ( -13.17415721692276165, 36.00000000000000000, 0.03826467346021143745 ) ) ;
#22499 = CARTESIAN_POINT ( 'NONE',  ( 13.14518615778179544, 34.00507812608393721, -1.609821015232357215E-15 ) ) ;
#22500 = CARTESIAN_POINT ( 'NONE',  ( 13.14518615778179900, 36.93203125108394147, 5.444914386472293977 ) ) ;
#22501 = CARTESIAN_POINT ( 'NONE',  ( 181.4251840539369596, 32.21914062500000142, -5.622872871577873077 ) ) ;
#22502 = CARTESIAN_POINT ( 'NONE',  ( -9.598844408820458085, 34.65000000216787868, -9.598844408820458085 ) ) ;
#22503 = CARTESIAN_POINT ( 'NONE',  ( -8.312177448680279460E-16, 36.83281249999999574, -13.57481594606304576 ) ) ;
#22504 = CARTESIAN_POINT ( 'NONE',  ( 2.493653234604083739E-15, 35.64218749999999147, 13.57481594606304576 ) ) ;
#22505 = CARTESIAN_POINT ( 'NONE',  ( 59.55508561352770158, 40.10703125108393152, 13.14518615778179722 ) ) ;
#22506 = CARTESIAN_POINT ( 'NONE',  ( 97.50236033167492167, 117.6869444889999841, -51.77500000273119696 ) ) ;
#22507 = CARTESIAN_POINT ( 'NONE',  ( 98.49227936199515909, 122.9999999999999858, 1.999863547705611477 ) ) ;
#22508 = VERTEX_POINT ( 'NONE', #8108 ) ;
#22509 = CARTESIAN_POINT ( 'NONE',  ( 98.53841926354351699, 123.0500000010924850, 1.461580736456455920 ) ) ;
#22510 = CARTESIAN_POINT ( 'NONE',  ( 5.622872871577878406, 34.10429687499999574, 13.57481594606304576 ) ) ;
#22511 = CARTESIAN_POINT ( 'NONE',  ( 135.4449143864723055, 33.36015625108393579, -13.14518615778179900 ) ) ;
#22512 = PRODUCT_DEFINITION ( 'UNKNOWN', '', #10832, #10044 ) ;
#22513 = ORIENTED_EDGE ( 'NONE', *, *, #16095, .F. ) ;
#22514 = CARTESIAN_POINT ( 'NONE',  ( 97.92893218813451028, 80.81250000000001421, -5.000000000000018652 ) ) ;
#22515 = EDGE_CURVE ( 'NONE', #20976, #26480, #10148, .T. ) ;
#22516 = DIRECTION ( 'NONE',  ( -0.000000000000000000, 1.000000000000000000, -0.000000000000000000 ) ) ;
#22517 = CARTESIAN_POINT ( 'NONE',  ( 103.1528011352953342, 83.06250000136560629, -3.152801135295383084 ) ) ;
#22518 = CARTESIAN_POINT ( 'NONE',  ( 97.92893218813452449, 92.68749999999998579, 4.999999999999983125 ) ) ;
#22519 = CARTESIAN_POINT ( 'NONE',  ( 78.57481594606304043, 39.06523437716786873, 5.622872871577869525 ) ) ;
#22520 = VECTOR ( 'NONE', #12489, 1000.000000000000000 ) ;
#22521 = CARTESIAN_POINT ( 'NONE',  ( 104.9952793366501709, 116.8754121666685393, -46.32499999726881867 ) ) ;
#22522 = CARTESIAN_POINT ( 'NONE',  ( 74.59884440882045453, 40.70234374999999716, -9.598844408820458085 ) ) ;
#22523 = CARTESIAN_POINT ( 'NONE',  ( 5.622872871577878406, 38.17226562716786731, 13.57481594606304576 ) ) ;
#22524 = ORIENTED_EDGE ( 'NONE', *, *, #22765, .T. ) ;
#22525 = CARTESIAN_POINT ( 'NONE',  ( 59.37712712842208873, 36.38632812499999858, 13.57481594606300135 ) ) ;
#22526 = CARTESIAN_POINT ( 'NONE',  ( 103.5355339059327093, 3.535533905932755072, 12.62499999999999822 ) ) ;
#22527 = ORIENTED_EDGE ( 'NONE', *, *, #20222, .F. ) ;
#22528 = CARTESIAN_POINT ( 'NONE',  ( 2.414731522848535132E-15, 35.39414062608393863, 13.14518615778179544 ) ) ;
#22529 = CARTESIAN_POINT ( 'NONE',  ( 195.0000000000000000, 35.34453125216787583, -13.57481594606304576 ) ) ;
#22530 = CARTESIAN_POINT ( 'NONE',  ( -9.295050272127046043, 32.51679687608393721, -9.295050272127046043 ) ) ;
#22531 = DIRECTION ( 'NONE',  ( 1.000000000000000000, 0.000000000000000000, 0.000000000000000000 ) ) ;
#22532 = CARTESIAN_POINT ( 'NONE',  ( 208.5748159460630688, 38.37070312716787157, -5.622872871577873966 ) ) ;
#22533 = CARTESIAN_POINT ( 'NONE',  ( -13.14518615778179544, 35.98945312608393721, 0.000000000000000000 ) ) ;
#22534 = DIRECTION ( 'NONE',  ( 1.000000000000000000, 0.000000000000000000, -5.782411586589357392E-17 ) ) ;
#22535 = CARTESIAN_POINT ( 'NONE',  ( 70.62287287157788285, 32.51679687499999716, 13.57481594606304576 ) ) ;
#22536 = CARTESIAN_POINT ( 'NONE',  ( -9.598844408820454532, 34.74921874999999716, 9.598844408820459861 ) ) ;
#22537 =( NAMED_UNIT ( * ) SI_UNIT ( $, .STERADIAN. ) SOLID_ANGLE_UNIT ( ) );
#22538 = CARTESIAN_POINT ( 'NONE',  ( 116.9040934463640156, 36.00000000000000000, 1.137167824541468031 ) ) ;
#22539 = CARTESIAN_POINT ( 'NONE',  ( 101.8468681455906903, 4.458734125000016313, 5.375000001365592972 ) ) ;
#22540 = CARTESIAN_POINT ( 'NONE',  ( 214.9999999999999716, 55.00000000000000000, -10.00000000000000000 ) ) ;
#22541 = AXIS2_PLACEMENT_3D ( 'NONE', #4246, #6381, #113 ) ;
#22542 = CARTESIAN_POINT ( 'NONE',  ( 101.8468681455907046, 4.458734125000016313, 9.125000001365592084 ) ) ;
#22543 = CARTESIAN_POINT ( 'NONE',  ( 93.46109445667491400, 114.7507929638356785, -47.32500000273119412 ) ) ;
#22544 = CARTESIAN_POINT ( 'NONE',  ( 98.96446609406724804, 124.1500000021849672, -2.499999999999992450 ) ) ;
#22545 = CARTESIAN_POINT ( 'NONE',  ( 94.99999999999995737, 1.387778780781445676E-14, 4.000000000000000000 ) ) ;
#22546 = CARTESIAN_POINT ( 'NONE',  ( 99.99999999999997158, 101.5015231886685712, -55.12499999726881583 ) ) ;
#22547 = CARTESIAN_POINT ( 'NONE',  ( -13.14518615778179189, 34.45156250108394147, 5.444914386472304635 ) ) ;
#22548 = EDGE_LOOP ( 'NONE', ( #15696, #3592, #5615, #25888, #17876, #14183, #10300, #14571, #771, #4319, #23088, #11406, #23497, #20451, #15883 ) ) ;
#22549 = DIRECTION ( 'NONE',  ( 0.000000000000000000, 0.000000000000000000, -1.000000000000000000 ) ) ;
#22551 = EDGE_CURVE ( 'NONE', #20179, #789, #27511, .T. ) ;
#22550 = CARTESIAN_POINT ( 'NONE',  ( 5.622872871577976994, 40.05742187716787583, -13.57481594606294095 ) ) ;
#22552 = CARTESIAN_POINT ( 'NONE',  ( 99.99999999999998579, 90.00000000000000000, -4.999999999999996447 ) ) ;
#22553 = EDGE_CURVE ( 'NONE', #13728, #19422, #18805, .T. ) ;
#22554 = CARTESIAN_POINT ( 'NONE',  ( 204.2950502721270425, 36.28710937608393294, -9.295050272127046043 ) ) ;
#22555 = VERTEX_POINT ( 'NONE', #7967 ) ;
#22556 =( BOUNDED_CURVE ( )  B_SPLINE_CURVE ( 2, ( #10003, #1203, #23135, #21272, #20721, #16287, #9871, #1755, #12411, #20857, #18578, #18983, #1616, #16712, #14277, #19128, #8011, #27834, #21131, #25546, #24989, #1339, #1477, #20996, #3884, #5611, #27693, #10274, #18712, #7875, #5469, #14420, #10133, #27281, #6026, #5891, #11996, #14561, #7738, #22995, #16427, #18845, #23276, #23410, #3611, #10421, #14138, #25260, #25124, #3465, #12131, #27412, #12270, #25409, #5751, #27554, #3749, #23551, #21841, #11115, #6437, #8573, #15251, #21555, #14827, #1896, #26104, #23969, #4448, #15106, #10698, #8288, #2172, #21418, #6161, #10562, #19686, #10834, #4028, #6569, #16980 ),
 .UNSPECIFIED., .F., .F. ) 
 B_SPLINE_CURVE_WITH_KNOTS ( ( 3, 2, 2, 2, 2, 2, 2, 2, 2, 2, 2, 2, 2, 2, 2, 2, 2, 2, 2, 2, 2, 2, 2, 2, 2, 2, 2, 2, 2, 2, 2, 2, 2, 2, 2, 2, 2, 2, 2, 2, 3 ),
 ( 0.000000000000000000, 0.02500000000000000139, 0.05000000000000000278, 0.07499999999999999722, 0.1000000000000000056, 0.1250000000000000000, 0.1499999999999999944, 0.1749999999999999889, 0.2000000000000000111, 0.2250000000000000056, 0.2500000000000000000, 0.2750000000000000222, 0.2999999999999999889, 0.3250000000000000111, 0.3499999999999999778, 0.3750000000000000000, 0.4000000000000000222, 0.4249999999999999889, 0.4500000000000000111, 0.4749999999999999778, 0.5000000000000000000, 0.5250000000000000222, 0.5500000000000000444, 0.5749999999999999556, 0.5999999999999999778, 0.6250000000000000000, 0.6500000000000000222, 0.6750000000000000444, 0.6999999999999999556, 0.7249999999999999778, 0.7500000000000000000, 0.7750000000000000222, 0.8000000000000000444, 0.8249999999999999556, 0.8499999999999999778, 0.8750000000000000000, 0.9000000000000000222, 0.9250000000000000444, 0.9499999999999999556, 0.9749999999999999778, 1.000000000000000000 ),
 .UNSPECIFIED. ) 
 CURVE ( )  GEOMETRIC_REPRESENTATION_ITEM ( )  RATIONAL_B_SPLINE_CURVE ( ( 1.000000000000000000, 0.9238795325112867385, 1.000000000000000000, 0.9238795325112867385, 1.000000000000000000, 0.9238795325112867385, 1.000000000000000000, 0.9238795325112867385, 1.000000000000000000, 0.9238795325112867385, 1.000000000000000000, 0.9238795325112867385, 1.000000000000000000, 0.9238795325112867385, 1.000000000000000000, 0.9238795325112867385, 1.000000000000000000, 0.9238795325112867385, 1.000000000000000000, 0.9238795325112867385, 1.000000000000000000, 0.9238795325112867385, 1.000000000000000000, 0.9238795325112867385, 1.000000000000000000, 0.9238795325112867385, 1.000000000000000000, 0.9238795325112867385, 1.000000000000000000, 0.9238795325112867385, 1.000000000000000000, 0.9238795325112867385, 1.000000000000000000, 0.9238795325112867385, 1.000000000000000000, 0.9238795325112867385, 1.000000000000000000, 0.9238795325112867385, 1.000000000000000000, 0.9238795325112867385, 1.000000000000000000, 0.9238795325112867385, 1.000000000000000000, 0.9238795325112867385, 1.000000000000000000, 0.9238795325112867385, 1.000000000000000000, 0.9238795325112867385, 1.000000000000000000, 0.9238795325112867385, 1.000000000000000000, 0.9238795325112867385, 1.000000000000000000, 0.9238795325112867385, 1.000000000000000000, 0.9238795325112867385, 1.000000000000000000, 0.9238795325112867385, 1.000000000000000000, 0.9238795325112867385, 1.000000000000000000, 0.9238795325112867385, 1.000000000000000000, 0.9238795325112867385, 1.000000000000000000, 0.9238795325112867385, 1.000000000000000000, 0.9238795325112867385, 1.000000000000000000, 0.9238795325112867385, 1.000000000000000000, 0.9238795325112867385, 1.000000000000000000, 0.9238795325112867385, 1.000000000000000000, 0.9238795325112867385, 1.000000000000000000, 0.9238795325112867385, 1.000000000000000000, 0.9238795325112867385, 1.000000000000000000 ) ) 
 REPRESENTATION_ITEM ( '' )  );
#22557 = CARTESIAN_POINT ( 'NONE',  ( 188.8801563723155823, 51.28708186915214640, -15.00000000000279243 ) ) ;
#22558 = CARTESIAN_POINT ( 'NONE',  ( 104.4587341249999781, -1.846868145590721655, 11.12500000136559386 ) ) ;
#22559 = ORIENTED_EDGE ( 'NONE', *, *, #9787, .T. ) ;
#22560 = CARTESIAN_POINT ( 'NONE',  ( 93.00000000000001421, 107.7255621263696668, -45.89999999999999858 ) ) ;
#22561 = VECTOR ( 'NONE', #18943, 1000.000000000000000 ) ;
#22562 = CARTESIAN_POINT ( 'NONE',  ( 13.14518615778179544, 36.98164062608393010, -1.609821015232357215E-15 ) ) ;
#22563 = LINE ( 'NONE', #11700, #10287 ) ;
#22564 = EDGE_CURVE ( 'NONE', #22244, #4790, #24039, .T. ) ;
#22565 = CARTESIAN_POINT ( 'NONE',  ( 124.5550856135277087, 38.32109375108394289, 13.14518615778179722 ) ) ;
#22566 = CARTESIAN_POINT ( 'NONE',  ( -5.444914386472297529, 36.63437500108393863, -13.14518615778179722 ) ) ;
#22567 = CARTESIAN_POINT ( 'NONE',  ( 13.14518615778179900, 36.13828125108393863, 5.444914386472293977 ) ) ;
#22569 = PRESENTATION_LAYER_ASSIGNMENT (  '', '', ( #7058 ) ) ;
#22568 = CARTESIAN_POINT ( 'NONE',  ( 99.99999999999998579, 94.31249999863440792, 4.458734124999981674 ) ) ;
#22570 = AXIS2_PLACEMENT_3D ( 'NONE', #13909, #9506, #546 ) ;
#22571 = CARTESIAN_POINT ( 'NONE',  ( 66.01413082606791249, 51.45790058219658647, -14.99999999999999645 ) ) ;
#22572 = CARTESIAN_POINT ( 'NONE',  ( 93.46109445667491400, 105.2492070361643215, -53.17500000273119554 ) ) ;
#22573 = CARTESIAN_POINT ( 'NONE',  ( 78.01985494039040248, 36.00000000000002132, 3.369129453356682014 ) ) ;
#22574 = CARTESIAN_POINT ( 'NONE',  ( 5.444914386472302859, 34.65000000108393863, 13.14518615778179189 ) ) ;
#22575 = CARTESIAN_POINT ( 'NONE',  ( 96.84719886470459471, 3.152801135295383084, 5.562500001365592972 ) ) ;
#22576 = CARTESIAN_POINT ( 'NONE',  ( 70.44491438647229131, 38.71796875108393721, -13.14518615778179722 ) ) ;
#22577 = CARTESIAN_POINT ( 'NONE',  ( 102.4999999999999858, 124.5500000000000256, 1.035533905932722876 ) ) ;
#22578 = CYLINDRICAL_SURFACE ( 'NONE', #19881, 2.500000000000008882 ) ;
#22579 = ORIENTED_EDGE ( 'NONE', *, *, #18755, .T. ) ;
#22580 = CARTESIAN_POINT ( 'NONE',  ( 13.14518615778179544, 35.59257812608393579, -1.609821015232357215E-15 ) ) ;
#22581 = ORIENTED_EDGE ( 'NONE', *, *, #8760, .F. ) ;
#22582 = CARTESIAN_POINT ( 'NONE',  ( 98.53841926354351699, 122.8500000010924680, -1.461580736456474794 ) ) ;
#22583 = CARTESIAN_POINT ( 'NONE',  ( 13.57481594606304753, 34.30273437500000000, -5.622872871577873966 ) ) ;
#22584 = EDGE_CURVE ( 'NONE', #17997, #9015, #23092, .T. ) ;
#22585 = CARTESIAN_POINT ( 'NONE',  ( 185.7049497278729575, 36.68398437608393436, -9.295050272127046043 ) ) ;
#22586 = CARTESIAN_POINT ( 'NONE',  ( 93.46109445667489979, 105.2492070361643215, -47.67499999726882720 ) ) ;
#22587 = ORIENTED_EDGE ( 'NONE', *, *, #8245, .F. ) ;
#22588 = CARTESIAN_POINT ( 'NONE',  ( -9.598844408820454532, 34.74921874999999716, 9.598844408820459861 ) ) ;
#22589 = CARTESIAN_POINT ( 'NONE',  ( -13.14518615778179189, 32.66562500108393863, 5.444914386472304635 ) ) ;
#22590 = AXIS2_PLACEMENT_3D ( 'NONE', #19865, #6605, #8470 ) ;
#22591 = ORIENTED_EDGE ( 'NONE', *, *, #8674, .F. ) ;
#22592 = CARTESIAN_POINT ( 'NONE',  ( 135.4449143864723055, 33.06250000108393294, 13.14518615778179189 ) ) ;
#22593 = CARTESIAN_POINT ( 'NONE',  ( 70.44491438647229131, 40.20625000108394431, 13.14518615778179189 ) ) ;
#22594 = EDGE_CURVE ( 'NONE', #15224, #6173, #3837, .T. ) ;
#22595 = CARTESIAN_POINT ( 'NONE',  ( 204.2950502721270425, 35.49335937608393721, 9.295050272127046043 ) ) ;
#22596 = ORIENTED_EDGE ( 'NONE', *, *, #19255, .T. ) ;
#22597 = CARTESIAN_POINT ( 'NONE',  ( 96.46446609406721961, -3.535533905932727539, 13.12500000000000000 ) ) ;
#22598 =( NAMED_UNIT ( * ) SI_UNIT ( $, .STERADIAN. ) SOLID_ANGLE_UNIT ( ) );
#22599 = CARTESIAN_POINT ( 'NONE',  ( 195.0000000000000000, 36.00000000000000000, -11.57481594606306707 ) ) ;
#22600 = CARTESIAN_POINT ( 'NONE',  ( 139.5988444088204403, 36.83281250216787583, -9.598844408820458085 ) ) ;
#22601 = CARTESIAN_POINT ( 'NONE',  ( 93.46109445667491400, 114.7507929638356785, -49.32500000273120122 ) ) ;
#22602 =( BOUNDED_CURVE ( )  B_SPLINE_CURVE ( 2, ( #4805, #8510, #10770, #19905, #1965, #4237, #6784, #19339, #15327 ),
 .UNSPECIFIED., .F., .F. ) 
 B_SPLINE_CURVE_WITH_KNOTS ( ( 3, 2, 2, 2, 3 ),
 ( 0.1785714285714286031, 0.1875000000000000000, 0.1964285714285713969, 0.2053571428571428215, 0.2142857142857142183 ),
 .UNSPECIFIED. ) 
 CURVE ( )  GEOMETRIC_REPRESENTATION_ITEM ( )  RATIONAL_B_SPLINE_CURVE ( ( 0.9999999999999997780, 0.9238795325112869605, 1.000000000000000000, 0.9238795325112867385, 1.000000000000000000, 0.9238795325112867385, 1.000000000000000000, 0.9238795325112871826, 0.9999999999999995559 ) ) 
 REPRESENTATION_ITEM ( '' )  );
#22603 = AXIS2_PLACEMENT_3D ( 'NONE', #22289, #26564, #24562 ) ;
#22604 = DIRECTION ( 'NONE',  ( 1.000000000000000000, 0.000000000000000000, -2.385244779468110248E-16 ) ) ;
#22605 = CARTESIAN_POINT ( 'NONE',  ( 6.944426393311537993, 31.75150625057403175, -11.16113171639042356 ) ) ;
#22606 = ORIENTED_EDGE ( 'NONE', *, *, #19274, .T. ) ;
#22607 = FILL_AREA_STYLE ('',( #18175 ) ) ;
#22608 = CARTESIAN_POINT ( 'NONE',  ( 98.15313185440925281, 4.458734125000016313, 3.250000001365592528 ) ) ;
#22609 = ORIENTED_EDGE ( 'NONE', *, *, #8960, .T. ) ;
#22610 = LINE ( 'NONE', #11884, #12953 ) ;
#22611 = CARTESIAN_POINT ( 'NONE',  ( 103.1528011352953342, 3.152801135295383084, 6.062500001365592084 ) ) ;
#22612 = CARTESIAN_POINT ( 'NONE',  ( 130.0000000000000000, 38.51953125216787299, -13.57481594606304576 ) ) ;
#22613 = CARTESIAN_POINT ( 'NONE',  ( -4.780039198851662618, 35.99999999999998579, 12.25280873422828520 ) ) ;
#22614 = CARTESIAN_POINT ( 'NONE',  ( 51.85481384221820633, 33.65781250108393152, 5.444914386472304635 ) ) ;
#22615 = DIRECTION ( 'NONE',  ( -0.000000000000000000, -1.000000000000000000, -0.000000000000000000 ) ) ;
#22616 = CARTESIAN_POINT ( 'NONE',  ( 95.00472066334982912, 103.1245878333314323, -46.82500000273118701 ) ) ;
#22617 = CARTESIAN_POINT ( 'NONE',  ( 5.908507747193088022, 36.04503594658365984, 12.68159279706100939 ) ) ;
#22618 = CARTESIAN_POINT ( 'NONE',  ( 99.99999999999998579, 90.00000000000000000, -6.938893903907228378E-15 ) ) ;
#22619 = CARTESIAN_POINT ( 'NONE',  ( -8.268597328389915901, 50.00000000054339466, 10.78867689284126463 ) ) ;
#22620 = CARTESIAN_POINT ( 'NONE',  ( 51.42518405393695957, 40.99999999999999289, 0.000000000000000000 ) ) ;
#22621 = CARTESIAN_POINT ( 'NONE',  ( 116.4251840539369454, 33.01289062500000426, -5.622872871577873077 ) ) ;
#22622 = ORIENTED_EDGE ( 'NONE', *, *, #25863, .F. ) ;
#22623 = CARTESIAN_POINT ( 'NONE',  ( 99.99999999999998579, 94.12499999726881583, -4.999999999999997335 ) ) ;
#22624 = CARTESIAN_POINT ( 'NONE',  ( -13.14518615778179189, 35.24531250108393721, 5.444914386472304635 ) ) ;
#22625 = CARTESIAN_POINT ( 'NONE',  ( -9.598844408820454532, 35.64218750216787868, 9.598844408820459861 ) ) ;
#22626 =( REPRESENTATION_RELATIONSHIP ('NONE','NONE', #2411, #9145 ) REPRESENTATION_RELATIONSHIP_WITH_TRANSFORMATION ( #8117 )SHAPE_REPRESENTATION_RELATIONSHIP( ) );
#22627 = VECTOR ( 'NONE', #17009, 1000.000000000000000 ) ;
#22628 = CARTESIAN_POINT ( 'NONE',  ( 104.9999999999999574, 2.071067811865491937, 10.68750000273118417 ) ) ;
#22629 = CARTESIAN_POINT ( 'NONE',  ( 143.1451861577818079, 32.16953125108393152, 5.444914386472293977 ) ) ;
#22630 = CARTESIAN_POINT ( 'NONE',  ( 70.44491438647230552, 39.51171875108392584, -13.14518615778179900 ) ) ;
#22631 = EDGE_CURVE ( 'NONE', #4145, #23060, #9962, .T. ) ;
#22632 = CARTESIAN_POINT ( 'NONE',  ( 104.9999999999999716, 80.50000000000000000, -1.449011120738813565E-14 ) ) ;
#22633 = CARTESIAN_POINT ( 'NONE',  ( 13.14518615778179544, 39.36289062608393152, -1.609821015232357215E-15 ) ) ;
#22634 = CARTESIAN_POINT ( 'NONE',  ( -5.444914386472299306, 32.16953125108393152, 13.14518615778179722 ) ) ;
#22635 = LINE ( 'NONE', #5385, #14839 ) ;
#22636 = CARTESIAN_POINT ( 'NONE',  ( 99.99999999999997158, 101.5015231886685712, -55.37499999726881583 ) ) ;
#22637 = DIRECTION ( 'NONE',  ( 0.000000000000000000, 0.000000000000000000, -1.000000000000000000 ) ) ;
#22638 = CARTESIAN_POINT ( 'NONE',  ( 185.7049497278729575, 31.92148437608393508, 9.295050272127047819 ) ) ;
#22639 = CARTESIAN_POINT ( 'NONE',  ( -9.598844408820458085, 31.47500000216787441, -9.598844408820458085 ) ) ;
#22640 = CARTESIAN_POINT ( 'NONE',  ( 101.7677669529663547, 123.9069999999781402, -1.767766952966370209 ) ) ;
#22641 = CARTESIAN_POINT ( 'NONE',  ( 100.8561741729129295, 123.2000000010924765, 2.066987299999979211 ) ) ;
#22642 = CARTESIAN_POINT ( 'NONE',  ( 128.7288612287584044, 36.00000000000000000, -13.43002483374371714 ) ) ;
#22643 = CARTESIAN_POINT ( 'NONE',  ( 130.0000000000000000, 36.53515625216787299, 13.57481594606304576 ) ) ;
#22644 = CARTESIAN_POINT ( 'NONE',  ( 195.0000000000000000, -7.395377635281828788, 13.57481594606302266 ) ) ;
#22645 = CARTESIAN_POINT ( 'NONE',  ( 13.57481594606304576, 33.45937499999999432, -1.662435489736055892E-15 ) ) ;
#22646 = CARTESIAN_POINT ( 'NONE',  ( 5.622872871577863307, 40.45429687500001137, 13.57481594606306174 ) ) ;
#22647 = CARTESIAN_POINT ( 'NONE',  ( 13.14518615778179900, 33.26093750108393721, -5.444914386472297529 ) ) ;
#22648 = CARTESIAN_POINT ( 'NONE',  ( 2.414731522848535132E-15, 33.60820312608392868, 13.14518615778179544 ) ) ;
#22649 = CARTESIAN_POINT ( 'NONE',  ( 13.14518615778179544, 34.60039062608392868, -1.609821015232357215E-15 ) ) ;
#22650 = CARTESIAN_POINT ( 'NONE',  ( 9.598844408820456309, 36.83281250216787583, -9.598844408820458085 ) ) ;
#22651 = DIRECTION ( 'NONE',  ( -0.000000000000000000, -1.000000000000000000, -0.000000000000000000 ) ) ;
#22652 = LINE ( 'NONE', #11789, #22900 ) ;
#22653 = CARTESIAN_POINT ( 'NONE',  ( 65.00000000000000000, 33.60820312608392868, 13.14518615778179544 ) ) ;
#22654 = CARTESIAN_POINT ( 'NONE',  ( 97.92893218813453871, 90.31249999999998579, -4.999999999999994671 ) ) ;
#22655 = CARTESIAN_POINT ( 'NONE',  ( -8.312177448680279460E-16, 32.07031249999999289, -13.57481594606304576 ) ) ;
#22656 = ORIENTED_EDGE ( 'NONE', *, *, #11709, .F. ) ;
#22657 = CARTESIAN_POINT ( 'NONE',  ( -8.312177448680279460E-16, 37.62656249999999858, -13.57481594606304576 ) ) ;
#22658 = CARTESIAN_POINT ( 'NONE',  ( -8.312177448680279460E-16, 32.07031249999999289, -13.57481594606304576 ) ) ;
#22659 = CARTESIAN_POINT ( 'NONE',  ( 120.7049497278729575, 34.30273437608393294, -9.295050272127046043 ) ) ;
#22660 = ORIENTED_EDGE ( 'NONE', *, *, #15915, .F. ) ;
#22661 = DIRECTION ( 'NONE',  ( 1.000000000000000000, 0.000000000000000000, 0.000000000000000000 ) ) ;
#22662 = LINE ( 'NONE', #5416, #12996 ) ;
#22663 = CARTESIAN_POINT ( 'NONE',  ( 104.9999999999999574, 79.68750000273119838, -2.071067811865491937 ) ) ;
#22664 = CARTESIAN_POINT ( 'NONE',  ( 99.99999999999998579, 90.75000000000000000, 4.999999999999984013 ) ) ;
#22665 = CARTESIAN_POINT ( 'NONE',  ( 59.37712712842213136, 38.86679687716788578, 13.57481594606304753 ) ) ;
#22666 = CARTESIAN_POINT ( 'NONE',  ( 99.99999999999997158, 101.5015231886685854, -47.12499999726882294 ) ) ;
#22667 = CARTESIAN_POINT ( 'NONE',  ( 195.0000000000000000, 40.15664062608393436, 13.14518615778179544 ) ) ;
#22668 = CARTESIAN_POINT ( 'NONE',  ( 9.598844408820459861, 37.42812500216787441, 9.598844408820456309 ) ) ;
#22669 = ORIENTED_EDGE ( 'NONE', *, *, #16960, .T. ) ;
#22670 = AXIS2_PLACEMENT_3D ( 'NONE', #17598, #4502, #21753 ) ;
#22671 = CARTESIAN_POINT ( 'NONE',  ( 185.9219080773009125, 36.00000000000000711, -9.794392408848729303 ) ) ;
#22672 = CARTESIAN_POINT ( 'NONE',  ( 97.92893218813451028, -4.999999999999989342, 12.18750000000000000 ) ) ;
#22673 = EDGE_LOOP ( 'NONE', ( #9318, #21959, #14398 ) ) ;
#22674 = CARTESIAN_POINT ( 'NONE',  ( 5.444914386472297529, 34.94765625108394147, -13.14518615778179900 ) ) ;
#22675 = CARTESIAN_POINT ( 'NONE',  ( 200.4449143864723055, 39.51171875108392584, -13.14518615778179900 ) ) ;
#22676 = CARTESIAN_POINT ( 'NONE',  ( -13.14518615778179722, 32.56640625108394005, -5.444914386472297529 ) ) ;
#22677 = PRODUCT_DEFINITION_SHAPE ( 'NONE', 'NONE',  #28208 ) ;
#22678 = CARTESIAN_POINT ( 'NONE',  ( 107.0000000000000142, 110.0000000000000000, -44.25000000273119127 ) ) ;
#22679 = CARTESIAN_POINT ( 'NONE',  ( -8.049105076161786076E-16, 32.61601562608393579, -13.14518615778179544 ) ) ;
#22680 = EDGE_CURVE ( 'NONE', #25384, #8015, #20563, .T. ) ;
#22681 = CARTESIAN_POINT ( 'NONE',  ( 116.8548138422182063, 32.56640625108394005, -5.444914386472297529 ) ) ;
#22682 = CARTESIAN_POINT ( 'NONE',  ( 55.40115559117954547, 32.16953124999999147, -9.598844408820458085 ) ) ;
#22683 = CARTESIAN_POINT ( 'NONE',  ( 97.93301270000000613, 123.1500000010924651, -9.540979117872439019E-15 ) ) ;
#22684 = CARTESIAN_POINT ( 'NONE',  ( -8.312177448680279460E-16, 36.13828125216787157, -13.57481594606304576 ) ) ;
#22685 = CARTESIAN_POINT ( 'NONE',  ( 104.4587341249999781, 1.846868145590750299, 8.250000001365592084 ) ) ;
#22686 = CARTESIAN_POINT ( 'NONE',  ( -13.57481594606304576, 37.92421875216787441, 0.000000000000000000 ) ) ;
#22687 = CARTESIAN_POINT ( 'NONE',  ( 99.99999999999995737, -4.458734124999988779, 11.68750000136559208 ) ) ;
#22688 = CARTESIAN_POINT ( 'NONE',  ( 95.00472066334982912, 103.1245878333314323, -44.82500000273117990 ) ) ;
#22689 = FACE_OUTER_BOUND ( 'NONE', #12243, .T. ) ;
#22690 = CARTESIAN_POINT ( 'NONE',  ( 214.9999999999999716, 75.00000000000000000, -9.999999999999998224 ) ) ;
#22691 = CARTESIAN_POINT ( 'NONE',  ( 95.00472066334981491, 116.8754121666685393, -53.92499999726882720 ) ) ;
#22692 = CARTESIAN_POINT ( 'NONE',  ( 9.295050272127047819, 34.69960937608393436, 9.295050272127046043 ) ) ;
#22693 = VECTOR ( 'NONE', #9803, 1000.000000000000000 ) ;
#22694 = VERTEX_POINT ( 'NONE', #19078 ) ;
#22695 = LINE ( 'NONE', #16408, #12259 ) ;
#22696 =( GEOMETRIC_REPRESENTATION_CONTEXT ( 3 ) GLOBAL_UNCERTAINTY_ASSIGNED_CONTEXT ( ( #5794 ) ) GLOBAL_UNIT_ASSIGNED_CONTEXT ( ( #13814, #9835, #22537 ) ) REPRESENTATION_CONTEXT ( 'NONE', 'WORKASPACE' ) );
#22697 = CARTESIAN_POINT ( 'NONE',  ( 9.598844408820456309, 40.00781250216787299, -9.598844408820458085 ) ) ;
#22698 = CYLINDRICAL_SURFACE ( 'NONE', #25240, 13.57481594606304576 ) ;
#22699 = CARTESIAN_POINT ( 'NONE',  ( 185.7049497278729575, 35.09648437608392868, 9.295050272127047819 ) ) ;
#22700 = ORIENTED_EDGE ( 'NONE', *, *, #7569, .F. ) ;
#22701 = CARTESIAN_POINT ( 'NONE',  ( 191.9553905430759926, 53.89089363584393766, -14.99999999999999645 ) ) ;
#22702 = CARTESIAN_POINT ( 'NONE',  ( 99.99999999999995737, -4.458734124999988779, 11.93750000136559208 ) ) ;
#22703 = ORIENTED_EDGE ( 'NONE', *, *, #2053, .F. ) ;
#22704 = CARTESIAN_POINT ( 'NONE',  ( 95.67376207875072680, 115.9545556584642867, -46.30000000000001137 ) ) ;
#22705 = CARTESIAN_POINT ( 'NONE',  ( -8.049105076161786076E-16, 37.97382812608393721, -13.14518615778179544 ) ) ;
#22706 = CARTESIAN_POINT ( 'NONE',  ( 12.07727640983618400, 35.99999999999999289, -6.197985357348142266 ) ) ;
#22707 = CARTESIAN_POINT ( 'NONE',  ( 99.99999999999998579, 128.0000000000000000, 11.50000000000000888 ) ) ;
#22708 = CARTESIAN_POINT ( 'NONE',  ( 116.8548138422182205, 37.37851562608393863, 0.000000000000000000 ) ) ;
#22709 = CARTESIAN_POINT ( 'NONE',  ( -13.14518615778179722, 36.73359375108393010, -5.444914386472297529 ) ) ;
#22710 = CARTESIAN_POINT ( 'NONE',  ( 5.444914386472302859, 36.83281250108392868, 13.14518615778179189 ) ) ;
#22711 = CARTESIAN_POINT ( 'NONE',  ( 101.8468681455907330, 93.74999999863439371, -4.458734124999994997 ) ) ;
#22712 = CARTESIAN_POINT ( 'NONE',  ( 63.49450781844505087, 53.60078691996341860, -14.99999999999999822 ) ) ;
#22713 = CARTESIAN_POINT ( 'NONE',  ( 95.00472066334981491, 116.8754121666685393, -51.67500000273118843 ) ) ;
#22714 = ORIENTED_EDGE ( 'NONE', *, *, #23222, .T. ) ;
#22715 = EDGE_CURVE ( 'NONE', #18166, #15854, #2901, .T. ) ;
#22716 = CARTESIAN_POINT ( 'NONE',  ( 74.59884440882045453, 38.12265624999999858, 9.598844408820456309 ) ) ;
#22717 = CARTESIAN_POINT ( 'NONE',  ( 13.14518615778179900, 37.22968750108393721, -5.444914386472297529 ) ) ;
#22718 = CARTESIAN_POINT ( 'NONE',  ( 101.8468681455907046, -4.458734124999987891, 7.000000001365592972 ) ) ;
#22719 =( BOUNDED_CURVE ( )  B_SPLINE_CURVE ( 2, ( #24812, #22830, #7560, #9838, #5296, #27523, #13817, #20963, #23104 ),
 .UNSPECIFIED., .F., .F. ) 
 B_SPLINE_CURVE_WITH_KNOTS ( ( 3, 2, 2, 2, 3 ),
 ( 0.5833333333333337034, 0.6250000000000002220, 0.6666666666666667407, 0.7083333333333332593, 0.7499999999999997780 ),
 .UNSPECIFIED. ) 
 CURVE ( )  GEOMETRIC_REPRESENTATION_ITEM ( )  RATIONAL_B_SPLINE_CURVE ( ( 0.9999999999999994449, 0.9238795325112872936, 1.000000000000000000, 0.9238795325112867385, 1.000000000000000000, 0.9238795325112867385, 1.000000000000000000, 0.9238795325112871826, 0.9999999999999995559 ) ) 
 REPRESENTATION_ITEM ( '' )  );
#22720 = CARTESIAN_POINT ( 'NONE',  ( 55.70494972787295751, 37.47773437608393010, 9.295050272127047819 ) ) ;
#22721 = DIRECTION ( 'NONE',  ( -0.000000000000000000, -0.000000000000000000, -1.000000000000000000 ) ) ;
#22722 = CARTESIAN_POINT ( 'NONE',  ( 93.00000000000000000, 110.0000000000000000, -50.00000000000000711 ) ) ;
#22723 = CARTESIAN_POINT ( 'NONE',  ( 204.2950502721270425, 36.88242187608393152, 9.295050272127046043 ) ) ;
#22724 = CARTESIAN_POINT ( 'NONE',  ( -5.444914386472297529, 34.25312500108393721, -13.14518615778179722 ) ) ;
#22725 = CARTESIAN_POINT ( 'NONE',  ( 99.99999999999998579, 122.5000000021849615, -2.499999999999997780 ) ) ;
#22726 = CARTESIAN_POINT ( 'NONE',  ( 9.598844408820456309, 34.35234374999999574, -9.598844408820458085 ) ) ;
#22727 = CARTESIAN_POINT ( 'NONE',  ( 189.5550856135277229, 38.22187500108393721, -13.14518615778179722 ) ) ;
#22728 = CARTESIAN_POINT ( 'NONE',  ( 102.4976396683250783, 117.6869444889999841, -52.47499999726882436 ) ) ;
#22729 = CARTESIAN_POINT ( 'NONE',  ( -13.57481594606304576, 33.11210937499999574, 5.622872871577880183 ) ) ;
#22730 = CARTESIAN_POINT ( 'NONE',  ( -13.14518615778179900, 34.94765625108392726, -5.444914386472297529 ) ) ;
#22731 = MECHANICAL_DESIGN_GEOMETRIC_PRESENTATION_REPRESENTATION (  '', ( #6771 ), #9535 ) ;
#22732 = ORIENTED_EDGE ( 'NONE', *, *, #8313, .T. ) ;
#22733 = DIRECTION ( 'NONE',  ( 0.000000000000000000, 0.000000000000000000, -1.000000000000000000 ) ) ;
#22734 = CARTESIAN_POINT ( 'NONE',  ( 51.85481384221820633, 39.95820312608393010, 0.000000000000000000 ) ) ;
#22735 = CARTESIAN_POINT ( 'NONE',  ( 185.8198241863519797, 55.00000000000000000, 9.999999999999953815 ) ) ;
#22736 = CARTESIAN_POINT ( 'NONE',  ( 208.1451861577818079, 34.79882812608394005, -1.609821015232357215E-15 ) ) ;
#22737 = EDGE_CURVE ( 'NONE', #18276, #12549, #4396, .T. ) ;
#22738 = ORIENTED_EDGE ( 'NONE', *, *, #8803, .F. ) ;
#22739 = CARTESIAN_POINT ( 'NONE',  ( 65.00000000000000000, -7.395377635281828788, -11.57481594606305109 ) ) ;
#22740 = CARTESIAN_POINT ( 'NONE',  ( 7.115490391850728180, 49.99999999945644902, -11.58166858714323055 ) ) ;
#22741 = FACE_OUTER_BOUND ( 'NONE', #4735, .T. ) ;
#22742 = CARTESIAN_POINT ( 'NONE',  ( 124.3771271284221314, 38.86679687716788578, 13.57481594606304753 ) ) ;
#22743 = CARTESIAN_POINT ( 'NONE',  ( 130.0000000000000000, 52.00000000000000711, -1.503427012513233026E-14 ) ) ;
#22744 = EDGE_CURVE ( 'NONE', #16597, #15008, #28058, .T. ) ;
#22745 = CARTESIAN_POINT ( 'NONE',  ( 73.20144618763828248, 50.69246985422719121, 14.99999999999789146 ) ) ;
#22746 = ORIENTED_EDGE ( 'NONE', *, *, #4769, .F. ) ;
#22747 = ADVANCED_FACE ( 'NONE', ( #6656 ), #24058, .T. ) ;
#22748 =( NAMED_UNIT ( * ) SI_UNIT ( $, .STERADIAN. ) SOLID_ANGLE_UNIT ( ) );
#22749 =( GEOMETRIC_REPRESENTATION_CONTEXT ( 3 ) GLOBAL_UNCERTAINTY_ASSIGNED_CONTEXT ( ( #12586 ) ) GLOBAL_UNIT_ASSIGNED_CONTEXT ( ( #16738, #9618, #3215 ) ) REPRESENTATION_CONTEXT ( 'NONE', 'WORKASPACE' ) );
#22750 = CARTESIAN_POINT ( 'NONE',  ( 95.54126587499995082, -1.846868145590724986, 4.500000001365592084 ) ) ;
#22751 = ORIENTED_EDGE ( 'NONE', *, *, #10708, .T. ) ;
#22752 = CARTESIAN_POINT ( 'NONE',  ( -13.57481594606304753, 35.49335937716787726, -5.622872871577872189 ) ) ;
#22753 = CARTESIAN_POINT ( 'NONE',  ( 104.4587341249999639, 1.442382525525748735E-14, 8.937500001365592084 ) ) ;
#22754 = CARTESIAN_POINT ( 'NONE',  ( 0.000000000000000000, 23.00000000000000000, 0.000000000000000000 ) ) ;
#22755 = ADVANCED_FACE ( 'NONE', ( #15059 ), #21499, .T. ) ;
#22756 = DIRECTION ( 'NONE',  ( 0.000000000000000000, 0.000000000000000000, 1.000000000000000000 ) ) ;
#22757 = CARTESIAN_POINT ( 'NONE',  ( 104.9999999999999716, 95.81249999726880162, 2.071067811865467956 ) ) ;
#22758 = CARTESIAN_POINT ( 'NONE',  ( -13.57481594606304753, 40.25585937716787299, -5.622872871577872189 ) ) ;
#22759 = CARTESIAN_POINT ( 'NONE',  ( 104.9952793366501851, 103.1245878333314323, -46.42500000273119554 ) ) ;
#22760 = CARTESIAN_POINT ( 'NONE',  ( -13.57481594606304576, 39.51171875216787299, 0.000000000000000000 ) ) ;
#22761 = DIRECTION ( 'NONE',  ( 0.000000000000000000, 0.000000000000000000, -1.000000000000000000 ) ) ;
#22762 = FACE_OUTER_BOUND ( 'NONE', #16638, .T. ) ;
#22763 = CARTESIAN_POINT ( 'NONE',  ( 112.9999999999999858, 123.0000000000000000, -13.00000000000001066 ) ) ;
#22764 = CARTESIAN_POINT ( 'NONE',  ( 124.3771271284221314, 32.91367187499999858, -13.57481594606304753 ) ) ;
#22765 = EDGE_CURVE ( 'NONE', #12423, #17847, #5826, .T. ) ;
#22766 = ORIENTED_EDGE ( 'NONE', *, *, #9429, .F. ) ;
#22767 = CARTESIAN_POINT ( 'NONE',  ( 5.444914386472302859, 33.85625000108393579, 13.14518615778179189 ) ) ;
#22768 = CARTESIAN_POINT ( 'NONE',  ( 9.598844408820459861, 32.66562500216787157, 9.598844408820456309 ) ) ;
#22769 = CARTESIAN_POINT ( 'NONE',  ( 94.99999999999995737, 2.071067811865491048, 6.062500002731184168 ) ) ;
#22770 = CARTESIAN_POINT ( 'NONE',  ( 135.4449143864723055, 32.36796875108393579, -13.14518615778179900 ) ) ;
#22771 = CARTESIAN_POINT ( 'NONE',  ( 51.85481384221820633, 39.01562500108393294, 5.444914386472304635 ) ) ;
#22772 =( BOUNDED_CURVE ( )  B_SPLINE_CURVE ( 2, ( #4058, #10032, #8321, #12720, #16600, #6324, #21446, #7905, #10451, #1924, #19157, #20887, #17006, #23439, #25292, #12303, #5780, #10303, #14448, #3778, #21026, #27583, #8042, #16739, #5920, #14586, #15571, #22146, #6463, #345, #6884, #15138, #4760, #9032, #13134, #24279, #13420, #11288, #8742, #2627, #26567, #10865, #17434, #24417, #20009, #489, #26133, #15426, #12854, #9171, #26426, #17863, #23856, #21869, #7020, #4334, #2347, #201, #17291, #15715, #21583, #11003, #2203, #19715, #24139, #12990, #2059, #10729, #8884, #19577, #19437, #4616, #28136, #8603, #61, #6599, #25993, #21730, #26280, #13275, #4478, #17574, #15282, #24001, #11142, #6741, #17724, #22005, #2481, #19858, #2900, #9305, #3042, #24565, #13850, #11431, #24707, #7736, #20151, #13711, #22857, #16426, #15856, #5046, #7306, #16286, #20719, #5187, #630, #18577, #14137, #9870, #9446, #16142, #22432, #9589, #24850, #11570, #13992, #4906, #5328, #11712, #2767, #22718, #13568, #7160, #20437, #24987, #20287, #22291, #18003, #918, #18293, #773, #18146, #5468, #11995, #15993, #3324, #26999, #3186, #26860, #1202, #27280, #7446, #26711, #22575, #11856, #20578, #1061, #9731, #18436, #27144, #7596, #16710, #18982, #5750, #27969, #5610, #1895, #4027, #20856, #23549, #1754, #3464, #16847, #10420, #8154, #8426, #14689, #25545, #1475, #23275, #22994, #23408, #25122, #27411, #3748, #8287, #12269, #14276, #14560, #3610, #6025, #12409, #10561, #21129, #10132, #12692, #14418, #16979, #12129, #7874, #14826, #21417, #1615, #19270, #23133, #1338, #10002, #10273, #25677, #16568, #6159, #27692, #3883, #19126, #12544, #18709, #25259, #21270, #27833, #20995, #18844, #27553, #8010, #25408, #5890, #172, #456, #6706, #2170, #19685, #17115, #13390 ),
 .UNSPECIFIED., .F., .T. ) 
 B_SPLINE_CURVE_WITH_KNOTS ( ( 3, 2, 2, 2, 2, 2, 2, 2, 2, 2, 2, 2, 2, 2, 2, 2, 2, 2, 2, 2, 2, 2, 2, 2, 2, 2, 2, 2, 2, 2, 2, 2, 2, 2, 2, 2, 2, 2, 2, 2, 2, 2, 2, 2, 2, 2, 2, 2, 2, 2, 2, 2, 2, 2, 2, 2, 2, 2, 2, 2, 2, 2, 2, 2, 2, 2, 2, 2, 2, 2, 2, 2, 2, 2, 2, 2, 2, 2, 2, 2, 2, 2, 2, 2, 2, 2, 2, 2, 2, 2, 2, 2, 2, 2, 2, 2, 2, 2, 2, 2, 2, 2, 2, 2, 2, 2, 2, 2, 2, 2, 2, 2, 3 ),
 ( 0.000000000000000000, 0.008928571428571428076, 0.01785714285714285615, 0.02678571428571428423, 0.03571428571428571230, 0.04464285714285714385, 0.05357142857142856845, 0.06250000000000000000, 0.07142857142857142461, 0.08035714285714286309, 0.08928571428571428770, 0.09821428571428571230, 0.1071428571428571369, 0.1160714285714285754, 0.1250000000000000000, 0.1339285714285714246, 0.1428571428571428492, 0.1517857142857142738, 0.1607142857142857262, 0.1696428571428571508, 0.1785714285714285754, 0.1875000000000000000, 0.1964285714285714246, 0.2053571428571428492, 0.2142857142857142738, 0.2232142857142857262, 0.2321428571428571508, 0.2410714285714285754, 0.2500000000000000000, 0.2589285714285714524, 0.2678571428571428492, 0.2767857142857143016, 0.2857142857142856984, 0.2946428571428571508, 0.3035714285714285476, 0.3125000000000000000, 0.3214285714285714524, 0.3303571428571428492, 0.3392857142857143016, 0.3482142857142856984, 0.3571428571428571508, 0.3660714285714285476, 0.3750000000000000000, 0.3839285714285714524, 0.3928571428571428492, 0.4017857142857143016, 0.4107142857142856984, 0.4196428571428571508, 0.4285714285714285476, 0.4375000000000000000, 0.4464285714285714524, 0.4553571428571428492, 0.4642857142857143016, 0.4732142857142856984, 0.4821428571428571508, 0.4910714285714285476, 0.5000000000000000000, 0.5089285714285713969, 0.5178571428571429047, 0.5267857142857143016, 0.5357142857142856984, 0.5446428571428570953, 0.5535714285714286031, 0.5625000000000000000, 0.5714285714285713969, 0.5803571428571429047, 0.5892857142857143016, 0.5982142857142856984, 0.6071428571428570953, 0.6160714285714286031, 0.6250000000000000000, 0.6339285714285713969, 0.6428571428571429047, 0.6517857142857143016, 0.6607142857142856984, 0.6696428571428570953, 0.6785714285714286031, 0.6875000000000000000, 0.6964285714285713969, 0.7053571428571429047, 0.7142857142857143016, 0.7232142857142856984, 0.7321428571428570953, 0.7410714285714286031, 0.7500000000000000000, 0.7589285714285713969, 0.7678571428571429047, 0.7767857142857143016, 0.7857142857142856984, 0.7946428571428570953, 0.8035714285714286031, 0.8125000000000000000, 0.8214285714285713969, 0.8303571428571429047, 0.8392857142857143016, 0.8482142857142856984, 0.8571428571428570953, 0.8660714285714286031, 0.8750000000000000000, 0.8839285714285713969, 0.8928571428571429047, 0.9017857142857143016, 0.9107142857142856984, 0.9196428571428570953, 0.9285714285714286031, 0.9375000000000000000, 0.9464285714285713969, 0.9553571428571429047, 0.9642857142857143016, 0.9732142857142856984, 0.9821428571428570953, 0.9910714285714286031, 1.000000000000000000 ),
 .UNSPECIFIED. ) 
 CURVE ( )  GEOMETRIC_REPRESENTATION_ITEM ( )  RATIONAL_B_SPLINE_CURVE ( ( 1.000000000000000000, 0.9238795325112867385, 1.000000000000000000, 0.9238795325112867385, 1.000000000000000000, 0.9238795325112867385, 1.000000000000000000, 0.9238795325112867385, 1.000000000000000000, 0.9238795325112867385, 1.000000000000000000, 0.9238795325112867385, 1.000000000000000000, 0.9238795325112867385, 1.000000000000000000, 0.9238795325112867385, 1.000000000000000000, 0.9238795325112867385, 1.000000000000000000, 0.9238795325112867385, 1.000000000000000000, 0.9238795325112867385, 1.000000000000000000, 0.9238795325112867385, 1.000000000000000000, 0.9238795325112867385, 1.000000000000000000, 0.9238795325112867385, 1.000000000000000000, 0.9238795325112867385, 1.000000000000000000, 0.9238795325112867385, 1.000000000000000000, 0.9238795325112867385, 1.000000000000000000, 0.9238795325112867385, 1.000000000000000000, 0.9238795325112867385, 1.000000000000000000, 0.9238795325112867385, 1.000000000000000000, 0.9238795325112867385, 1.000000000000000000, 0.9238795325112867385, 1.000000000000000000, 0.9238795325112867385, 1.000000000000000000, 0.9238795325112867385, 1.000000000000000000, 0.9238795325112867385, 1.000000000000000000, 0.9238795325112867385, 1.000000000000000000, 0.9238795325112867385, 1.000000000000000000, 0.9238795325112867385, 1.000000000000000000, 0.9238795325112867385, 1.000000000000000000, 0.9238795325112867385, 1.000000000000000000, 0.9238795325112867385, 1.000000000000000000, 0.9238795325112867385, 1.000000000000000000, 0.9238795325112867385, 1.000000000000000000, 0.9238795325112867385, 1.000000000000000000, 0.9238795325112867385, 1.000000000000000000, 0.9238795325112867385, 1.000000000000000000, 0.9238795325112867385, 1.000000000000000000, 0.9238795325112867385, 1.000000000000000000, 0.9238795325112867385, 1.000000000000000000, 0.9238795325112867385, 1.000000000000000000, 0.9238795325112867385, 1.000000000000000000, 0.9238795325112867385, 1.000000000000000000, 0.9238795325112867385, 1.000000000000000000, 0.9238795325112867385, 1.000000000000000000, 0.9238795325112867385, 1.000000000000000000, 0.9238795325112867385, 1.000000000000000000, 0.9238795325112867385, 1.000000000000000000, 0.9238795325112867385, 1.000000000000000000, 0.9238795325112867385, 1.000000000000000000, 0.9238795325112867385, 1.000000000000000000, 0.9238795325112867385, 1.000000000000000000, 0.9238795325112867385, 1.000000000000000000, 0.9238795325112867385, 1.000000000000000000, 0.9238795325112867385, 1.000000000000000000, 0.9238795325112867385, 1.000000000000000000, 0.9238795325112867385, 1.000000000000000000, 0.9238795325112867385, 1.000000000000000000, 0.9238795325112867385, 1.000000000000000000, 0.9238795325112867385, 1.000000000000000000, 0.9238795325112867385, 1.000000000000000000, 0.9238795325112867385, 1.000000000000000000, 0.9238795325112867385, 1.000000000000000000, 0.9238795325112867385, 1.000000000000000000, 0.9238795325112867385, 1.000000000000000000, 0.9238795325112867385, 1.000000000000000000, 0.9238795325112867385, 1.000000000000000000, 0.9238795325112867385, 1.000000000000000000, 0.9238795325112867385, 1.000000000000000000, 0.9238795325112867385, 1.000000000000000000, 0.9238795325112867385, 1.000000000000000000, 0.9238795325112867385, 1.000000000000000000, 0.9238795325112867385, 1.000000000000000000, 0.9238795325112867385, 1.000000000000000000, 0.9238795325112867385, 1.000000000000000000, 0.9238795325112867385, 1.000000000000000000, 0.9238795325112867385, 1.000000000000000000, 0.9238795325112867385, 1.000000000000000000, 0.9238795325112867385, 1.000000000000000000, 0.9238795325112867385, 1.000000000000000000, 0.9238795325112867385, 1.000000000000000000, 0.9238795325112867385, 1.000000000000000000, 0.9238795325112867385, 1.000000000000000000, 0.9238795325112867385, 1.000000000000000000, 0.9238795325112867385, 1.000000000000000000, 0.9238795325112867385, 1.000000000000000000, 0.9238795325112867385, 1.000000000000000000, 0.9238795325112867385, 1.000000000000000000, 0.9238795325112867385, 1.000000000000000000, 0.9238795325112867385, 1.000000000000000000, 0.9238795325112867385, 1.000000000000000000, 0.9238795325112867385, 1.000000000000000000, 0.9238795325112867385, 1.000000000000000000, 0.9238795325112867385, 1.000000000000000000, 0.9238795325112867385, 1.000000000000000000, 0.9238795325112867385, 1.000000000000000000, 0.9238795325112867385, 1.000000000000000000, 0.9238795325112867385, 1.000000000000000000, 0.9238795325112867385, 1.000000000000000000, 0.9238795325112867385, 1.000000000000000000, 0.9238795325112867385, 1.000000000000000000, 0.9238795325112867385, 1.000000000000000000, 0.9238795325112867385, 1.000000000000000000, 0.9238795325112867385, 1.000000000000000000, 0.9238795325112867385, 1.000000000000000000, 0.9238795325112867385, 1.000000000000000000, 0.9238795325112867385, 1.000000000000000000, 0.9238795325112867385, 1.000000000000000000, 0.9238795325112867385, 1.000000000000000000, 0.9238795325112867385, 1.000000000000000000, 0.9238795325112867385, 1.000000000000000000, 0.9238795325112867385, 1.000000000000000000, 0.9238795325112867385, 1.000000000000000000 ) ) 
 REPRESENTATION_ITEM ( '' )  );
#22773 = CARTESIAN_POINT ( 'NONE',  ( 96.46446609406721961, 3.535533905932755072, 14.87500000000000000 ) ) ;
#22774 = CARTESIAN_POINT ( 'NONE',  ( 13.14518615778179900, 38.51953125108393294, 5.444914386472293977 ) ) ;
#22775 = CARTESIAN_POINT ( 'NONE',  ( 99.99999999999998579, 90.00000000000000000, -6.938893903907228378E-15 ) ) ;
#22776 = CARTESIAN_POINT ( 'NONE',  ( 182.1602487631418228, 35.99999999999998579, 2.850296047819894873 ) ) ;
#22777 = CARTESIAN_POINT ( 'NONE',  ( 65.00000000000000000, 50.00000000000000000, -13.57481594606305109 ) ) ;
#22778 = CARTESIAN_POINT ( 'NONE',  ( -9.598844408820454532, 38.02343750216788010, 9.598844408820459861 ) ) ;
#22779 = CARTESIAN_POINT ( 'NONE',  ( 181.8548138422182205, 31.82226562608393650, 0.000000000000000000 ) ) ;
#22780 = FACE_OUTER_BOUND ( 'NONE', #15808, .T. ) ;
#22781 = CARTESIAN_POINT ( 'NONE',  ( 106.9999999999999858, 107.7255621263696810, -52.10000000000000142 ) ) ;
#22782 = CARTESIAN_POINT ( 'NONE',  ( 98.53841926354351699, 123.8500000010924680, 1.461580736456455920 ) ) ;
#22783 = CARTESIAN_POINT ( 'NONE',  ( 97.83688103937535629, 116.6573956140660897, -50.89999999453764445 ) ) ;
#22784 = CARTESIAN_POINT ( 'NONE',  ( 94.33688103937537051, 105.8855032339526758, -47.80000000000001137 ) ) ;
#22785 = LINE ( 'NONE', #11352, #26052 ) ;
#22786 = CARTESIAN_POINT ( 'NONE',  ( -5.622872871577873077, 33.21132812499999432, 13.57481594606304753 ) ) ;
#22787 = CARTESIAN_POINT ( 'NONE',  ( -13.10247082172194943, 36.00000000000000711, -1.608626461598226420 ) ) ;
#22788 = CARTESIAN_POINT ( 'NONE',  ( 13.14518615778179544, 34.79882812608394005, -1.609821015232357215E-15 ) ) ;
#22789 = CARTESIAN_POINT ( 'NONE',  ( -13.14518615778179189, 32.66562500108393863, 5.444914386472304635 ) ) ;
#22790 = CARTESIAN_POINT ( 'NONE',  ( 200.6228728715778686, 32.81445312499999289, -13.57481594606304753 ) ) ;
#22791 = ADVANCED_FACE ( 'NONE', ( #26193 ), #8944, .F. ) ;
#22792 = CARTESIAN_POINT ( 'NONE',  ( -13.57481594606304576, 35.59257812716788294, 5.622872871577880183 ) ) ;
#22793 = CARTESIAN_POINT ( 'NONE',  ( 97.92893218813451028, -4.999999999999989342, 4.312500002731185056 ) ) ;
#22794 = CARTESIAN_POINT ( 'NONE',  ( 98.15313185440925281, 83.62500000136560629, 4.458734124999987891 ) ) ;
#22795 = CARTESIAN_POINT ( 'NONE',  ( 51.85481384221820633, 31.82226562608393650, 0.000000000000000000 ) ) ;
#22796 = CARTESIAN_POINT ( 'NONE',  ( 91.91746824999999887, 110.0000000000000000, -53.37500000273119838 ) ) ;
#22797 = FACE_OUTER_BOUND ( 'NONE', #7158, .T. ) ;
#22798 = CARTESIAN_POINT ( 'NONE',  ( 116.4251840539369738, 37.97382812716787726, 5.622872871577880183 ) ) ;
#22799 = DIRECTION ( 'NONE',  ( 0.000000000000000000, 0.000000000000000000, -1.000000000000000000 ) ) ;
#22800 = CARTESIAN_POINT ( 'NONE',  ( 105.6631189606246295, 105.8855032339526758, -47.69999999453764161 ) ) ;
#22801 = CARTESIAN_POINT ( 'NONE',  ( 116.8548138422182063, 34.35234375108393579, -5.444914386472297529 ) ) ;
#22802 = ORIENTED_EDGE ( 'NONE', *, *, #9429, .T. ) ;
#22803 = DIRECTION ( 'NONE',  ( -1.156482317317871478E-16, -0.000000000000000000, -1.000000000000000000 ) ) ;
#22804 = VECTOR ( 'NONE', #10554, 999.9999999999997726 ) ;
#22805 = CARTESIAN_POINT ( 'NONE',  ( 208.5748159460630688, 36.73359375216787015, -1.662435489736055892E-15 ) ) ;
#22806 = CARTESIAN_POINT ( 'NONE',  ( 104.4587341249999781, 82.00000000136560629, -1.846868145590750299 ) ) ;
#22807 = CARTESIAN_POINT ( 'NONE',  ( 99.99999999999998579, 91.75000000000000000, 4.999999999999984013 ) ) ;
#22808 = DIRECTION ( 'NONE',  ( -0.000000000000000000, -1.000000000000000000, -0.000000000000000000 ) ) ;
#22809 = CARTESIAN_POINT ( 'NONE',  ( 97.50236033167490746, 102.3130555110000159, -49.22499999726882436 ) ) ;
#22810 = CARTESIAN_POINT ( 'NONE',  ( 204.2950502721270425, 32.31835937608393294, -9.295050272127046043 ) ) ;
#22811 = CARTESIAN_POINT ( 'NONE',  ( 13.57481594606304753, 37.57695312716787583, -5.622872871577873077 ) ) ;
#22812 = ORIENTED_EDGE ( 'NONE', *, *, #19754, .T. ) ;
#22813 = CARTESIAN_POINT ( 'NONE',  ( 97.92893218813451028, -4.999999999999989342, 10.18749999999999822 ) ) ;
#22814 = ORIENTED_EDGE ( 'NONE', *, *, #13642, .F. ) ;
#22815 = CARTESIAN_POINT ( 'NONE',  ( -13.14518615778179900, 36.73359375108393010, -5.444914386472297529 ) ) ;
#22816 = CARTESIAN_POINT ( 'NONE',  ( 195.0000000000000000, 31.77265625216787370, 13.57481594606304576 ) ) ;
#22817 = CARTESIAN_POINT ( 'NONE',  ( -8.049105076161786076E-16, 34.00507812608393721, -13.14518615778179544 ) ) ;
#22818 = CARTESIAN_POINT ( 'NONE',  ( 103.5355339059327093, -3.535533905932726206, 12.50000000273118594 ) ) ;
#22819 = AXIS2_PLACEMENT_3D ( 'NONE', #22072, #20073, #17786 ) ;
#22820 = CARTESIAN_POINT ( 'NONE',  ( 120.7049497278729575, 39.85898437608393152, 9.295050272127047819 ) ) ;
#22821 = CARTESIAN_POINT ( 'NONE',  ( -5.444914386472299306, 32.96328125108393436, 13.14518615778179722 ) ) ;
#22822 = B_SPLINE_CURVE_WITH_KNOTS ( 'NONE', 3,
 ( #16371, #8229, #5965, #27364, #6102, #3553, #21074, #1835, #14769, #3825, #21212, #1280, #27499, #1697, #20800, #7954, #5832, #22943 ),
 .UNSPECIFIED., .F., .F.,
 ( 4, 2, 2, 2, 2, 2, 2, 2, 4 ),
 ( 0.000000000000000000, 0.004618502246277159280, 0.006927753369415741089, 0.009237004492554323765, 0.01039163005412361250, 0.01154625561569290471, 0.01385550673883148044, 0.01616475786197005618, 0.01847400898510863018 ),
 .UNSPECIFIED. ) ;
#22823 = CARTESIAN_POINT ( 'NONE',  ( 130.0000000000000000, 32.81445312608393294, 13.14518615778179544 ) ) ;
#22824 = CARTESIAN_POINT ( 'NONE',  ( 51.42518405393695957, 33.06249999999999289, 0.000000000000000000 ) ) ;
#22825 = CARTESIAN_POINT ( 'NONE',  ( 98.53841926354351699, 123.8500000010924680, -1.461580736456474794 ) ) ;
#22826 = EDGE_CURVE ( 'NONE', #18276, #4141, #16562, .T. ) ;
#22827 = DIRECTION ( 'NONE',  ( 1.000000000000000000, 0.000000000000000000, 0.000000000000000000 ) ) ;
#22828 = CYLINDRICAL_SURFACE ( 'NONE', #5022, 7.000000000000006217 ) ;
#22829 = CARTESIAN_POINT ( 'NONE',  ( 99.99999999999995737, -4.458734124999988779, 6.937500001365592972 ) ) ;
#22830 = CARTESIAN_POINT ( 'NONE',  ( 98.96446609406726225, 123.5500000000000114, 2.499999999999972022 ) ) ;
#22831 = VECTOR ( 'NONE', #18706, 1000.000000000000000 ) ;
#22832 = CARTESIAN_POINT ( 'NONE',  ( 99.99999999999995737, -4.458734124999988779, 8.687500001365592084 ) ) ;
#22833 = CARTESIAN_POINT ( 'NONE',  ( 95.67376207875072680, 115.9545556584642867, -48.80000000546237260 ) ) ;
#22834 = CARTESIAN_POINT ( 'NONE',  ( 95.54126587499999346, 91.99999999863439371, -1.846868145590737864 ) ) ;
#22835 = CARTESIAN_POINT ( 'NONE',  ( 195.0000000000000000, 40.00781250000000000, -13.57481594606304576 ) ) ;
#22836 = CARTESIAN_POINT ( 'NONE',  ( 97.93301270000000613, 124.7500000010924737, -9.540979117872439019E-15 ) ) ;
#22837 = CARTESIAN_POINT ( 'NONE',  ( 9.295050272127047819, 33.11210937608393579, 9.295050272127046043 ) ) ;
#22838 = EDGE_LOOP ( 'NONE', ( #17121, #6912, #8458, #8979, #23695, #25837, #4488, #21109 ) ) ;
#22839 =( NAMED_UNIT ( * ) SI_UNIT ( $, .STERADIAN. ) SOLID_ANGLE_UNIT ( ) );
#22840 = CARTESIAN_POINT ( 'NONE',  ( 1.137167824541903460, 36.00000000000000000, 13.09590655363594180 ) ) ;
#22841 = CARTESIAN_POINT ( 'NONE',  ( 195.0000000000000000, 33.21132812608393436, -13.14518615778179544 ) ) ;
#22842 = ORIENTED_EDGE ( 'NONE', *, *, #5465, .F. ) ;
#22843 = CARTESIAN_POINT ( 'NONE',  ( 201.1177599455311338, 54.65941425414898447, -14.99999999999999645 ) ) ;
#22844 = CARTESIAN_POINT ( 'NONE',  ( 95.54126587499996504, 1.387778780781445676E-14, 7.687500001365592084 ) ) ;
#22845 = ORIENTED_EDGE ( 'NONE', *, *, #16501, .F. ) ;
#22846 = CARTESIAN_POINT ( 'NONE',  ( 102.4976396683250925, 102.3130555110000159, -44.77500000273119696 ) ) ;
#22847 = CARTESIAN_POINT ( 'NONE',  ( -13.14518615778179544, 36.58476562608393579, 0.000000000000000000 ) ) ;
#22848 = DIRECTION ( 'NONE',  ( 0.000000000000000000, 1.000000000000000000, 0.000000000000000000 ) ) ;
#22849 = CARTESIAN_POINT ( 'NONE',  ( 97.50000000000000000, 123.4500000000000028, 1.035533905932725096 ) ) ;
#22850 = CARTESIAN_POINT ( 'NONE',  ( 135.4449143864723055, 37.13046875108393152, -13.14518615778179900 ) ) ;
#22851 = CARTESIAN_POINT ( 'NONE',  ( 9.295050272127047819, 36.28710937608393294, 9.295050272127046043 ) ) ;
#22852 = CARTESIAN_POINT ( 'NONE',  ( -5.444914386472299306, 31.97109375108393436, 13.14518615778179722 ) ) ;
#22853 = CARTESIAN_POINT ( 'NONE',  ( 104.9999999999999716, 95.81249999726881583, 2.071067811865467956 ) ) ;
#22854 = DIRECTION ( 'NONE',  ( -0.000000000000000000, 1.000000000000000000, -0.000000000000000000 ) ) ;
#22855 = ORIENTED_EDGE ( 'NONE', *, *, #20331, .F. ) ;
#22856 = CARTESIAN_POINT ( 'NONE',  ( 9.598844408820459861, 38.22187500216787015, 9.598844408820456309 ) ) ;
#22857 = CARTESIAN_POINT ( 'NONE',  ( 99.99999999999995737, 4.458734125000016313, 8.437500001365592084 ) ) ;
#22858 = DIRECTION ( 'NONE',  ( 0.000000000000000000, 0.000000000000000000, 1.000000000000000000 ) ) ;
#22859 = FACE_OUTER_BOUND ( 'NONE', #21845, .T. ) ;
#22860 = CARTESIAN_POINT ( 'NONE',  ( 68.79745186895802078, 54.08938259242986391, 14.99999999999998224 ) ) ;
#22861 = CARTESIAN_POINT ( 'NONE',  ( 102.0710678118654329, -4.999999999999989342, 2.312499999999998668 ) ) ;
#22862 = ORIENTED_EDGE ( 'NONE', *, *, #26373, .T. ) ;
#22863 = CARTESIAN_POINT ( 'NONE',  ( -8.049105076161786076E-16, 35.79101562608394005, -13.14518615778179544 ) ) ;
#22864 = CARTESIAN_POINT ( 'NONE',  ( 97.93301269999999192, 122.9000000010924936, -0.8561741729129505041 ) ) ;
#22865 = CARTESIAN_POINT ( 'NONE',  ( 95.54126587500000767, 94.06249999863440792, -7.484931351350258973E-15 ) ) ;
#22866 = DIRECTION ( 'NONE',  ( -1.000000000000000000, 0.000000000000000000, 0.000000000000000000 ) ) ;
#22867 = CARTESIAN_POINT ( 'NONE',  ( 99.99999999999997158, 118.4984768113314004, -48.37499999726881583 ) ) ;
#22868 = ADVANCED_FACE ( 'NONE', ( #8526 ), #6800, .T. ) ;
#22869 = CARTESIAN_POINT ( 'NONE',  ( 13.57481594606304753, 34.30273437500000000, -5.622872871577873077 ) ) ;
#22870 = CARTESIAN_POINT ( 'NONE',  ( 5.444914386472302859, 33.65781250108393152, 13.14518615778179189 ) ) ;
#22871 = VERTEX_POINT ( 'NONE', #1849 ) ;
#22872 = EDGE_LOOP ( 'NONE', ( #25020, #7879, #23282, #13165 ) ) ;
#22873 = FACE_OUTER_BOUND ( 'NONE', #7592, .T. ) ;
#22874 = CARTESIAN_POINT ( 'NONE',  ( 51.85481384221819923, 31.77265625108393365, -5.444914386472297529 ) ) ;
#22875 = DIRECTION ( 'NONE',  ( 0.000000000000000000, 0.000000000000000000, -1.000000000000000000 ) ) ;
#22876 = CARTESIAN_POINT ( 'NONE',  ( 208.1451861577817795, 33.16171875108393863, 5.444914386472293977 ) ) ;
#22877 = VERTEX_POINT ( 'NONE', #17211 ) ;
#22878 = CARTESIAN_POINT ( 'NONE',  ( 97.92893218813453871, 91.18749999726880162, -4.999999999999994671 ) ) ;
#22879 = CARTESIAN_POINT ( 'NONE',  ( 99.99999999999998579, 123.0000000000000000, 0.5000000000000034417 ) ) ;
#22880 = VECTOR ( 'NONE', #21646, 1000.000000000000000 ) ;
#22881 = CARTESIAN_POINT ( 'NONE',  ( 135.6228728715778686, 36.88242187716787157, -13.57481594606304753 ) ) ;
#22882 =( BOUNDED_CURVE ( )  B_SPLINE_CURVE ( 2, ( #20701, #9712, #3445, #17980, #16265, #9283, #5024, #26689, #7137 ),
 .UNSPECIFIED., .F., .T. ) 
 B_SPLINE_CURVE_WITH_KNOTS ( ( 3, 2, 2, 2, 3 ),
 ( 0.2500000000000002220, 0.2750000000000002442, 0.3000000000000002665, 0.3250000000000002887, 0.3500000000000003109 ),
 .UNSPECIFIED. ) 
 CURVE ( )  GEOMETRIC_REPRESENTATION_ITEM ( )  RATIONAL_B_SPLINE_CURVE ( ( 0.9999999999999993339, 0.9238795325112874046, 1.000000000000000000, 0.9238795325112867385, 1.000000000000000000, 0.9238795325112867385, 1.000000000000000000, 0.9238795325112857393, 1.000000000000001110 ) ) 
 REPRESENTATION_ITEM ( '' )  );
#22883 = DIRECTION ( 'NONE',  ( -0.000000000000000000, 1.000000000000000000, -0.000000000000000000 ) ) ;
#22884 = CARTESIAN_POINT ( 'NONE',  ( -8.312177448680279460E-16, 34.45156249999999432, -13.57481594606304576 ) ) ;
#22885 = CARTESIAN_POINT ( 'NONE',  ( 208.1451861577817795, 38.02343750108395426, -5.444914386472297529 ) ) ;
#22886 = ORIENTED_EDGE ( 'NONE', *, *, #324, .F. ) ;
#22887 =( NAMED_UNIT ( * ) PLANE_ANGLE_UNIT ( ) SI_UNIT ( $, .RADIAN. ) );
#22888 = CARTESIAN_POINT ( 'NONE',  ( 103.1528011352953342, -3.152801135295355106, 14.06250000136559208 ) ) ;
#22889 = CARTESIAN_POINT ( 'NONE',  ( -8.669112105337029917, 36.00000000000002842, -10.16963847934323262 ) ) ;
#22890 = CARTESIAN_POINT ( 'NONE',  ( 131.8921833570923638, 53.66387243068089674, 14.99999999999996447 ) ) ;
#22891 = CARTESIAN_POINT ( 'NONE',  ( -12.73839015785548945, 36.00000000000000000, 3.273369733618486155 ) ) ;
#22892 = CARTESIAN_POINT ( 'NONE',  ( 51.85481384221819923, 31.97109375108393436, -5.444914386472297529 ) ) ;
#22893 = CARTESIAN_POINT ( 'NONE',  ( -8.312177448680279460E-16, 40.80156249999999574, -13.57481594606304576 ) ) ;
#22894 = EDGE_CURVE ( 'NONE', #2116, #24154, #8718, .T. ) ;
#22895 = CARTESIAN_POINT ( 'NONE',  ( -13.14518615778179900, 39.11484375108394573, -5.444914386472297529 ) ) ;
#22896 = CARTESIAN_POINT ( 'NONE',  ( 1.137167824540872951, 35.99999999999998579, 13.09590655363602707 ) ) ;
#22897 = CARTESIAN_POINT ( 'NONE',  ( 96.46446609406721961, 83.12500000000000000, 3.535533905932727539 ) ) ;
#22898 = CARTESIAN_POINT ( 'NONE',  ( 120.4011555911795455, 34.74921874999999716, 9.598844408820459861 ) ) ;
#22899 = ORIENTED_EDGE ( 'NONE', *, *, #1003, .T. ) ;
#22900 = VECTOR ( 'NONE', #11930, 1000.000000000000000 ) ;
#22901 = ORIENTED_EDGE ( 'NONE', *, *, #10885, .F. ) ;
#22902 = LINE ( 'NONE', #3365, #16765 ) ;
#22903 = CARTESIAN_POINT ( 'NONE',  ( 13.14518615778179900, 32.46718750108393436, -5.444914386472297529 ) ) ;
#22904 = CARTESIAN_POINT ( 'NONE',  ( -13.57481594606304576, 35.59257812716788294, 5.622872871577880183 ) ) ;
#22905 = CARTESIAN_POINT ( 'NONE',  ( 96.46446609406721961, -3.535533905932727539, 4.250000002731185056 ) ) ;
#22906 = CARTESIAN_POINT ( 'NONE',  ( 139.2950502721270425, 39.66054687608393436, -9.295050272127046043 ) ) ;
#22907 = EDGE_CURVE ( 'NONE', #8135, #778, #17452, .T. ) ;
#22908 = CARTESIAN_POINT ( 'NONE',  ( 59.37712712842213136, 31.72304687716787441, 13.57481594606304753 ) ) ;
#22909 = EDGE_CURVE ( 'NONE', #17753, #25242, #26099, .T. ) ;
#22910 = CARTESIAN_POINT ( 'NONE',  ( 99.99999999999998579, 89.99899999999999523, 2.499999999999985789 ) ) ;
#22911 = CARTESIAN_POINT ( 'NONE',  ( -9.295050272127044266, 39.85898437608393152, 9.295050272127047819 ) ) ;
#22912 = CARTESIAN_POINT ( 'NONE',  ( 2.414731522848535132E-15, 32.21914062608393436, 13.14518615778179544 ) ) ;
#22913 = CARTESIAN_POINT ( 'NONE',  ( 0.000000000000000000, -7.395377635281828788, 13.57481594606304398 ) ) ;
#22914 = CARTESIAN_POINT ( 'NONE',  ( 95.00472066334981491, 103.1245878333314465, -51.57499999726881157 ) ) ;
#22915 = ORIENTED_EDGE ( 'NONE', *, *, #26645, .F. ) ;
#22916 =( NAMED_UNIT ( * ) SI_UNIT ( $, .STERADIAN. ) SOLID_ANGLE_UNIT ( ) );
#22917 = CARTESIAN_POINT ( 'NONE',  ( 13.14518615778179544, 40.15664062608393436, -1.609821015232357215E-15 ) ) ;
#22918 = CARTESIAN_POINT ( 'NONE',  ( 97.50000000000000000, 124.2500000000000000, 1.035533905932725096 ) ) ;
#22919 = CARTESIAN_POINT ( 'NONE',  ( 99.99999999999998579, 123.2000000000000028, -2.499999999999997780 ) ) ;
#22920 = VECTOR ( 'NONE', #10575, 1000.000000000000000 ) ;
#22921 = ADVANCED_FACE ( 'NONE', ( #13768 ), #9088, .T. ) ;
#22922 = CARTESIAN_POINT ( 'NONE',  ( 102.0669872999999939, 122.6000000010924964, -0.8561741729129507261 ) ) ;
#22923 = CARTESIAN_POINT ( 'NONE',  ( 189.3771271284221598, 39.26367187500000000, -13.57481594606310260 ) ) ;
#22924 = CARTESIAN_POINT ( 'NONE',  ( 116.4251840539369596, 40.30546875216787583, 0.000000000000000000 ) ) ;
#22925 = CARTESIAN_POINT ( 'NONE',  ( 13.57481594606304753, 33.50898437499999716, -5.622872871577873077 ) ) ;
#22926 = EDGE_LOOP ( 'NONE', ( #6054, #17815, #3832, #6821 ) ) ;
#22927 = CARTESIAN_POINT ( 'NONE',  ( 105.6631189606246295, 105.8855032339526758, -49.69999999453764161 ) ) ;
#22928 = CARTESIAN_POINT ( 'NONE',  ( -5.622872871577873077, 39.56132812499999574, 13.57481594606304753 ) ) ;
#22929 = CARTESIAN_POINT ( 'NONE',  ( 13.14518615778179900, 33.06250000108393294, -5.444914386472297529 ) ) ;
#22930 = CARTESIAN_POINT ( 'NONE',  ( -8.049105076161786076E-16, 34.79882812608393294, -13.14518615778179544 ) ) ;
#22931 = CARTESIAN_POINT ( 'NONE',  ( -8.312177448680279460E-16, 33.75703125216787726, -13.57481594606304576 ) ) ;
#22932 = FACE_OUTER_BOUND ( 'NONE', #2006, .T. ) ;
#22933 = CARTESIAN_POINT ( 'NONE',  ( 95.54126587499995082, 83.37500000136563472, -1.846868145590750077 ) ) ;
#22934 = CARTESIAN_POINT ( 'NONE',  ( 78.14518615778179367, 40.35507812608393863, -1.609821015232357215E-15 ) ) ;
#22935 = CARTESIAN_POINT ( 'NONE',  ( 1.662435489736055892E-15, 36.00000000000000000, 13.57481594606304576 ) ) ;
#22936 = CARTESIAN_POINT ( 'NONE',  ( -8.312177448680279460E-16, 35.34453125216787583, -13.57481594606304576 ) ) ;
#22937 = CARTESIAN_POINT ( 'NONE',  ( 130.0000000000000000, 39.61093749999999147, 13.57481594606304576 ) ) ;
#22938 = CARTESIAN_POINT ( 'NONE',  ( -13.57481594606304576, 32.31835937499999289, 5.622872871577880183 ) ) ;
#22939 = CARTESIAN_POINT ( 'NONE',  ( 91.91746824999997045, 107.3738262389971538, -51.77499999726881441 ) ) ;
#22940 = CARTESIAN_POINT ( 'NONE',  ( 116.8548138422182205, 35.19570312608393436, 0.000000000000000000 ) ) ;
#22941 = ADVANCED_FACE ( 'NONE', ( #26487 ), #4679, .T. ) ;
#22942 = ORIENTED_EDGE ( 'NONE', *, *, #24186, .F. ) ;
#22943 = CARTESIAN_POINT ( 'NONE',  ( -9.180175813647991845, 55.00000000000000000, -14.99999999999999822 ) ) ;
#22944 =( BOUNDED_CURVE ( )  B_SPLINE_CURVE ( 2, ( #20126, #23977, #17269 ),
 .UNSPECIFIED., .F., .T. ) 
 B_SPLINE_CURVE_WITH_KNOTS ( ( 3, 3 ),
 ( 0.8250000005912452306, 0.8500000000000007550 ),
 .UNSPECIFIED. ) 
 CURVE ( )  GEOMETRIC_REPRESENTATION_ITEM ( )  RATIONAL_B_SPLINE_CURVE ( ( 1.000000000000000000, 0.9238795325112844070, 1.000000000000002442 ) ) 
 REPRESENTATION_ITEM ( '' )  );
#22945 = CARTESIAN_POINT ( 'NONE',  ( 208.5748159460630688, 36.78320312716788010, -5.622872871577873966 ) ) ;
#22946 = CARTESIAN_POINT ( 'NONE',  ( 104.4587341249999639, 81.93750000136559208, -1.442382525525748735E-14 ) ) ;
#22947 = CARTESIAN_POINT ( 'NONE',  ( 139.2950502721270425, 38.66835937608393436, -9.295050272127046043 ) ) ;
#22948 = CARTESIAN_POINT ( 'NONE',  ( 130.0000000000000000, 38.42031249999999432, -13.57481594606304576 ) ) ;
#22949 = AXIS2_PLACEMENT_3D ( 'NONE', #371, #18023, #15454 ) ;
#22950 = CARTESIAN_POINT ( 'NONE',  ( 102.4976396683250783, 117.6869444889999841, -48.22499999726881725 ) ) ;
#22951 = CARTESIAN_POINT ( 'NONE',  ( 189.5550856135277229, 32.46718750108393436, -13.14518615778179900 ) ) ;
#22952 = CARTESIAN_POINT ( 'NONE',  ( -9.598844408820454532, 39.61093750216787868, 9.598844408820459861 ) ) ;
#22953 = ORIENTED_EDGE ( 'NONE', *, *, #22737, .T. ) ;
#22954 = EDGE_CURVE ( 'NONE', #8402, #25384, #20391, .T. ) ;
#22955 = CARTESIAN_POINT ( 'NONE',  ( 103.5355339059327093, -3.535533905932726206, 10.37499999999999822 ) ) ;
#22956 = EDGE_LOOP ( 'NONE', ( #3059, #16610, #6055, #17755 ) ) ;
#22957 = CARTESIAN_POINT ( 'NONE',  ( 2.414731522848535132E-15, 33.80664062608393294, 13.14518615778179544 ) ) ;
#22958 = CARTESIAN_POINT ( 'NONE',  ( 181.4251840539369596, 32.36796875216787583, 0.000000000000000000 ) ) ;
#22959 = CARTESIAN_POINT ( 'NONE',  ( 99.99999999999998579, 125.0000000000000000, -9.540979117872439019E-15 ) ) ;
#22960 = CARTESIAN_POINT ( 'NONE',  ( 99.99999999999995737, 5.000000000000018652, 12.87500000273118594 ) ) ;
#22961 = CARTESIAN_POINT ( 'NONE',  ( 130.0000000000000000, 40.35507812608393152, -13.14518615778179544 ) ) ;
#22962 = CARTESIAN_POINT ( 'NONE',  ( 5.444914386472302859, 33.06250000108393294, 13.14518615778179189 ) ) ;
#22963 = CARTESIAN_POINT ( 'NONE',  ( 6.944423533878893551, 31.68536041724614449, -11.16113349551710066 ) ) ;
#22964 = CARTESIAN_POINT ( 'NONE',  ( 95.54126587499999346, 91.87499999863439371, 1.846868145590722543 ) ) ;
#22965 = CARTESIAN_POINT ( 'NONE',  ( 99.14382582708707048, 123.3000000010924708, 2.066987299999979211 ) ) ;
#22966 = CARTESIAN_POINT ( 'NONE',  ( 185.4011555911795597, 39.51171874999999289, 9.598844408820459861 ) ) ;
#22967 = ITEM_DEFINED_TRANSFORMATION ( 'NONE', 'NONE', #25867,  #26844 ) ;
#22968 = CARTESIAN_POINT ( 'NONE',  ( 121.8746960822088141, 36.00000000000000000, 10.34220695173579507 ) ) ;
#22969 = CARTESIAN_POINT ( 'NONE',  ( 101.8468681455906903, -4.458734124999987891, 7.000000001365592972 ) ) ;
#22970 = CARTESIAN_POINT ( 'NONE',  ( 95.54126587499996504, 1.387778780781445676E-14, 10.43750000136559208 ) ) ;
#22971 = CARTESIAN_POINT ( 'NONE',  ( 97.83688103937538472, 116.6573956140660897, -46.90000000546238113 ) ) ;
#22972 = CARTESIAN_POINT ( 'NONE',  ( 96.84719886470463734, 90.68749999863440792, -3.152801135295366208 ) ) ;
#22973 = CARTESIAN_POINT ( 'NONE',  ( 5.622872871577742515, 39.66054687500000142, 13.57481594606318076 ) ) ;
#22974 = CARTESIAN_POINT ( 'NONE',  ( 106.5389055433250860, 114.7507929638356785, -54.42499999726882720 ) ) ;
#22975 = CARTESIAN_POINT ( 'NONE',  ( -5.444914386472297529, 31.87187500108393223, -13.14518615778179900 ) ) ;
#22976 = ORIENTED_EDGE ( 'NONE', *, *, #1318, .T. ) ;
#22977 = CARTESIAN_POINT ( 'NONE',  ( 98.15313185440925281, 84.50000000136562051, -4.458734125000016313 ) ) ;
#22978 =( BOUNDED_CURVE ( )  B_SPLINE_CURVE ( 2, ( #27180, #27036, #814, #18329, #24604 ),
 .UNSPECIFIED., .F., .F. ) 
 B_SPLINE_CURVE_WITH_KNOTS ( ( 3, 2, 3 ),
 ( 0.000000000000000000, 0.01041666666666679446, 0.02083333333333358892 ),
 .UNSPECIFIED. ) 
 CURVE ( )  GEOMETRIC_REPRESENTATION_ITEM ( )  RATIONAL_B_SPLINE_CURVE ( ( 1.000000000000000000, 0.9238795325112867385, 1.000000000000000000, 0.9238795325112848511, 1.000000000000001776 ) ) 
 REPRESENTATION_ITEM ( '' )  );
#22979 = CARTESIAN_POINT ( 'NONE',  ( 1.907364849565526780E-15, 40.99999999999999289, 15.57481594606304576 ) ) ;
#22980 = CARTESIAN_POINT ( 'NONE',  ( 204.2950502721270425, 33.90585937608393152, -9.295050272127046043 ) ) ;
#22981 = ORIENTED_EDGE ( 'NONE', *, *, #11405, .F. ) ;
#22982 = CARTESIAN_POINT ( 'NONE',  ( 187.3780364657951338, 54.91641323977498246, -15.00000000000000000 ) ) ;
#22983 = CARTESIAN_POINT ( 'NONE',  ( 95.54126587499995082, -1.846868145590724986, 8.750000001365592084 ) ) ;
#22984 = ORIENTED_EDGE ( 'NONE', *, *, #13303, .T. ) ;
#22985 = CARTESIAN_POINT ( 'NONE',  ( 99.99999999999998579, 101.5015231886685854, -48.87500000273119838 ) ) ;
#22986 = CARTESIAN_POINT ( 'NONE',  ( -13.14518615778179189, 32.66562500108393863, 5.444914386472304635 ) ) ;
#22987 = CARTESIAN_POINT ( 'NONE',  ( 5.444914386472297529, 40.30546875108393579, -13.14518615778179722 ) ) ;
#22988 = CARTESIAN_POINT ( 'NONE',  ( -5.444914386472297529, 37.42812500108394147, -13.14518615778179722 ) ) ;
#22989 = CARTESIAN_POINT ( 'NONE',  ( -5.444914386472299306, 40.10703125108393152, 13.14518615778179722 ) ) ;
#22990 = CARTESIAN_POINT ( 'NONE',  ( 103.1528011352953484, 92.68749999863440792, -3.152801135295366208 ) ) ;
#22991 = CARTESIAN_POINT ( 'NONE',  ( 94.99999999999995737, 84.56250000136560629, -1.387778780781445676E-14 ) ) ;
#22992 = DIRECTION ( 'NONE',  ( -0.000000000000000000, -1.000000000000000000, -0.000000000000000000 ) ) ;
#22993 = CARTESIAN_POINT ( 'NONE',  ( -5.444914386472299306, 32.16953125108393152, 13.14518615778179722 ) ) ;
#22994 = CARTESIAN_POINT ( 'NONE',  ( 98.15313185440923860, -4.458734124999987891, 3.875000001365591640 ) ) ;
#22995 = CARTESIAN_POINT ( 'NONE',  ( 104.4587341249999781, 82.25000000136559208, -1.846868145590750521 ) ) ;
#22996 = CARTESIAN_POINT ( 'NONE',  ( -13.14518615778179189, 35.04687500108393294, 5.444914386472304635 ) ) ;
#22997 = CARTESIAN_POINT ( 'NONE',  ( 2.493653234604083739E-15, 38.91640625216786731, 13.57481594606304576 ) ) ;
#22998 = CARTESIAN_POINT ( 'NONE',  ( 57.37605803807456084, 55.00000000000000000, 14.99999999999998579 ) ) ;
#22999 = EDGE_LOOP ( 'NONE', ( #18564, #2610 ) ) ;
#23000 = CARTESIAN_POINT ( 'NONE',  ( 13.14518615778179722, 34.05468750108394005, -5.444914386472297529 ) ) ;
#23001 = CARTESIAN_POINT ( 'NONE',  ( 98.23223304703363112, 123.4000000021849530, -1.767766952966370209 ) ) ;
#23002 = CARTESIAN_POINT ( 'NONE',  ( 104.4587341249999923, 94.62499999863439371, -1.846868145590737198 ) ) ;
#23003 = CARTESIAN_POINT ( 'NONE',  ( 99.99999999999995737, 1.387778780781445676E-14, 0.000000000000000000 ) ) ;
#23004 = LINE ( 'NONE', #3474, #15786 ) ;
#23005 = CIRCLE ( 'NONE', #10687, 13.57481594606304398 ) ;
#23006 = CARTESIAN_POINT ( 'NONE',  ( 103.5355339059327093, -3.535533905932726206, 6.500000002731185944 ) ) ;
#23007 = CARTESIAN_POINT ( 'NONE',  ( 13.14518615778179900, 32.26875000108393721, -5.444914386472297529 ) ) ;
#23008 = ORIENTED_EDGE ( 'NONE', *, *, #5320, .F. ) ;
#23009 = CARTESIAN_POINT ( 'NONE',  ( 51.85481384221820633, 38.37070312608393152, 0.000000000000000000 ) ) ;
#23010 = CARTESIAN_POINT ( 'NONE',  ( 97.50000000000000000, 124.3000000021849587, -9.540979117872439019E-15 ) ) ;
#23011 = CARTESIAN_POINT ( 'NONE',  ( 9.598844408820456309, 35.14609374999999858, -9.598844408820458085 ) ) ;
#23012 =( BOUNDED_CURVE ( )  B_SPLINE_CURVE ( 2, ( #26345, #4536, #2824, #22351, #26489, #6946, #24202, #20356, #19779 ),
 .UNSPECIFIED., .F., .T. ) 
 B_SPLINE_CURVE_WITH_KNOTS ( ( 3, 2, 2, 2, 3 ),
 ( 0.1875000000000001388, 0.1979166666666667407, 0.2083333333333333703, 0.2187499999999999722, 0.2291666666666665741 ),
 .UNSPECIFIED. ) 
 CURVE ( )  GEOMETRIC_REPRESENTATION_ITEM ( )  RATIONAL_B_SPLINE_CURVE ( ( 0.9999999999999990008, 0.9238795325112877377, 1.000000000000000000, 0.9238795325112867385, 1.000000000000000000, 0.9238795325112867385, 1.000000000000000000, 0.9238795325112872936, 0.9999999999999994449 ) ) 
 REPRESENTATION_ITEM ( '' )  );
#23013 = VERTEX_POINT ( 'NONE', #26633 ) ;
#23014 = DIRECTION ( 'NONE',  ( -0.000000000000000000, -1.000000000000000000, -0.000000000000000000 ) ) ;
#23015 = CARTESIAN_POINT ( 'NONE',  ( -1.892183357088964346, 53.66387243068090385, -15.00000000000000000 ) ) ;
#23016 = AXIS2_PLACEMENT_3D ( 'NONE', #7276, #9139, #17832 ) ;
#23017 = CARTESIAN_POINT ( 'NONE',  ( 188.8834397602831814, 54.66944451632673463, 14.99999999999994849 ) ) ;
#23018 = CARTESIAN_POINT ( 'NONE',  ( 135.6228728715778686, 38.46992187716787015, -13.57481594606304753 ) ) ;
#23019 = LINE ( 'NONE', #10027, #9214 ) ;
#23020 = CARTESIAN_POINT ( 'NONE',  ( 92.99999999999998579, 110.0000000000000000, -46.49999999453763877 ) ) ;
#23021 = CARTESIAN_POINT ( 'NONE',  ( 189.5550856135277229, 39.01562500108394005, -13.14518615778179900 ) ) ;
#23022 = EDGE_LOOP ( 'NONE', ( #14585, #13448, #2771, #15530 ) ) ;
#23023 = ADVANCED_FACE ( 'NONE', ( #406 ), #16057, .F. ) ;
#23024 = VECTOR ( 'NONE', #8461, 1000.000000000000000 ) ;
#23025 = ORIENTED_EDGE ( 'NONE', *, *, #9653, .F. ) ;
#23026 = CARTESIAN_POINT ( 'NONE',  ( 103.1528011352953342, -3.152801135295355106, 1.812500001365591640 ) ) ;
#23027 = LINE ( 'NONE', #13740, #14332 ) ;
#23028 = CARTESIAN_POINT ( 'NONE',  ( 13.57481594606304576, 38.22187499999999716, -1.662435489736055892E-15 ) ) ;
#23029 = CARTESIAN_POINT ( 'NONE',  ( 102.0710678118654329, 5.000000000000018652, 13.68750000000000000 ) ) ;
#23030 = CARTESIAN_POINT ( 'NONE',  ( 5.622872871577961895, 34.50117187716787726, -13.57481594606295339 ) ) ;
#23031 = SURFACE_STYLE_FILL_AREA ( #25026 ) ;
#23032 = CARTESIAN_POINT ( 'NONE',  ( 9.295050272127046043, 39.66054687608393436, -9.295050272127046043 ) ) ;
#23033 = CARTESIAN_POINT ( 'NONE',  ( -8.312177448680279460E-16, 40.80156249999999574, -13.57481594606304576 ) ) ;
#23034 = VECTOR ( 'NONE', #8580, 1000.000000000000000 ) ;
#23035 = CARTESIAN_POINT ( 'NONE',  ( 12.00957333851107300, 36.00000000000000711, 5.901833544882737925 ) ) ;
#23036 = CARTESIAN_POINT ( 'NONE',  ( 8.395938741298724750, 54.99999999495823744, 14.99999999999999289 ) ) ;
#23037 = CARTESIAN_POINT ( 'NONE',  ( 124.3771271284221314, 33.21132812499999432, 13.57481594606304753 ) ) ;
#23038 = ORIENTED_EDGE ( 'NONE', *, *, #27785, .T. ) ;
#23039 = ORIENTED_EDGE ( 'NONE', *, *, #14844, .T. ) ;
#23040 = CARTESIAN_POINT ( 'NONE',  ( 7.171391216998964424, 31.99955315621561525, -11.52591757658528948 ) ) ;
#23041 = CARTESIAN_POINT ( 'NONE',  ( -8.312177448680279460E-16, 38.42031249999999432, -13.57481594606304576 ) ) ;
#23042 = CARTESIAN_POINT ( 'NONE',  ( -8.049105076161786076E-16, 38.76757812608393294, -13.14518615778179544 ) ) ;
#23043 = CARTESIAN_POINT ( 'NONE',  ( 104.9999999999999574, 2.071067811865491937, 4.687500002731185944 ) ) ;
#23044 = CARTESIAN_POINT ( 'NONE',  ( 116.8548138422182205, 38.37070312608393152, 0.000000000000000000 ) ) ;
#23045 = CARTESIAN_POINT ( 'NONE',  ( 59.55508561352770158, 37.22968750108393721, -13.14518615778179900 ) ) ;
#23046 = FACE_OUTER_BOUND ( 'NONE', #10702, .T. ) ;
#23047 = CARTESIAN_POINT ( 'NONE',  ( -13.14518615778179544, 38.17226562608393436, 0.000000000000000000 ) ) ;
#23048 =( BOUNDED_SURFACE ( )  B_SPLINE_SURFACE ( 1, 2, ( 
 ( #16923, #7825, #25623, #10357, #14503, #6105, #23492, #1424, #14637, #3972, #5698, #23355, #12632, #21358, #18929, #25352, #3408, #1839, #1283, #21077, #10502, #19209, #3828, #27911, #17057, #16656, #5563, #27637, #3556, #9949, #3696, #14365, #23220, #12079, #12359, #14226, #18663, #23081, #22947, #16518, #10083, #12213, #18795, #1566, #8097, #27502, #7957, #16791, #4671, #8655, #15477, #23906, #26182, #19347, #12775, #110, #26042, #2398, #8792, #11056, #6513, #397, #6243, #26331, #8517, #8935, #4386, #21778, #19765, #6648, #17625, #14912, #4525, #249, #21491, #24192, #6792, #4108, #17483, #13333, #15334, #9079, #24050, #17346, #10640, #1972, #28050, #15189, #22059, #13043, #13185, #17202, #25761, #19489, #25907, #6377, #2257, #10919, #2533, #19629, #15050, #21923, #11197, #23768, #19914, #23632, #4244, #12904, #21634, #2110, #10777, #28187, #2677, #7498, #26764, #20489, #2948, #20344, #9358, #13758, #14049, #18344, #970, #11619, #1112, #15628, #16193, #830, #17913, #22342, #9497, #16045, #11338, #7071, #13473, #11765, #3098, #7207, #15901, #4958, #17774, #538, #9221, #20198, #9640, #5380, #18051, #5096, #20628, #26478, #24618, #2812, #18197, #26624, #22483, #26908, #15766, #7354, #6934, #24755, #11481, #5237, #24329, #13902, #22198, #22770, #4813, #27049, #13620, #22629, #24900, #24473, #3236, #11903, #20059, #683, #1388, #7647, #3792, #25039, #25310, #25586, #12451 ),
 ( #7788, #14188, #7921, #1249, #18760, #16339, #10049, #12592, #5521, #18626, #27737, #9779, #12040, #14601, #3933, #23183, #8197, #16617, #5659, #14735, #25453, #27329, #22906, #3369, #23319, #21316, #5799, #16752, #14465, #27464, #16475, #3659, #10317, #21177, #25170, #20906, #1658, #6069, #12320, #19025, #21041, #16887, #1526, #14323, #18887, #10178, #23455, #27596, #23044, #18487, #3517, #27196, #20764, #9911, #12176, #8058, #5933, #13290, #8478, #13004, #2361, #10464, #6614, #8901, #10606, #28151, #21597, #23871, #19313, #4632, #19172, #6757, #17589, #26295, #23735, #10742, #8618, #23591, #27874, #19729, #17448, #28014, #15440, #21744, #11016, #24155, #1799, #15298, #24014, #12735, #19452, #4492, #4073, #17306, #26006, #6206, #13149, #214, #21459, #26147, #21887, #1937, #8336, #17020, #2074, #25723, #8756, #14876, #17167, #25870, #6339, #15013, #2219, #4208, #10883, #12867, #19592, #6477, #15152, #4350, #75, #2780, #13866, #4921, #22447, #4774, #22019, #15730, #6898, #358, #13584, #18016, #20452, #11444, #11302, #20164, #24579, #22162, #7320, #24863, #646, #9184, #11726, #15585, #17737, #9319, #24293, #934, #26727, #24723, #7172, #5061, #22305, #15869, #18307, #22592, #5201, #13725, #5343, #19873, #9605, #2914, #2640, #26583, #11584, #20305, #13435, #20023, #26439, #16009, #3060, #790, #9460, #17877, #2496, #503, #7032, #24434, #27014, #7461, #18163, #26874, #11158 ) ),
 .UNSPECIFIED., .F., .F., .T. ) 
 B_SPLINE_SURFACE_WITH_KNOTS ( ( 2, 2 ),
 ( 3, 2, 2, 2, 2, 2, 2, 2, 2, 2, 2, 2, 2, 2, 2, 2, 2, 2, 2, 2, 2, 2, 2, 2, 2, 2, 2, 2, 2, 2, 2, 2, 2, 2, 2, 2, 2, 2, 2, 2, 2, 2, 2, 2, 2, 2, 2, 2, 2, 2, 2, 2, 2, 2, 2, 2, 2, 2, 2, 2, 2, 2, 2, 2, 2, 2, 2, 2, 2, 2, 2, 2, 2, 2, 2, 2, 2, 2, 2, 2, 2, 2, 2, 2, 2, 2, 2, 2, 2, 2, 2, 3 ),
 ( 0.000000000000000000, 1.000000000000000000 ),
 ( 0.000000000000000000, 0.01041666666666666609, 0.02083333333333333218, 0.03125000000000000000, 0.04166666666666666435, 0.05208333333333333565, 0.06250000000000000000, 0.07291666666666667129, 0.08333333333333332871, 0.09375000000000000000, 0.1041666666666666713, 0.1145833333333333287, 0.1250000000000000000, 0.1354166666666666574, 0.1458333333333333426, 0.1562500000000000000, 0.1666666666666666574, 0.1770833333333333426, 0.1875000000000000000, 0.1979166666666666574, 0.2083333333333333426, 0.2187500000000000000, 0.2291666666666666574, 0.2395833333333333426, 0.2500000000000000000, 0.2604166666666666852, 0.2708333333333333148, 0.2812500000000000000, 0.2916666666666666852, 0.3020833333333333148, 0.3125000000000000000, 0.3229166666666666852, 0.3333333333333333148, 0.3437500000000000000, 0.3541666666666666852, 0.3645833333333333148, 0.3750000000000000000, 0.3854166666666666852, 0.3958333333333333148, 0.4062500000000000000, 0.4166666666666666852, 0.4270833333333333148, 0.4375000000000000000, 0.4479166666666666852, 0.4583333333333333148, 0.4687500000000000000, 0.4791666666666666852, 0.4895833333333333148, 0.5000000000000000000, 0.5104166666666666297, 0.5208333333333333703, 0.5312500000000000000, 0.5416666666666666297, 0.5520833333333333703, 0.5625000000000000000, 0.5729166666666666297, 0.5833333333333333703, 0.5937500000000000000, 0.6041666666666666297, 0.6145833333333333703, 0.6250000000000000000, 0.6354166666666666297, 0.6458333333333333703, 0.6562500000000000000, 0.6666666666666666297, 0.6770833333333333703, 0.6875000000000000000, 0.6979166666666666297, 0.7083333333333333703, 0.7187500000000000000, 0.7291666666666666297, 0.7395833333333333703, 0.7500000000000000000, 0.7604166666666666297, 0.7708333333333333703, 0.7812500000000000000, 0.7916666666666666297, 0.8020833333333333703, 0.8125000000000000000, 0.8229166666666666297, 0.8333333333333333703, 0.8437500000000000000, 0.8541666666666666297, 0.8645833333333333703, 0.8750000000000000000, 0.8854166666666666297, 0.8958333333333333703, 0.9062500000000000000, 0.9166666666666666297, 0.9270833333333333703, 0.9375000000000000000, 0.9448587001587775980 ),
 .UNSPECIFIED. ) 
 GEOMETRIC_REPRESENTATION_ITEM ( )  RATIONAL_B_SPLINE_SURFACE ( (
 ( 1.000000000000000000, 0.9238795325112867385, 1.000000000000000000, 0.9238795325112867385, 1.000000000000000000, 0.9238795325112867385, 1.000000000000000000, 0.9238795325112867385, 1.000000000000000000, 0.9238795325112867385, 1.000000000000000000, 0.9238795325112867385, 1.000000000000000000, 0.9238795325112867385, 1.000000000000000000, 0.9238795325112867385, 1.000000000000000000, 0.9238795325112867385, 1.000000000000000000, 0.9238795325112867385, 1.000000000000000000, 0.9238795325112867385, 1.000000000000000000, 0.9238795325112867385, 1.000000000000000000, 0.9238795325112867385, 1.000000000000000000, 0.9238795325112867385, 1.000000000000000000, 0.9238795325112867385, 1.000000000000000000, 0.9238795325112867385, 1.000000000000000000, 0.9238795325112867385, 1.000000000000000000, 0.9238795325112867385, 1.000000000000000000, 0.9238795325112867385, 1.000000000000000000, 0.9238795325112867385, 1.000000000000000000, 0.9238795325112867385, 1.000000000000000000, 0.9238795325112867385, 1.000000000000000000, 0.9238795325112867385, 1.000000000000000000, 0.9238795325112867385, 1.000000000000000000, 0.9238795325112867385, 1.000000000000000000, 0.9238795325112867385, 1.000000000000000000, 0.9238795325112867385, 1.000000000000000000, 0.9238795325112867385, 1.000000000000000000, 0.9238795325112867385, 1.000000000000000000, 0.9238795325112867385, 1.000000000000000000, 0.9238795325112867385, 1.000000000000000000, 0.9238795325112867385, 1.000000000000000000, 0.9238795325112867385, 1.000000000000000000, 0.9238795325112867385, 1.000000000000000000, 0.9238795325112867385, 1.000000000000000000, 0.9238795325112867385, 1.000000000000000000, 0.9238795325112867385, 1.000000000000000000, 0.9238795325112867385, 1.000000000000000000, 0.9238795325112867385, 1.000000000000000000, 0.9238795325112867385, 1.000000000000000000, 0.9238795325112867385, 1.000000000000000000, 0.9238795325112867385, 1.000000000000000000, 0.9238795325112867385, 1.000000000000000000, 0.9238795325112867385, 1.000000000000000000, 0.9238795325112867385, 1.000000000000000000, 0.9238795325112867385, 1.000000000000000000, 0.9238795325112867385, 1.000000000000000000, 0.9238795325112867385, 1.000000000000000000, 0.9238795325112867385, 1.000000000000000000, 0.9238795325112867385, 1.000000000000000000, 0.9238795325112867385, 1.000000000000000000, 0.9238795325112867385, 1.000000000000000000, 0.9238795325112867385, 1.000000000000000000, 0.9238795325112867385, 1.000000000000000000, 0.9238795325112867385, 1.000000000000000000, 0.9238795325112867385, 1.000000000000000000, 0.9238795325112867385, 1.000000000000000000, 0.9238795325112867385, 1.000000000000000000, 0.9238795325112867385, 1.000000000000000000, 0.9238795325112867385, 1.000000000000000000, 0.9238795325112867385, 1.000000000000000000, 0.9238795325112867385, 1.000000000000000000, 0.9238795325112867385, 1.000000000000000000, 0.9238795325112867385, 1.000000000000000000, 0.9238795325112867385, 1.000000000000000000, 0.9238795325112867385, 1.000000000000000000, 0.9238795325112867385, 1.000000000000000000, 0.9238795325112867385, 1.000000000000000000, 0.9238795325112867385, 1.000000000000000000, 0.9238795325112867385, 1.000000000000000000, 0.9238795325112867385, 1.000000000000000000, 0.9238795325112867385, 1.000000000000000000, 0.9238795325112867385, 1.000000000000000000, 0.9238795325112867385, 1.000000000000000000, 0.9238795325112867385, 1.000000000000000000, 0.9238795325112867385, 1.000000000000000000, 0.9238795325112867385, 1.000000000000000000, 0.9238795325112867385, 1.000000000000000000, 0.9238795325112867385, 1.000000000000000000, 0.9238795325112867385, 1.000000000000000000, 0.9238795325112867385, 1.000000000000000000, 0.9238795325112867385, 1.000000000000000000, 0.9238795325112867385, 1.000000000000000000, 0.9238795325112867385, 1.000000000000000000, 0.9238795325112867385, 1.000000000000000000, 0.9238795325112867385, 1.000000000000000000, 0.9238795325112867385, 1.000000000000000000, 0.9238795325112867385, 1.000000000000000000, 0.9238795325112867385, 1.000000000000000000, 0.9238795325112867385, 1.000000000000000000, 0.9462258211652395667, 0.9684275895297407288),
 ( 1.000000000000000000, 0.9238795325112867385, 1.000000000000000000, 0.9238795325112867385, 1.000000000000000000, 0.9238795325112867385, 1.000000000000000000, 0.9238795325112867385, 1.000000000000000000, 0.9238795325112867385, 1.000000000000000000, 0.9238795325112867385, 1.000000000000000000, 0.9238795325112867385, 1.000000000000000000, 0.9238795325112867385, 1.000000000000000000, 0.9238795325112867385, 1.000000000000000000, 0.9238795325112867385, 1.000000000000000000, 0.9238795325112867385, 1.000000000000000000, 0.9238795325112867385, 1.000000000000000000, 0.9238795325112867385, 1.000000000000000000, 0.9238795325112867385, 1.000000000000000000, 0.9238795325112867385, 1.000000000000000000, 0.9238795325112867385, 1.000000000000000000, 0.9238795325112867385, 1.000000000000000000, 0.9238795325112867385, 1.000000000000000000, 0.9238795325112867385, 1.000000000000000000, 0.9238795325112867385, 1.000000000000000000, 0.9238795325112867385, 1.000000000000000000, 0.9238795325112867385, 1.000000000000000000, 0.9238795325112867385, 1.000000000000000000, 0.9238795325112867385, 1.000000000000000000, 0.9238795325112867385, 1.000000000000000000, 0.9238795325112867385, 1.000000000000000000, 0.9238795325112867385, 1.000000000000000000, 0.9238795325112867385, 1.000000000000000000, 0.9238795325112867385, 1.000000000000000000, 0.9238795325112867385, 1.000000000000000000, 0.9238795325112867385, 1.000000000000000000, 0.9238795325112867385, 1.000000000000000000, 0.9238795325112867385, 1.000000000000000000, 0.9238795325112867385, 1.000000000000000000, 0.9238795325112867385, 1.000000000000000000, 0.9238795325112867385, 1.000000000000000000, 0.9238795325112867385, 1.000000000000000000, 0.9238795325112867385, 1.000000000000000000, 0.9238795325112867385, 1.000000000000000000, 0.9238795325112867385, 1.000000000000000000, 0.9238795325112867385, 1.000000000000000000, 0.9238795325112867385, 1.000000000000000000, 0.9238795325112867385, 1.000000000000000000, 0.9238795325112867385, 1.000000000000000000, 0.9238795325112867385, 1.000000000000000000, 0.9238795325112867385, 1.000000000000000000, 0.9238795325112867385, 1.000000000000000000, 0.9238795325112867385, 1.000000000000000000, 0.9238795325112867385, 1.000000000000000000, 0.9238795325112867385, 1.000000000000000000, 0.9238795325112867385, 1.000000000000000000, 0.9238795325112867385, 1.000000000000000000, 0.9238795325112867385, 1.000000000000000000, 0.9238795325112867385, 1.000000000000000000, 0.9238795325112867385, 1.000000000000000000, 0.9238795325112867385, 1.000000000000000000, 0.9238795325112867385, 1.000000000000000000, 0.9238795325112867385, 1.000000000000000000, 0.9238795325112867385, 1.000000000000000000, 0.9238795325112867385, 1.000000000000000000, 0.9238795325112867385, 1.000000000000000000, 0.9238795325112867385, 1.000000000000000000, 0.9238795325112867385, 1.000000000000000000, 0.9238795325112867385, 1.000000000000000000, 0.9238795325112867385, 1.000000000000000000, 0.9238795325112867385, 1.000000000000000000, 0.9238795325112867385, 1.000000000000000000, 0.9238795325112867385, 1.000000000000000000, 0.9238795325112867385, 1.000000000000000000, 0.9238795325112867385, 1.000000000000000000, 0.9238795325112867385, 1.000000000000000000, 0.9238795325112867385, 1.000000000000000000, 0.9238795325112867385, 1.000000000000000000, 0.9238795325112867385, 1.000000000000000000, 0.9238795325112867385, 1.000000000000000000, 0.9238795325112867385, 1.000000000000000000, 0.9238795325112867385, 1.000000000000000000, 0.9238795325112867385, 1.000000000000000000, 0.9238795325112867385, 1.000000000000000000, 0.9238795325112867385, 1.000000000000000000, 0.9238795325112867385, 1.000000000000000000, 0.9238795325112867385, 1.000000000000000000, 0.9238795325112867385, 1.000000000000000000, 0.9238795325112867385, 1.000000000000000000, 0.9238795325112867385, 1.000000000000000000, 0.9238795325112867385, 1.000000000000000000, 0.9238795325112867385, 1.000000000000000000, 0.9238795325112867385, 1.000000000000000000, 0.9238795325112867385, 1.000000000000000000, 0.9238795325112867385, 1.000000000000000000, 0.9462258211652395667, 0.9684275895297407288) ) ) 
 REPRESENTATION_ITEM ( '' )  SURFACE ( )  );
#23049 = FACE_OUTER_BOUND ( 'NONE', #11843, .T. ) ;
#23050 = CARTESIAN_POINT ( 'NONE',  ( 185.8843427382057882, 36.00000000000002132, 9.510219181138902300 ) ) ;
#23051 = CARTESIAN_POINT ( 'NONE',  ( 93.46109445667489979, 105.2492070361643215, -53.67499999726882720 ) ) ;
#23052 = CARTESIAN_POINT ( 'NONE',  ( 5.444914386472297529, 40.30546875108393579, -13.14518615778179900 ) ) ;
#23053 = CARTESIAN_POINT ( 'NONE',  ( 136.1066586549483191, 35.99999999999999289, 11.74215035806533258 ) ) ;
#23054 = CARTESIAN_POINT ( 'NONE',  ( 98.23223304703363112, 123.2999999999999972, -1.767766952966370209 ) ) ;
#23055 = CARTESIAN_POINT ( 'NONE',  ( 102.0669872999999939, 122.8000000010924708, -0.8561741729129507261 ) ) ;
#23056 = CARTESIAN_POINT ( 'NONE',  ( 127.1079374786957317, 36.00000000000001421, -13.15766692561454754 ) ) ;
#23057 = CARTESIAN_POINT ( 'NONE',  ( 181.4251840539369596, 39.56132812716787583, 5.622872871577880183 ) ) ;
#23058 = CARTESIAN_POINT ( 'NONE',  ( 98.15313185440925281, 4.458734125000016313, 12.25000000136559208 ) ) ;
#23059 = CARTESIAN_POINT ( 'NONE',  ( -5.622872871577828668, 32.51679687716787015, 13.57481594606309194 ) ) ;
#23060 = VERTEX_POINT ( 'NONE', #22207 ) ;
#23061 = CARTESIAN_POINT ( 'NONE',  ( 9.598844408820459861, 40.50390624999999289, 9.598844408820456309 ) ) ;
#23062 = CARTESIAN_POINT ( 'NONE',  ( -13.57481594606304753, 39.36289062499999858, -5.622872871577873077 ) ) ;
#23063 = CARTESIAN_POINT ( 'NONE',  ( -13.14518615778179722, 32.56640625108394005, -5.444914386472297529 ) ) ;
#23064 = CARTESIAN_POINT ( 'NONE',  ( -13.57481594606304753, 32.31835937716786589, -5.622872871577873077 ) ) ;
#23065 = DIRECTION ( 'NONE',  ( 0.000000000000000000, 0.000000000000000000, -1.000000000000000000 ) ) ;
#23066 = CARTESIAN_POINT ( 'NONE',  ( 104.4587341249999781, 80.87500000136560629, 1.846868145590721655 ) ) ;
#23067 = CARTESIAN_POINT ( 'NONE',  ( 51.85481384221819923, 33.36015625108393579, -5.444914386472297529 ) ) ;
#23068 = EDGE_CURVE ( 'NONE', #24537, #2357, #5178, .T. ) ;
#23069 = CARTESIAN_POINT ( 'NONE',  ( 104.9952793366501851, 103.1245878333314323, -50.67500000273119554 ) ) ;
#23070 = CARTESIAN_POINT ( 'NONE',  ( 104.9999999999999716, 93.93750000000000000, 2.071067811865467956 ) ) ;
#23071 = VECTOR ( 'NONE', #12680, 1000.000000000000227 ) ;
#23072 = CARTESIAN_POINT ( 'NONE',  ( 97.93301269999999192, 123.9000000010924794, -0.8561741729129505041 ) ) ;
#23073 = CARTESIAN_POINT ( 'NONE',  ( 59.37712712842198926, 38.86679687716787868, 13.57481594606290720 ) ) ;
#23074 = CARTESIAN_POINT ( 'NONE',  ( 108.0825317499999869, 112.6261737610028320, -54.77499999726881441 ) ) ;
#23075 = CARTESIAN_POINT ( 'NONE',  ( 116.8548138422182063, 33.65781250108393152, 5.444914386472304635 ) ) ;
#23076 = PRODUCT_DEFINITION_SHAPE ( 'NONE', 'NONE',  #28214 ) ;
#23077 = ORIENTED_EDGE ( 'NONE', *, *, #3949, .F. ) ;
#23078 = CARTESIAN_POINT ( 'NONE',  ( 143.5748159460630688, 37.52734375216787299, -1.662435489736055892E-15 ) ) ;
#23079 = CARTESIAN_POINT ( 'NONE',  ( -8.049105076161786076E-16, 40.55351562608393579, -13.14518615778179544 ) ) ;
#23080 = CARTESIAN_POINT ( 'NONE',  ( -13.57481594606304576, 40.30546875216787583, 0.000000000000000000 ) ) ;
#23081 = CARTESIAN_POINT ( 'NONE',  ( 135.4449143864723055, 38.71796875108393721, -13.14518615778179900 ) ) ;
#23082 = CARTESIAN_POINT ( 'NONE',  ( 208.5748159460630688, 37.42812499999999432, -1.662435489736055892E-15 ) ) ;
#23083 = AXIS2_PLACEMENT_3D ( 'NONE', #16569, #8155, #12545 ) ;
#23084 = CARTESIAN_POINT ( 'NONE',  ( 91.91746824999997045, 107.3738262389971538, -53.52499999726882862 ) ) ;
#23085 = CARTESIAN_POINT ( 'NONE',  ( -13.57481594606304753, 40.25585937716787299, -5.622872871577873077 ) ) ;
#23086 = ORIENTED_EDGE ( 'NONE', *, *, #24515, .T. ) ;
#23087 = CARTESIAN_POINT ( 'NONE',  ( 94.99999999999995737, 2.071067811865491048, 9.937499999999996447 ) ) ;
#23088 = ORIENTED_EDGE ( 'NONE', *, *, #27991, .F. ) ;
#23089 = CARTESIAN_POINT ( 'NONE',  ( -13.14518615778179544, 32.81445312608393294, 0.000000000000000000 ) ) ;
#23090 = CARTESIAN_POINT ( 'NONE',  ( 185.4011555911795313, 32.26875000216787726, -9.598844408820458085 ) ) ;
#23091 = AXIS2_PLACEMENT_3D ( 'NONE', #23978, #17270, #4455 ) ;
#23092 = LINE ( 'NONE', #1575, #642 ) ;
#23093 = CARTESIAN_POINT ( 'NONE',  ( 96.46446609406721961, 3.535533905932755072, 13.00000000273118417 ) ) ;
#23094 = CARTESIAN_POINT ( 'NONE',  ( 135.4449143864723339, 37.62656250108393152, 13.14518615778179189 ) ) ;
#23095 = CARTESIAN_POINT ( 'NONE',  ( -13.14518615778179900, 31.97109375108393436, -5.444914386472297529 ) ) ;
#23096 = CARTESIAN_POINT ( 'NONE',  ( 143.5748159460630688, 37.37851562499999858, 5.622872871577868636 ) ) ;
#23097 = CARTESIAN_POINT ( 'NONE',  ( 99.99999999999998579, 95.06249999863440792, 4.458734124999981674 ) ) ;
#23098 = CARTESIAN_POINT ( 'NONE',  ( 102.4999999999999716, 123.7500000000000142, 1.035533905932722876 ) ) ;
#23099 = EDGE_CURVE ( 'NONE', #12810, #12494, #4969, .T. ) ;
#23100 = CARTESIAN_POINT ( 'NONE',  ( 208.1451861577817795, 32.46718750108393436, -5.444914386472297529 ) ) ;
#23101 = ITEM_DEFINED_TRANSFORMATION ( 'NONE', 'NONE', #3589,  #26844 ) ;
#23102 = CARTESIAN_POINT ( 'NONE',  ( 51.42518405393695957, 39.41249999999999432, 0.000000000000000000 ) ) ;
#23103 = CARTESIAN_POINT ( 'NONE',  ( 96.84719886470459471, 3.152801135295383084, 2.562500001365592084 ) ) ;
#23104 = CARTESIAN_POINT ( 'NONE',  ( 99.99999999999998579, 123.2000000000000028, -2.499999999999997780 ) ) ;
#23105 = CARTESIAN_POINT ( 'NONE',  ( 99.99999999999995737, 4.458734125000016313, 5.187500001365592972 ) ) ;
#23106 = CARTESIAN_POINT ( 'NONE',  ( 93.00000000000000000, 110.0000000000000000, -46.50000000546238255 ) ) ;
#23107 = CARTESIAN_POINT ( 'NONE',  ( 104.4587341249999781, 90.31249999863440792, -6.938893903907228378E-15 ) ) ;
#23108 = CARTESIAN_POINT ( 'NONE',  ( 94.99999999999995737, -2.071067811865466624, 4.062499999999998224 ) ) ;
#23109 = CARTESIAN_POINT ( 'NONE',  ( 0.2703369776648356093, 36.00000000000000000, 13.14949859323919590 ) ) ;
#23110 = CARTESIAN_POINT ( 'NONE',  ( 13.57481594606304753, 39.06523437499998863, -5.622872871577873077 ) ) ;
#23111 = ADVANCED_FACE ( 'NONE', ( #27060 ), #17784, .T. ) ;
#23112 = ORIENTED_EDGE ( 'NONE', *, *, #11224, .F. ) ;
#23113 = CARTESIAN_POINT ( 'NONE',  ( 98.15313185440925281, 83.50000000136560629, -4.458734125000016313 ) ) ;
#23114 = CLOSED_SHELL ( 'NONE', ( #22068, #3207, #27117, #12295, #4388, #20843, #26737, #2013, #3220, #13096, #22315, #7449, #11032, #15086, #14534, #12416, #7766, #22747, #15575, #9347, #12426, #18410, #16492, #18024, #11737, #2534, #14036, #9946, #13313, #15941, #24645, #1251, #25519, #12023, #3242, #1846, #19068, #12304, #17520, #9679, #21861, #15211, #10532, #21183, #14853, #13847, #14161, #11240, #27126, #5184, #9296, #26734, #3981, #4273, #2579, #18684, #9635, #13487, #7222, #26557, #9499, #6577, #1349, #5309, #13040, #23972, #5662, #13983, #3908, #7256, #26130, #24595, #3635, #15406, #19732, #6623, #11547 ) ) ;
#23115 = CARTESIAN_POINT ( 'NONE',  ( -9.598844408820458085, 31.47500000216787441, -9.598844408820458085 ) ) ;
#23116 = ORIENTED_EDGE ( 'NONE', *, *, #10096, .T. ) ;
#23117 = ADVANCED_FACE ( 'NONE', ( #6942 ), #22350, .F. ) ;
#23118 = VERTEX_POINT ( 'NONE', #11489 ) ;
#23119 = CARTESIAN_POINT ( 'NONE',  ( 196.6025331306099986, 53.60343507247939243, -15.00000000000000000 ) ) ;
#23120 = CARTESIAN_POINT ( 'NONE',  ( 96.84719886470459471, 3.152801135295383084, 7.562500001365592084 ) ) ;
#23121 = VERTEX_POINT ( 'NONE', #13341 ) ;
#23122 = CARTESIAN_POINT ( 'NONE',  ( 93.46109445667491400, 105.2492070361643215, -45.17500000273119554 ) ) ;
#23123 = CARTESIAN_POINT ( 'NONE',  ( -13.14518615778179189, 31.87187500108393223, 5.444914386472304635 ) ) ;
#23124 = CARTESIAN_POINT ( 'NONE',  ( 208.5748159460630688, 39.90859375216787441, -1.662435489736055892E-15 ) ) ;
#23125 = CARTESIAN_POINT ( 'NONE',  ( -13.14518615778179189, 38.22187500108393721, 5.444914386472304635 ) ) ;
#23126 = CARTESIAN_POINT ( 'NONE',  ( 91.91746824999999887, 110.0000000000000000, -45.12500000273119838 ) ) ;
#23127 = CARTESIAN_POINT ( 'NONE',  ( -9.295050272127044266, 36.08867187608393579, 9.295050272127047819 ) ) ;
#23128 = CARTESIAN_POINT ( 'NONE',  ( -13.14518615778179189, 31.87187500108393223, 5.444914386472304635 ) ) ;
#23129 = CARTESIAN_POINT ( 'NONE',  ( 78.57481594606305464, 38.22187499999999716, -1.662435489736055892E-15 ) ) ;
#23130 = CARTESIAN_POINT ( 'NONE',  ( 59.37712712842210294, 39.66054687716787441, 13.57481594606302444 ) ) ;
#23131 = DIRECTION ( 'NONE',  ( 0.000000000000000000, -1.000000000000000000, 0.000000000000000000 ) ) ;
#23132 = CARTESIAN_POINT ( 'NONE',  ( 13.14518615778179900, 33.95546875108393436, 5.444914386472293977 ) ) ;
#23133 = CARTESIAN_POINT ( 'NONE',  ( 101.8468681455907046, 4.458734125000016313, 2.375000001365592084 ) ) ;
#23134 =( BOUNDED_CURVE ( )  B_SPLINE_CURVE ( 2, ( #5484, #26728, #16010, #18164, #11727, #15870, #20734, #26584, #24724 ),
 .UNSPECIFIED., .F., .F. ) 
 B_SPLINE_CURVE_WITH_KNOTS ( ( 3, 2, 2, 2, 3 ),
 ( 0.3125000000000002220, 0.3229166666666668517, 0.3333333333333334259, 0.3437500000000000555, 0.3541666666666666852 ),
 .UNSPECIFIED. ) 
 CURVE ( )  GEOMETRIC_REPRESENTATION_ITEM ( )  RATIONAL_B_SPLINE_CURVE ( ( 0.9999999999999983347, 0.9238795325112884038, 1.000000000000000000, 0.9238795325112867385, 1.000000000000000000, 0.9238795325112867385, 1.000000000000000000, 0.9238795325112867385, 1.000000000000000000 ) ) 
 REPRESENTATION_ITEM ( '' )  );
#23135 = CARTESIAN_POINT ( 'NONE',  ( 96.84719886470459471, 84.56250000136560629, -3.152801135295383084 ) ) ;
#23136 = CARTESIAN_POINT ( 'NONE',  ( -13.14518615778179544, 35.79101562608393294, 0.000000000000000000 ) ) ;
#23137 = CARTESIAN_POINT ( 'NONE',  ( 5.622872871577786924, 32.51679687499999716, 13.57481594606313813 ) ) ;
#23138 = EDGE_CURVE ( 'NONE', #13477, #6975, #23299, .T. ) ;
#23139 = CARTESIAN_POINT ( 'NONE',  ( 66.88752872587643594, 53.66306546785492060, 14.99999999999998579 ) ) ;
#23140 = EDGE_LOOP ( 'NONE', ( #15658, #1782 ) ) ;
#23141 = DIRECTION ( 'NONE',  ( 0.000000000000000000, 0.000000000000000000, -1.000000000000000000 ) ) ;
#23142 = FACE_OUTER_BOUND ( 'NONE', #27709, .T. ) ;
#23143 = CARTESIAN_POINT ( 'NONE',  ( 98.15313185440923860, 93.24999999863439371, 4.458734124999980786 ) ) ;
#23144 = DIRECTION ( 'NONE',  ( 0.8660254037844404840, -0.000000000000000000, -0.4999999999999967804 ) ) ;
#23145 = DIRECTION ( 'NONE',  ( 0.000000000000000000, 1.000000000000000000, 0.000000000000000000 ) ) ;
#23146 = CARTESIAN_POINT ( 'NONE',  ( -9.598844408820458085, 32.16953124999999147, -9.598844408820458085 ) ) ;
#23147 = CARTESIAN_POINT ( 'NONE',  ( -13.14518615778179189, 31.87187500108393223, 5.444914386472304635 ) ) ;
#23148 = VERTEX_POINT ( 'NONE', #20205 ) ;
#23149 = CARTESIAN_POINT ( 'NONE',  ( 70.44491438647229131, 38.91640625108393436, -13.14518615778179722 ) ) ;
#23150 = CARTESIAN_POINT ( 'NONE',  ( 1.417506129906585004E-15, 52.00000000000000711, -11.57481594606304398 ) ) ;
#23151 = CIRCLE ( 'NONE', #12663, 11.50000000000001421 ) ;
#23152 = DIRECTION ( 'NONE',  ( -0.000000000000000000, 1.000000000000000000, -0.000000000000000000 ) ) ;
#23153 = ORIENTED_EDGE ( 'NONE', *, *, #27781, .F. ) ;
#23154 = DIRECTION ( 'NONE',  ( -0.8660254037844407060, 0.4999999999999963363, 0.000000000000000000 ) ) ;
#23155 = PRODUCT_DEFINITION_FORMATION_WITH_SPECIFIED_SOURCE ( 'ANY', '', #12815, .NOT_KNOWN. ) ;
#23156 = CARTESIAN_POINT ( 'NONE',  ( 0.000000000000000000, -7.395377635281828788, 13.57481594606304398 ) ) ;
#23157 = CARTESIAN_POINT ( 'NONE',  ( 124.3771271284221314, 35.69179687716786731, 13.57481594606304753 ) ) ;
#23158 = CARTESIAN_POINT ( 'NONE',  ( 99.99999999999998579, 124.1000000021849416, -2.499999999999997780 ) ) ;
#23159 = LINE ( 'NONE', #5773, #27758 ) ;
#23160 = CARTESIAN_POINT ( 'NONE',  ( 200.4449143864723055, 38.91640625108393436, -13.14518615778179900 ) ) ;
#23161 = EDGE_LOOP ( 'NONE', ( #9492, #318, #15507, #7243 ) ) ;
#23162 = B_SPLINE_CURVE_WITH_KNOTS ( 'NONE', 3,
 ( #21449, #14590, #21587, #19013, #17010, #23169 ),
 .UNSPECIFIED., .F., .F.,
 ( 4, 2, 4 ),
 ( 0.6250000000000000000, 0.6875000000000000000, 0.7500000000000000000 ),
 .UNSPECIFIED. ) ;
#23163 = FILL_AREA_STYLE ('',( #27582 ) ) ;
#23164 = CARTESIAN_POINT ( 'NONE',  ( 99.99999999999995737, 84.25000000000000000, 4.999999999999990230 ) ) ;
#23165 = CARTESIAN_POINT ( 'NONE',  ( 2.493653234604083739E-15, 39.61093749999999147, 13.57481594606304576 ) ) ;
#23166 = AXIS2_PLACEMENT_3D ( 'NONE', #17069, #2121, #6252 ) ;
#23167 = CARTESIAN_POINT ( 'NONE',  ( 0.000000000000000000, 40.99999999999999289, 0.000000000000000000 ) ) ;
#23168 = CARTESIAN_POINT ( 'NONE',  ( 9.598844408820459861, 34.25312500216787015, 9.598844408820456309 ) ) ;
#23169 = CARTESIAN_POINT ( 'NONE',  ( 102.4999999999999858, 123.0000000000000000, -8.724596124144689908E-15 ) ) ;
#23170 = CARTESIAN_POINT ( 'NONE',  ( -9.295050272127046043, 39.85898437608393152, -9.295050272127046043 ) ) ;
#23171 = CARTESIAN_POINT ( 'NONE',  ( 99.99999999999995737, 80.75000000000000000, -5.000000000000018652 ) ) ;
#23172 = VECTOR ( 'NONE', #23295, 1000.000000000000000 ) ;
#23173 = CARTESIAN_POINT ( 'NONE',  ( 99.99999999999995737, -4.999999999999990230, 6.249999999999998224 ) ) ;
#23174 = CARTESIAN_POINT ( 'NONE',  ( -8.312177448680279460E-16, 32.96328125216787441, -13.57481594606304576 ) ) ;
#23175 = FACE_OUTER_BOUND ( 'NONE', #26663, .T. ) ;
#23176 = ORIENTED_EDGE ( 'NONE', *, *, #25386, .F. ) ;
#23177 = CARTESIAN_POINT ( 'NONE',  ( 78.57481594606305464, 36.68398437500000142, -5.622872871577873966 ) ) ;
#23178 = PRODUCT_DEFINITION_CONTEXT ( 'detailed design', #3514, 'design' ) ;
#23179 =( BOUNDED_CURVE ( )  B_SPLINE_CURVE ( 2, ( #11308, #20171, #26590, #7038, #653, #7326, #26732, #11591, #20311 ),
 .UNSPECIFIED., .F., .T. ) 
 B_SPLINE_CURVE_WITH_KNOTS ( ( 3, 2, 2, 2, 3 ),
 ( 0.6071428571428570953, 0.6160714285714286031, 0.6250000000000000000, 0.6339285714285712858, 0.6428571428571427937 ),
 .UNSPECIFIED. ) 
 CURVE ( )  GEOMETRIC_REPRESENTATION_ITEM ( )  RATIONAL_B_SPLINE_CURVE ( ( 1.000000000000000000, 0.9238795325112867385, 1.000000000000000000, 0.9238795325112867385, 1.000000000000000000, 0.9238795325112867385, 1.000000000000000000, 0.9238795325112877377, 0.9999999999999990008 ) ) 
 REPRESENTATION_ITEM ( '' )  );
#23180 = CARTESIAN_POINT ( 'NONE',  ( -13.57481594606304753, 39.36289062499999858, -5.622872871577873077 ) ) ;
#23181 = CARTESIAN_POINT ( 'NONE',  ( -13.14518615778179900, 39.71015625108393010, -5.444914386472297529 ) ) ;
#23182 = CARTESIAN_POINT ( 'NONE',  ( 96.46446609406721961, 3.535533905932755072, 4.000000002731185056 ) ) ;
#23183 = CARTESIAN_POINT ( 'NONE',  ( 116.8548138422182063, 40.00781250108393294, 5.444914386472304635 ) ) ;
#23184 = CARTESIAN_POINT ( 'NONE',  ( 55.70494972787295751, 37.47773437608393010, 9.295050272127047819 ) ) ;
#23185 = EDGE_CURVE ( 'NONE', #14316, #21981, #9649, .T. ) ;
#23186 = DIRECTION ( 'NONE',  ( 0.000000000000000000, -0.000000000000000000, 1.000000000000000000 ) ) ;
#23187 = CARTESIAN_POINT ( 'NONE',  ( -13.14518615778179189, 34.25312500108393010, 5.444914386472304635 ) ) ;
#23188 = CARTESIAN_POINT ( 'NONE',  ( 104.9999999999999716, 1.449011120738813565E-14, 9.625000002731184168 ) ) ;
#23189 = CARTESIAN_POINT ( 'NONE',  ( 99.99999999999998579, 123.7000000021849502, 2.499999999999978684 ) ) ;
#23190 = DIRECTION ( 'NONE',  ( -0.000000000000000000, -1.000000000000000000, -0.000000000000000000 ) ) ;
#23191 = CARTESIAN_POINT ( 'NONE',  ( 130.0000000000000000, 40.00781250000000000, -13.57481594606304576 ) ) ;
#23192 = CARTESIAN_POINT ( 'NONE',  ( 130.0000000000000000, 37.22968749999999716, 13.57481594606304576 ) ) ;
#23193 = COLOUR_RGB ( '', 0.31764706, 0.68627451, 0.89019608) ;
#23194 = CARTESIAN_POINT ( 'NONE',  ( -5.444914386472297529, 38.02343750108394005, -13.14518615778179900 ) ) ;
#23195 = PLANE ( 'NONE',  #25651 ) ;
#23196 = CARTESIAN_POINT ( 'NONE',  ( 101.0355339059327378, 123.1569999999781402, -2.499999999999997780 ) ) ;
#23197 = AXIS2_PLACEMENT_3D ( 'NONE', #3012, #9138, #6992 ) ;
#23198 = CARTESIAN_POINT ( 'NONE',  ( 102.0669872999999939, 123.5000000010924595, 0.8561741729129311862 ) ) ;
#23199 = DIRECTION ( 'NONE',  ( 0.000000000000000000, 0.000000000000000000, -1.000000000000000000 ) ) ;
#23200 = FACE_OUTER_BOUND ( 'NONE', #5896, .T. ) ;
#23201 = CARTESIAN_POINT ( 'NONE',  ( 104.4587341249999781, -1.846868145590721655, 12.87500000136559208 ) ) ;
#23202 = CARTESIAN_POINT ( 'NONE',  ( -8.312177448680279460E-16, 33.75703125216787726, -13.57481594606304576 ) ) ;
#23203 = CARTESIAN_POINT ( 'NONE',  ( 102.1631189606246295, 103.3426043859339103, -49.89999999453763735 ) ) ;
#23204 = CARTESIAN_POINT ( 'NONE',  ( -13.57481594606304753, 40.95039062499999005, -5.622872871577873077 ) ) ;
#23205 = CARTESIAN_POINT ( 'NONE',  ( -8.049105076161786076E-16, 33.21132812608393436, -13.14518615778179544 ) ) ;
#23206 = CARTESIAN_POINT ( 'NONE',  ( -8.312177448680279460E-16, 32.96328125216787441, -13.57481594606304576 ) ) ;
#23207 = CARTESIAN_POINT ( 'NONE',  ( 97.71650635000000307, 124.4250000016387219, -9.540979117872439019E-15 ) ) ;
#23208 = CARTESIAN_POINT ( 'NONE',  ( 101.8468681455906903, 83.37500000136563472, -4.458734125000016313 ) ) ;
#23209 = CARTESIAN_POINT ( 'NONE',  ( 70.44491438647230552, 39.41250000108393436, 13.14518615778179189 ) ) ;
#23210 = CARTESIAN_POINT ( 'NONE',  ( 102.4976396683250925, 117.6869444889999841, -47.97500000273119269 ) ) ;
#23211 = CARTESIAN_POINT ( 'NONE',  ( 104.9999999999999858, 94.00000000000000000, -6.938893903907228378E-15 ) ) ;
#23212 = FACE_OUTER_BOUND ( 'NONE', #14704, .T. ) ;
#23213 = CARTESIAN_POINT ( 'NONE',  ( 99.99999999999998579, 89.99899999999999523, -9.540979117872439019E-15 ) ) ;
#23214 = CARTESIAN_POINT ( 'NONE',  ( 105.6631189606246295, 105.8855032339526758, -51.69999999453764161 ) ) ;
#23215 = CARTESIAN_POINT ( 'NONE',  ( 124.3771271284221314, 40.05742187499999574, -13.57481594606304753 ) ) ;
#23216 = ORIENTED_EDGE ( 'NONE', *, *, #4427, .F. ) ;
#23217 = CARTESIAN_POINT ( 'NONE',  ( 105.6631189606246295, 105.8855032339526758, -51.69999999453764161 ) ) ;
#23218 = CARTESIAN_POINT ( 'NONE',  ( -13.14518615778179189, 40.00781250108393294, 5.444914386472304635 ) ) ;
#23219 = CARTESIAN_POINT ( 'NONE',  ( 5.622872871577878406, 38.96601562716787015, 13.57481594606304576 ) ) ;
#23220 = CARTESIAN_POINT ( 'NONE',  ( 116.8548138422182205, 38.96601562608393721, 0.000000000000000000 ) ) ;
#23221 = CARTESIAN_POINT ( 'NONE',  ( 78.57481594606304043, 38.37070312716786447, -5.622872871577873077 ) ) ;
#23222 = EDGE_CURVE ( 'NONE', #13505, #2344, #14708, .T. ) ;
#23223 = CARTESIAN_POINT ( 'NONE',  ( 104.9952793366501709, 116.8754121666685393, -54.32499999726881867 ) ) ;
#23224 = CARTESIAN_POINT ( 'NONE',  ( -5.622872871577873077, 34.89804687716787868, 13.57481594606304753 ) ) ;
#23225 = ORIENTED_EDGE ( 'NONE', *, *, #8793, .T. ) ;
#23226 = CARTESIAN_POINT ( 'NONE',  ( 96.46446609406721961, -3.535533905932727539, 11.12500000000000000 ) ) ;
#23227 = CARTESIAN_POINT ( 'NONE',  ( 93.00000000000002842, 112.2744378736303474, -46.60000000546238397 ) ) ;
#23228 = CARTESIAN_POINT ( 'NONE',  ( -9.295050272127044266, 32.91367187608393152, 9.295050272127047819 ) ) ;
#23229 = CARTESIAN_POINT ( 'NONE',  ( 195.0000000000000000, 32.16953125216787157, -13.57481594606304576 ) ) ;
#23230 = DIRECTION ( 'NONE',  ( 0.000000000000000000, 0.000000000000000000, 1.000000000000000000 ) ) ;
#23231 = CARTESIAN_POINT ( 'NONE',  ( 139.2950502721270425, 39.46210937608393010, -9.295050272127046043 ) ) ;
#23232 = CARTESIAN_POINT ( 'NONE',  ( -9.295050272127046043, 32.71523437608393436, -9.295050272127046043 ) ) ;
#23233 = CARTESIAN_POINT ( 'NONE',  ( 99.99999999999995737, -4.999999999999990230, 11.25000000000000000 ) ) ;
#23234 = DIRECTION ( 'NONE',  ( -2.385244779468110248E-16, 0.000000000000000000, -1.000000000000000000 ) ) ;
#23235 = CARTESIAN_POINT ( 'NONE',  ( 99.99999999999998579, 101.5015231886685712, -52.87500000273119838 ) ) ;
#23236 = CARTESIAN_POINT ( 'NONE',  ( 97.93301269999999192, 123.1000000010924822, -0.8561741729129505041 ) ) ;
#23237 = CARTESIAN_POINT ( 'NONE',  ( 181.4251840539369596, 37.08085937499999574, 5.622872871577880183 ) ) ;
#23238 = SHAPE_DEFINITION_REPRESENTATION ( #18102, #26810 ) ;
#23239 = CARTESIAN_POINT ( 'NONE',  ( 65.00000000000000000, 39.21406249999999716, -13.57481594606304576 ) ) ;
#23240 = CARTESIAN_POINT ( 'NONE',  ( 103.1528011352953342, 3.152801135295383084, 1.312500001365592750 ) ) ;
#23241 = CARTESIAN_POINT ( 'NONE',  ( 51.85481384221820633, 38.17226562608393436, 0.000000000000000000 ) ) ;
#23242 = CARTESIAN_POINT ( 'NONE',  ( 101.8468681455907046, -4.458734124999987891, 4.750000001365592084 ) ) ;
#23243 = CARTESIAN_POINT ( 'NONE',  ( 94.33688103937537051, 114.1144967660473242, -50.70000000546238539 ) ) ;
#23244 = CARTESIAN_POINT ( 'NONE',  ( 99.99999999999998579, 94.31249999863440792, 4.458734124999981674 ) ) ;
#23245 = CARTESIAN_POINT ( 'NONE',  ( 103.5355339059327093, -3.535533905932726206, 4.374999999999999112 ) ) ;
#23246 = CARTESIAN_POINT ( 'NONE',  ( 120.4011555911795455, 39.31328124999999574, -9.598844408820458085 ) ) ;
#23247 = CARTESIAN_POINT ( 'NONE',  ( -5.622872871577873077, 39.56132812499999574, 13.57481594606304753 ) ) ;
#23248 = EDGE_LOOP ( 'NONE', ( #1470, #9443, #8830, #423 ) ) ;
#23249 = CARTESIAN_POINT ( 'NONE',  ( 95.54126587499996504, 81.68750000136559208, -1.387778780781445676E-14 ) ) ;
#23250 = ADVANCED_FACE ( 'NONE', ( #24628 ), #11631, .T. ) ;
#23251 = PRESENTATION_LAYER_ASSIGNMENT (  '', '', ( #18239 ) ) ;
#23252 = CARTESIAN_POINT ( 'NONE',  ( 104.4587341249999923, 91.37499999863439371, -1.846868145590737198 ) ) ;
#23253 = ORIENTED_EDGE ( 'NONE', *, *, #11918, .F. ) ;
#23254 = ORIENTED_EDGE ( 'NONE', *, *, #10156, .T. ) ;
#23255 = EDGE_CURVE ( 'NONE', #26813, #8417, #25321, .T. ) ;
#23256 = CYLINDRICAL_SURFACE ( 'NONE', #9502, 2.999999999999989786 ) ;
#23257 = CARTESIAN_POINT ( 'NONE',  ( 101.8468681455906903, -4.458734124999987891, 8.000000001365592084 ) ) ;
#23258 = ADVANCED_FACE ( 'NONE', ( #27611, #20638 ), #23195, .T. ) ;
#23259 = EDGE_LOOP ( 'NONE', ( #18269, #16928, #5871, #3127 ) ) ;
#23260 = CARTESIAN_POINT ( 'NONE',  ( 104.9952793366501851, 103.1245878333314323, -46.67500000273118843 ) ) ;
#23261 = CARTESIAN_POINT ( 'NONE',  ( -13.14518615778179544, 34.20351562608393436, 0.000000000000000000 ) ) ;
#23262 = CARTESIAN_POINT ( 'NONE',  ( 9.598844408820456309, 36.03906250216787299, -9.598844408820458085 ) ) ;
#23263 = CARTESIAN_POINT ( 'NONE',  ( -5.444914386472299306, 38.32109375108394289, 13.14518615778179722 ) ) ;
#23264 = EDGE_CURVE ( 'NONE', #18668, #17777, #16349, .T. ) ;
#23265 = CARTESIAN_POINT ( 'NONE',  ( 93.46109445667491400, 105.2492070361643215, -48.92500000273119554 ) ) ;
#23266 = CARTESIAN_POINT ( 'NONE',  ( 116.8548138422182205, 39.95820312608393010, 0.000000000000000000 ) ) ;
#23267 = CARTESIAN_POINT ( 'NONE',  ( 13.14518615778179544, 32.21914062608393436, -1.609821015232357215E-15 ) ) ;
#23268 = EDGE_LOOP ( 'NONE', ( #15134, #6787, #5197, #23402, #25244, #26841, #22581, #10539 ) ) ;
#23269 = CARTESIAN_POINT ( 'NONE',  ( 55.40115559117954547, 37.92421874999999432, 9.598844408820459861 ) ) ;
#23270 = DIRECTION ( 'NONE',  ( 5.782411586589357392E-17, -0.000000000000000000, 1.000000000000000000 ) ) ;
#23271 = EDGE_CURVE ( 'NONE', #17231, #21964, #20521, .T. ) ;
#23272 = CARTESIAN_POINT ( 'NONE',  ( 94.33688103937535629, 105.8855032339526758, -50.80000000000001137 ) ) ;
#23273 = CARTESIAN_POINT ( 'NONE',  ( 96.84719886470459471, 3.152801135295383084, 2.312500001365592084 ) ) ;
#23274 = CARTESIAN_POINT ( 'NONE',  ( 97.92893218813451028, 5.000000000000018652, 3.937500002731185056 ) ) ;
#23275 = CARTESIAN_POINT ( 'NONE',  ( 99.99999999999995737, -4.458734124999988779, 3.937500001365591640 ) ) ;
#23276 = CARTESIAN_POINT ( 'NONE',  ( 103.1528011352953342, 82.06250000136559208, 3.152801135295355106 ) ) ;
#23277 = CARTESIAN_POINT ( 'NONE',  ( -13.14518615778179544, 34.20351562608393436, 0.000000000000000000 ) ) ;
#23278 = CARTESIAN_POINT ( 'NONE',  ( 13.14518615778179900, 39.51171875108392584, 5.444914386472293977 ) ) ;
#23279 = ADVANCED_FACE ( 'NONE', ( #22780 ), #7799, .T. ) ;
#23280 = AXIS2_PLACEMENT_3D ( 'NONE', #23503, #10514, #25633 ) ;
#23281 = CARTESIAN_POINT ( 'NONE',  ( 99.99999999999995737, 1.387778780781445676E-14, 34.79898987322334136 ) ) ;
#23282 = ORIENTED_EDGE ( 'NONE', *, *, #17680, .T. ) ;
#23283 = CARTESIAN_POINT ( 'NONE',  ( 100.8561741729129437, 124.0000000010925021, 2.066987299999979655 ) ) ;
#23284 = CYLINDRICAL_SURFACE ( 'NONE', #7105, 5.000000000000004441 ) ;
#23285 = CARTESIAN_POINT ( 'NONE',  ( 106.5389055433250860, 105.2492070361643215, -55.07499999726882578 ) ) ;
#23286 = EDGE_CURVE ( 'NONE', #1089, #17753, #21187, .T. ) ;
#23287 = CARTESIAN_POINT ( 'NONE',  ( 96.46446609406726225, 93.62500000000000000, 3.535533905932723986 ) ) ;
#23288 = ORIENTED_EDGE ( 'NONE', *, *, #112, .F. ) ;
#23289 = CARTESIAN_POINT ( 'NONE',  ( 78.14518615778180788, 39.61093750108393863, -5.444914386472297529 ) ) ;
#23290 = DIRECTION ( 'NONE',  ( 1.000000000000000000, 0.000000000000000000, -0.000000000000000000 ) ) ;
#23291 = DIRECTION ( 'NONE',  ( -1.000000000000000000, 0.000000000000000000, 0.000000000000000000 ) ) ;
#23292 = ORIENTED_EDGE ( 'NONE', *, *, #27456, .T. ) ;
#23293 = CARTESIAN_POINT ( 'NONE',  ( 93.00000000000000000, 110.0000000000000000, -54.00000000000000711 ) ) ;
#23294 = EDGE_CURVE ( 'NONE', #5694, #18097, #9791, .T. ) ;
#23295 = DIRECTION ( 'NONE',  ( -0.000000000000000000, 1.000000000000000000, -0.000000000000000000 ) ) ;
#23296 = DIRECTION ( 'NONE',  ( -1.000000000000000000, 0.000000000000000000, 0.000000000000000000 ) ) ;
#23297 = EDGE_CURVE ( 'NONE', #11152, #8293, #919, .T. ) ;
#23298 = CARTESIAN_POINT ( 'NONE',  ( 124.3771271284221314, 33.01289062716787726, -13.57481594606304753 ) ) ;
#23299 =( BOUNDED_CURVE ( )  B_SPLINE_CURVE ( 2, ( #15638, #24766, #5247, #15909, #13485, #11207, #7220, #24339, #982 ),
 .UNSPECIFIED., .F., .F. ) 
 B_SPLINE_CURVE_WITH_KNOTS ( ( 3, 2, 2, 2, 3 ),
 ( 0.5714285714285713969, 0.5803571428571429047, 0.5892857142857143016, 0.5982142857142856984, 0.6071428571428570953 ),
 .UNSPECIFIED. ) 
 CURVE ( )  GEOMETRIC_REPRESENTATION_ITEM ( )  RATIONAL_B_SPLINE_CURVE ( ( 1.000000000000000000, 0.9238795325112867385, 1.000000000000000000, 0.9238795325112867385, 1.000000000000000000, 0.9238795325112867385, 1.000000000000000000, 0.9238795325112867385, 1.000000000000000000 ) ) 
 REPRESENTATION_ITEM ( '' )  );
#23300 = CARTESIAN_POINT ( 'NONE',  ( 99.99999999999998579, 130.0000000000000000, -5.204170427930421283E-15 ) ) ;
#23301 = DIRECTION ( 'NONE',  ( -1.000000000000000000, 0.000000000000000000, 0.000000000000000000 ) ) ;
#23302 = CARTESIAN_POINT ( 'NONE',  ( 185.7049497278729575, 36.68398437608393436, -9.295050272127046043 ) ) ;
#23303 = ORIENTED_EDGE ( 'NONE', *, *, #22909, .F. ) ;
#23304 = VERTEX_POINT ( 'NONE', #10894 ) ;
#23305 = SURFACE_SIDE_STYLE ('',( #3639 ) ) ;
#23306 = CARTESIAN_POINT ( 'NONE',  ( 130.0000000000000000, -7.395377635281828788, 13.57481594606302799 ) ) ;
#23307 = CARTESIAN_POINT ( 'NONE',  ( 99.99999999999998579, 92.62499999726881583, 4.999999999999984013 ) ) ;
#23308 = CARTESIAN_POINT ( 'NONE',  ( 107.0000000000000284, 107.7255621263696952, -51.60000000546238397 ) ) ;
#23309 = DIRECTION ( 'NONE',  ( -5.782411586589357392E-17, 0.000000000000000000, -1.000000000000000000 ) ) ;
#23310 = CARTESIAN_POINT ( 'NONE',  ( 0.000000000000000000, 40.99999999999999289, 0.000000000000000000 ) ) ;
#23311 = CARTESIAN_POINT ( 'NONE',  ( 102.2113248666666436, 122.8333333340616491, -9.811788309856265935E-15 ) ) ;
#23312 = CARTESIAN_POINT ( 'NONE',  ( 9.031440422454179995, 36.00000000000002132, 9.765766397119126196 ) ) ;
#23313 = DIRECTION ( 'NONE',  ( 0.000000000000000000, 0.000000000000000000, -1.000000000000000000 ) ) ;
#23314 = CARTESIAN_POINT ( 'NONE',  ( 99.99999999999997158, 118.4984768113314004, -46.12499999726880873 ) ) ;
#23315 = EDGE_LOOP ( 'NONE', ( #16195, #12013, #13153, #19155 ) ) ;
#23316 = CARTESIAN_POINT ( 'NONE',  ( 9.598844408820459861, 40.50390624999999289, 9.598844408820456309 ) ) ;
#23317 = CARTESIAN_POINT ( 'NONE',  ( -13.57481594606304576, 31.62382812716787228, 5.622872871577880183 ) ) ;
#23318 = CARTESIAN_POINT ( 'NONE',  ( 94.99999999999995737, -2.071067811865466624, 4.187500002731185056 ) ) ;
#23319 = CARTESIAN_POINT ( 'NONE',  ( 143.1451861577818079, 39.56132812608393579, -1.609821015232357215E-15 ) ) ;
#23320 = CARTESIAN_POINT ( 'NONE',  ( 70.44491438647230552, 36.33671875108394289, -13.14518615778179900 ) ) ;
#23321 = EDGE_CURVE ( 'NONE', #2000, #11798, #13265, .T. ) ;
#23322 = CARTESIAN_POINT ( 'NONE',  ( 52.62412159965071368, 36.00000000000000000, 4.513979326318426466 ) ) ;
#23323 = CARTESIAN_POINT ( 'NONE',  ( -13.14518615778179900, 35.74140625108393721, -5.444914386472297529 ) ) ;
#23324 = CARTESIAN_POINT ( 'NONE',  ( 190.5405265863611817, 36.00000000000001421, -12.68347323196760890 ) ) ;
#23325 = CARTESIAN_POINT ( 'NONE',  ( 104.9999999999999716, 1.449011120738813565E-14, 9.625000002731184168 ) ) ;
#23326 = CARTESIAN_POINT ( 'NONE',  ( 97.50000000000000000, 125.0000000000000000, -9.540979117872439019E-15 ) ) ;
#23327 = CARTESIAN_POINT ( 'NONE',  ( -5.444914386472297529, 39.61093750108393152, -13.14518615778179900 ) ) ;
#23328 = CARTESIAN_POINT ( 'NONE',  ( 142.0772764098356333, 36.00000000000000000, -6.197985357349214297 ) ) ;
#23329 = CARTESIAN_POINT ( 'NONE',  ( 97.50000000000000000, 123.3999999999999915, -9.540979117872439019E-15 ) ) ;
#23330 = LINE ( 'NONE', #8348, #22331 ) ;
#23331 = CARTESIAN_POINT ( 'NONE',  ( 101.4615807364564546, 124.2500000010924737, 1.461580736456455476 ) ) ;
#23332 = CYLINDRICAL_SURFACE ( 'NONE', #11800, 5.000000000000004441 ) ;
#23333 = CARTESIAN_POINT ( 'NONE',  ( 101.8468681455906903, -4.458734124999987891, 12.75000000136559386 ) ) ;
#23334 = CARTESIAN_POINT ( 'NONE',  ( -13.57481594606304576, 32.26874999999999716, 0.000000000000000000 ) ) ;
#23335 = ORIENTED_EDGE ( 'NONE', *, *, #8087, .T. ) ;
#23336 = CARTESIAN_POINT ( 'NONE',  ( 0.000000000000000000, 36.00000000000000000, 0.000000000000000000 ) ) ;
#23337 = CARTESIAN_POINT ( 'NONE',  ( -9.295050272127044266, 32.11992187608393579, 9.295050272127047819 ) ) ;
#23338 = CARTESIAN_POINT ( 'NONE',  ( -9.295050272127044266, 33.50898437608393010, 9.295050272127047819 ) ) ;
#23339 = CIRCLE ( 'NONE', #16502, 11.57481594606304398 ) ;
#23340 = CARTESIAN_POINT ( 'NONE',  ( -13.57481594606304753, 31.52460937716787370, -5.622872871577873077 ) ) ;
#23341 = CARTESIAN_POINT ( 'NONE',  ( 181.4251840539369596, 36.33671875216787583, 0.000000000000000000 ) ) ;
#23342 = CARTESIAN_POINT ( 'NONE',  ( 95.54126587499995082, 84.62500000136560629, -1.846868145590750077 ) ) ;
#23343 = CARTESIAN_POINT ( 'NONE',  ( 59.55508561352770158, 39.80937500108392868, -13.14518615778179900 ) ) ;
#23344 =( BOUNDED_CURVE ( )  B_SPLINE_CURVE ( 2, ( #14035, #3360, #12031, #20754, #22760, #3646, #9485, #817, #18187 ),
 .UNSPECIFIED., .F., .F. ) 
 B_SPLINE_CURVE_WITH_KNOTS ( ( 3, 2, 2, 2, 3 ),
 ( 0.06250000000000004163, 0.07291666666666665741, 0.08333333333333325932, 0.09374999999999987510, 0.1041666666666664909 ),
 .UNSPECIFIED. ) 
 CURVE ( )  GEOMETRIC_REPRESENTATION_ITEM ( )  RATIONAL_B_SPLINE_CURVE ( ( 0.9999999999999996669, 0.9238795325112870716, 1.000000000000000000, 0.9238795325112867385, 1.000000000000000000, 0.9238795325112867385, 1.000000000000000000, 0.9238795325112880708, 0.9999999999999986677 ) ) 
 REPRESENTATION_ITEM ( '' )  );
#23345 = CARTESIAN_POINT ( 'NONE',  ( 93.46109445667491400, 114.7507929638356785, -49.57500000273120122 ) ) ;
#23346 = CYLINDRICAL_SURFACE ( 'NONE', #20964, 13.57481594606304398 ) ;
#23347 = CARTESIAN_POINT ( 'NONE',  ( 102.0669872999999939, 123.6000000010924680, -0.8561741729129507261 ) ) ;
#23348 = CARTESIAN_POINT ( 'NONE',  ( -8.312177448680279460E-16, 40.80156249999999574, -13.57481594606304576 ) ) ;
#23349 = CARTESIAN_POINT ( 'NONE',  ( 107.0000000000000000, 112.2744378736303332, -53.39999999453764445 ) ) ;
#23350 = CARTESIAN_POINT ( 'NONE',  ( 116.4251840539369596, 39.41249999999999432, 0.000000000000000000 ) ) ;
#23351 = ORIENTED_EDGE ( 'NONE', *, *, #6697, .T. ) ;
#23352 = CARTESIAN_POINT ( 'NONE',  ( 97.92893218813451028, 5.000000000000018652, 7.812499999999999112 ) ) ;
#23353 = CARTESIAN_POINT ( 'NONE',  ( -9.295050272127044266, 39.26367187608393294, 9.295050272127047819 ) ) ;
#23354 = CARTESIAN_POINT ( 'NONE',  ( 104.4587341249999639, 80.93750000136559208, -1.442382525525748735E-14 ) ) ;
#23355 = CARTESIAN_POINT ( 'NONE',  ( 135.4449143864723055, 40.00781250108393294, 13.14518615778179189 ) ) ;
#23356 = CARTESIAN_POINT ( 'NONE',  ( 51.42518405393695957, 37.08085937716786873, -5.622872871577873077 ) ) ;
#23357 = CARTESIAN_POINT ( 'NONE',  ( 99.99999999999997158, 118.4984768113314004, -54.12499999726881583 ) ) ;
#23358 = CARTESIAN_POINT ( 'NONE',  ( -5.622872871577873077, 36.48554687716787015, 13.57481594606304753 ) ) ;
#23359 = EDGE_LOOP ( 'NONE', ( #16125, #4751, #24060, #11124 ) ) ;
#23360 = AXIS2_PLACEMENT_3D ( 'NONE', #23413, #25127, #10277 ) ;
#23361 = CARTESIAN_POINT ( 'NONE',  ( 104.9999999999999574, -2.071067811865462627, 8.437500000000000000 ) ) ;
#23362 = CARTESIAN_POINT ( 'NONE',  ( 107.0000000000000142, 110.0000000000000000, -53.00000000000000711 ) ) ;
#23363 = CARTESIAN_POINT ( 'NONE',  ( -9.295050272127046043, 31.92148437608393508, -9.295050272127046043 ) ) ;
#23364 = CARTESIAN_POINT ( 'NONE',  ( 195.0000000000000000, 38.76757812608393294, -13.14518615778179544 ) ) ;
#23365 = DIRECTION ( 'NONE',  ( 5.782411586589358625E-17, -0.000000000000000000, 1.000000000000000000 ) ) ;
#23366 = CARTESIAN_POINT ( 'NONE',  ( 116.8548138422182205, 38.17226562608393436, 0.000000000000000000 ) ) ;
#23367 = LINE ( 'NONE', #8666, #20081 ) ;
#23368 = CARTESIAN_POINT ( 'NONE',  ( 139.5988444088204687, 37.32890624999999574, 9.598844408820456309 ) ) ;
#23369 = CARTESIAN_POINT ( 'NONE',  ( 103.1528011352953484, 93.43749999863440792, -3.152801135295366208 ) ) ;
#23370 = CYLINDRICAL_SURFACE ( 'NONE', #20272, 13.57481594606304398 ) ;
#23371 = CARTESIAN_POINT ( 'NONE',  ( -8.049105076161786076E-16, 39.56132812608393579, -13.14518615778179544 ) ) ;
#23372 = CARTESIAN_POINT ( 'NONE',  ( 195.0000000000000000, 37.62656249999999858, -13.57481594606304576 ) ) ;
#23373 = CONTEXT_DEPENDENT_SHAPE_REPRESENTATION ( #14763, #22434 ) ;
#23374 = DIRECTION ( 'NONE',  ( -1.000000000000000000, 0.000000000000000000, 0.000000000000000000 ) ) ;
#23375 = CARTESIAN_POINT ( 'NONE',  ( 104.4587341249999639, 1.442382525525748735E-14, 3.187500001365592972 ) ) ;
#23376 = CARTESIAN_POINT ( 'NONE',  ( 51.85481384221819923, 39.71015625108393010, -5.444914386472297529 ) ) ;
#23377 = EDGE_CURVE ( 'NONE', #27310, #4145, #1098, .T. ) ;
#23378 = CARTESIAN_POINT ( 'NONE',  ( 96.84719886470459471, 3.152801135295383084, 6.312500001365592084 ) ) ;
#23379 = CARTESIAN_POINT ( 'NONE',  ( 105.6631189606246295, 114.1144967660473242, -49.30000000546237970 ) ) ;
#23380 = CARTESIAN_POINT ( 'NONE',  ( 95.54126587500000767, 95.06249999863440792, -7.484931351350258973E-15 ) ) ;
#23381 = DIRECTION ( 'NONE',  ( -1.000000000000000000, 0.000000000000000000, 0.000000000000000000 ) ) ;
#23382 = CARTESIAN_POINT ( 'NONE',  ( 2.493653234604083739E-15, 39.61093749999999147, 13.57481594606304576 ) ) ;
#23383 = DIRECTION ( 'NONE',  ( -5.782411586589357392E-17, 0.000000000000000000, -1.000000000000000000 ) ) ;
#23384 = ORIENTED_EDGE ( 'NONE', *, *, #18989, .T. ) ;
#23385 = CARTESIAN_POINT ( 'NONE',  ( 96.84719886470459471, 82.81250000136560629, 3.152801135295355994 ) ) ;
#23386 = AXIS2_PLACEMENT_3D ( 'NONE', #16802, #20679, #7834 ) ;
#23387 = CARTESIAN_POINT ( 'NONE',  ( 95.54126587499999346, 90.74999999863439371, -1.846868145590737864 ) ) ;
#23388 = ORIENTED_EDGE ( 'NONE', *, *, #23138, .F. ) ;
#23389 = DIRECTION ( 'NONE',  ( -0.000000000000000000, -1.000000000000000000, -0.000000000000000000 ) ) ;
#23390 = ORIENTED_EDGE ( 'NONE', *, *, #20317, .T. ) ;
#23391 = CARTESIAN_POINT ( 'NONE',  ( 2.493653234604083739E-15, 33.36015625216786873, 13.57481594606304576 ) ) ;
#23392 = CARTESIAN_POINT ( 'NONE',  ( 99.99999999999995737, -4.458734124999988779, 6.937500001365592972 ) ) ;
#23393 = EDGE_LOOP ( 'NONE', ( #28059, #12684, #17665, #16772 ) ) ;
#23394 = CARTESIAN_POINT ( 'NONE',  ( -5.444914386472297529, 35.04687500108393294, -13.14518615778179722 ) ) ;
#23395 = CARTESIAN_POINT ( 'NONE',  ( -13.14518615778179544, 32.61601562608393579, 0.000000000000000000 ) ) ;
#23396 = CARTESIAN_POINT ( 'NONE',  ( 200.6228728715778686, 39.26367187716787299, -13.57481594606304753 ) ) ;
#23397 = CARTESIAN_POINT ( 'NONE',  ( 9.295050272127046043, 38.66835937608393436, -9.295050272127046043 ) ) ;
#23398 = CARTESIAN_POINT ( 'NONE',  ( 106.5389055433251002, 105.2492070361643215, -44.32500000273119412 ) ) ;
#23399 = CARTESIAN_POINT ( 'NONE',  ( 193.9858691739322012, 51.45790058219657936, 15.00000000000130029 ) ) ;
#23400 = CARTESIAN_POINT ( 'NONE',  ( 143.1451861577818363, 37.92421875108393436, 5.444914386472293977 ) ) ;
#23401 = CARTESIAN_POINT ( 'NONE',  ( 9.295050272127046043, 33.11210937608393579, -9.295050272127046043 ) ) ;
#23402 = ORIENTED_EDGE ( 'NONE', *, *, #20623, .F. ) ;
#23403 = CARTESIAN_POINT ( 'NONE',  ( 70.62287287157786864, 36.78320312499999289, -13.57481594606304753 ) ) ;
#23404 = FACE_OUTER_BOUND ( 'NONE', #23022, .T. ) ;
#23405 = CARTESIAN_POINT ( 'NONE',  ( 207.6678442549460328, 36.00000000000000711, 4.396229039743087874 ) ) ;
#23406 = CARTESIAN_POINT ( 'NONE',  ( 103.1528011352953342, -3.152801135295355106, 5.812500001365591196 ) ) ;
#23407 = CARTESIAN_POINT ( 'NONE',  ( -5.444914386472299306, 32.96328125108393436, 13.14518615778179722 ) ) ;
#23408 = CARTESIAN_POINT ( 'NONE',  ( 96.84719886470459471, -3.152801135295355994, 3.812500001365591640 ) ) ;
#23409 = EDGE_CURVE ( 'NONE', #4741, #10253, #23467, .T. ) ;
#23410 = CARTESIAN_POINT ( 'NONE',  ( 101.8468681455907046, 82.00000000136560629, 4.458734124999987891 ) ) ;
#23411 = CARTESIAN_POINT ( 'NONE',  ( 13.14518615778179900, 33.85625000108393579, -5.444914386472297529 ) ) ;
#23412 = CARTESIAN_POINT ( 'NONE',  ( 2.414731522848535132E-15, 38.56914062608393579, 13.14518615778179544 ) ) ;
#23413 = CARTESIAN_POINT ( 'NONE',  ( 100.0000000000000000, 110.0000000000000000, -55.00000000000000711 ) ) ;
#23414 = VERTEX_POINT ( 'NONE', #19602 ) ;
#23415 = EDGE_CURVE ( 'NONE', #22018, #10089, #26017, .T. ) ;
#23416 = DIRECTION ( 'NONE',  ( 0.000000000000000000, -1.000000000000000000, 0.000000000000000000 ) ) ;
#23417 = CARTESIAN_POINT ( 'NONE',  ( 2.493653234604083739E-15, 39.71015625216787015, 13.57481594606304576 ) ) ;
#23418 = CARTESIAN_POINT ( 'NONE',  ( 95.54126587499999346, 93.99999999863439371, -1.846868145590737864 ) ) ;
#23419 = CARTESIAN_POINT ( 'NONE',  ( 65.00000000000000000, 38.12265625216787157, 13.57481594606304576 ) ) ;
#23420 = CARTESIAN_POINT ( 'NONE',  ( 101.0282581911821040, 123.0000000000000142, -2.018985708853541894 ) ) ;
#23421 = CARTESIAN_POINT ( 'NONE',  ( -5.622872871577873966, 32.11992187499999574, -13.57481594606304753 ) ) ;
#23422 = EDGE_LOOP ( 'NONE', ( #13824, #14831, #10288, #4846 ) ) ;
#23423 = CARTESIAN_POINT ( 'NONE',  ( 51.85481384221820633, 37.52734375108393294, -5.444914386472297529 ) ) ;
#23424 = FACE_OUTER_BOUND ( 'NONE', #13946, .T. ) ;
#23425 = EDGE_CURVE ( 'NONE', #14663, #24847, #14886, .T. ) ;
#23426 = CARTESIAN_POINT ( 'NONE',  ( 195.0000000000000000, -7.395377635281828788, -2.255140518769849538E-14 ) ) ;
#23427 = ORIENTED_EDGE ( 'NONE', *, *, #24668, .T. ) ;
#23428 = CARTESIAN_POINT ( 'NONE',  ( 95.00000000000000000, 92.50000000000000000, -7.551217303480904118E-15 ) ) ;
#23429 = AXIS2_PLACEMENT_3D ( 'NONE', #9744, #12805, #19244 ) ;
#23430 = CARTESIAN_POINT ( 'NONE',  ( 84.99999999999998579, 97.00000000000000000, 14.99999999999999467 ) ) ;
#23431 = CARTESIAN_POINT ( 'NONE',  ( 98.53841926354351699, 124.0500000010924708, 1.461580736456455920 ) ) ;
#23432 = CARTESIAN_POINT ( 'NONE',  ( 116.4251840539369596, 34.74921875216787726, 0.000000000000000000 ) ) ;
#23433 = CARTESIAN_POINT ( 'NONE',  ( 51.85481384221820633, 40.75195312608393294, 0.000000000000000000 ) ) ;
#23434 = CARTESIAN_POINT ( 'NONE',  ( 87.00000000000000000, 95.00000000000000000, 12.99999999999999467 ) ) ;
#23435 = CARTESIAN_POINT ( 'NONE',  ( 185.7049497278729575, 37.47773437608393010, -9.295050272127046043 ) ) ;
#23436 = EDGE_LOOP ( 'NONE', ( #9128, #22295, #2643, #27943 ) ) ;
#23437 = ORIENTED_EDGE ( 'NONE', *, *, #15861, .T. ) ;
#23438 = CARTESIAN_POINT ( 'NONE',  ( 13.14518615778179900, 34.55078125108393294, 5.444914386472293977 ) ) ;
#23439 = CARTESIAN_POINT ( 'NONE',  ( 98.15313185440923860, -4.458734124999987891, 13.87500000136559208 ) ) ;
#23440 = EDGE_CURVE ( 'NONE', #1596, #18580, #23842, .T. ) ;
#23441 = CARTESIAN_POINT ( 'NONE',  ( -8.312177448680279460E-16, 40.00781250000000000, -13.57481594606304576 ) ) ;
#23442 = DIRECTION ( 'NONE',  ( -0.000000000000000000, 1.000000000000000000, -0.000000000000000000 ) ) ;
#23443 = CARTESIAN_POINT ( 'NONE',  ( 102.0669872999999797, 122.6833333344258108, -9.794112055954758880E-15 ) ) ;
#23444 = LINE ( 'NONE', #3922, #8610 ) ;
#23445 = DIRECTION ( 'NONE',  ( 0.000000000000000000, -1.000000000000000000, 0.000000000000000000 ) ) ;
#23446 = CIRCLE ( 'NONE', #22541, 16.91709623134523000 ) ;
#23447 = DIRECTION ( 'NONE',  ( 0.000000000000000000, 1.000000000000000000, 0.000000000000000000 ) ) ;
#23448 = CARTESIAN_POINT ( 'NONE',  ( 102.0710678118654187, 94.06249999726881583, -5.000000000000031974 ) ) ;
#23449 = CARTESIAN_POINT ( 'NONE',  ( 104.9952793366501709, 103.1245878333314323, -46.92499999726882010 ) ) ;
#23450 = ADVANCED_FACE ( 'NONE', ( #26157, #6625 ), #25881, .F. ) ;
#23451 = EDGE_LOOP ( 'NONE', ( #15439, #6153, #12363, #5974 ) ) ;
#23452 = CARTESIAN_POINT ( 'NONE',  ( 5.622872871577871301, 39.95820312499999716, -13.57481594606304753 ) ) ;
#23453 = CARTESIAN_POINT ( 'NONE',  ( -9.295050272127046043, 38.86679687608393863, -9.295050272127046043 ) ) ;
#23454 = CARTESIAN_POINT ( 'NONE',  ( 101.8468681455906903, 4.458734125000016313, 14.12500000136559208 ) ) ;
#23455 = CARTESIAN_POINT ( 'NONE',  ( 120.7049497278729575, 38.46992187608393721, 9.295050272127047819 ) ) ;
#23456 = CARTESIAN_POINT ( 'NONE',  ( 78.14518615778179367, 36.98164062608393010, -1.609821015232357215E-15 ) ) ;
#23457 = EDGE_CURVE ( 'NONE', #3371, #19109, #24591, .T. ) ;
#23458 = CARTESIAN_POINT ( 'NONE',  ( 181.8548138422181921, 40.70234375108393721, -5.444914386472297529 ) ) ;
#23459 = CARTESIAN_POINT ( 'NONE',  ( 95.27063293749995410, 79.84375000068280315, -1.387778780781445676E-14 ) ) ;
#23460 = CARTESIAN_POINT ( 'NONE',  ( 2.414731522848535132E-15, 35.98945312608393010, 13.14518615778179544 ) ) ;
#23461 = CARTESIAN_POINT ( 'NONE',  ( 104.9999999999999716, -2.071067811865452857, 9.562500002731184168 ) ) ;
#23462 =( BOUNDED_CURVE ( )  B_SPLINE_CURVE ( 2, ( #22657, #4986, #11935, #5264, #16366, #11507, #3267, #2975, #26939 ),
 .UNSPECIFIED., .F., .F. ) 
 B_SPLINE_CURVE_WITH_KNOTS ( ( 3, 2, 2, 2, 3 ),
 ( 0.3541666666666666852, 0.3645833333333332593, 0.3749999999999998890, 0.3854166666666665741, 0.3958333333333331483 ),
 .UNSPECIFIED. ) 
 CURVE ( )  GEOMETRIC_REPRESENTATION_ITEM ( )  RATIONAL_B_SPLINE_CURVE ( ( 1.000000000000000000, 0.9238795325112867385, 1.000000000000000000, 0.9238795325112867385, 1.000000000000000000, 0.9238795325112867385, 1.000000000000000000, 0.9238795325112879597, 0.9999999999999987788 ) ) 
 REPRESENTATION_ITEM ( '' )  );
#23463 = CARTESIAN_POINT ( 'NONE',  ( 96.46446609406721961, 3.535533905932755072, 10.00000000273118594 ) ) ;
#23464 = CARTESIAN_POINT ( 'NONE',  ( 120.4011555911795455, 40.30546874999999574, 9.598844408820459861 ) ) ;
#23465 = AXIS2_PLACEMENT_3D ( 'NONE', #15032, #1817, #12471 ) ;
#23466 = CARTESIAN_POINT ( 'NONE',  ( 5.444914386472302859, 40.00781250108393294, 13.14518615778179189 ) ) ;
#23467 = LINE ( 'NONE', #17320, #4726 ) ;
#23468 = CARTESIAN_POINT ( 'NONE',  ( 97.50000000000000000, 123.3499999999999943, -1.035533905932742416 ) ) ;
#23469 = CARTESIAN_POINT ( 'NONE',  ( 104.9999999999999716, -2.071067811865452857, 10.43749999999999822 ) ) ;
#23470 = CARTESIAN_POINT ( 'NONE',  ( 102.0669873000000081, 123.6000000010924680, -0.8561741729129508371 ) ) ;
#23471 = CARTESIAN_POINT ( 'NONE',  ( -13.57481594606304753, 36.98164062499999005, -5.622872871577872189 ) ) ;
#23472 = CARTESIAN_POINT ( 'NONE',  ( 95.54126587499995082, -1.846868145590724986, 12.50000000136559208 ) ) ;
#23473 = CARTESIAN_POINT ( 'NONE',  ( 92.99999999999998579, 110.0000000000000000, -145.0000000000000284 ) ) ;
#23474 = DIRECTION ( 'NONE',  ( 0.000000000000000000, 0.000000000000000000, -1.000000000000000000 ) ) ;
#23475 = CARTESIAN_POINT ( 'NONE',  ( 5.622872871577871301, 40.75195312500000711, -13.57481594606304753 ) ) ;
#23476 = CARTESIAN_POINT ( 'NONE',  ( -13.14518615778179189, 32.66562500108393863, 5.444914386472304635 ) ) ;
#23477 = CARTESIAN_POINT ( 'NONE',  ( 13.57481594606304931, 32.71523437716787441, 5.622872871577869525 ) ) ;
#23478 = CARTESIAN_POINT ( 'NONE',  ( 94.99999999999995737, 2.071067811865491493, 2.937499999999999112 ) ) ;
#23479 = CARTESIAN_POINT ( 'NONE',  ( 101.8468681455906903, 79.75000000136560629, 4.458734124999987891 ) ) ;
#23480 = CARTESIAN_POINT ( 'NONE',  ( 51.85481384221820633, 39.95820312608393010, 0.000000000000000000 ) ) ;
#23481 = CARTESIAN_POINT ( 'NONE',  ( 108.0825317500000153, 110.0000000000000000, -50.37500000273119127 ) ) ;
#23482 = CARTESIAN_POINT ( 'NONE',  ( 65.00000000000000000, -7.395377635281828788, -7.517135062566165128E-15 ) ) ;
#23483 = CARTESIAN_POINT ( 'NONE',  ( 195.0000000000000000, 52.00000000000000711, -2.255140518769849538E-14 ) ) ;
#23484 = CARTESIAN_POINT ( 'NONE',  ( 135.6228728715779255, 38.86679687500001279, 13.57481594606301023 ) ) ;
#23485 = CARTESIAN_POINT ( 'NONE',  ( 102.1631189606246295, 103.3426043859339103, -49.89999999453763735 ) ) ;
#23486 = CARTESIAN_POINT ( 'NONE',  ( 143.1451861577818079, 32.41757812608393863, -1.609821015232357215E-15 ) ) ;
#23487 = EDGE_CURVE ( 'NONE', #4009, #22191, #27884, .T. ) ;
#23488 = EDGE_LOOP ( 'NONE', ( #6595, #1186, #13132, #2321, #392, #19288, #13583, #7047, #4382, #8457, #6460, #22669 ) ) ;
#23489 = CARTESIAN_POINT ( 'NONE',  ( 99.99999999999998579, 123.0000000000000000, -0.5000000000000138778 ) ) ;
#23490 = CARTESIAN_POINT ( 'NONE',  ( -8.049105076161786076E-16, 38.96601562608393721, -13.14518615778179544 ) ) ;
#23491 = CARTESIAN_POINT ( 'NONE',  ( 98.15313185440925281, 81.25000000136560629, -4.458734125000016313 ) ) ;
#23492 = CARTESIAN_POINT ( 'NONE',  ( 139.2950502721270425, 40.25585937608393294, -9.295050272127046043 ) ) ;
#23493 = CARTESIAN_POINT ( 'NONE',  ( 65.00000000000000000, 36.13828125216787157, -13.57481594606304576 ) ) ;
#23494 = CARTESIAN_POINT ( 'NONE',  ( 108.0825317499999869, 107.3738262389971538, -50.72499999726881015 ) ) ;
#23495 = CARTESIAN_POINT ( 'NONE',  ( -5.622872871577873077, 35.39414062716787157, -13.57481594606304753 ) ) ;
#23496 = AXIS2_PLACEMENT_3D ( 'NONE', #4702, #27977, #10427 ) ;
#23497 = ORIENTED_EDGE ( 'NONE', *, *, #25184, .F. ) ;
#23498 = CARTESIAN_POINT ( 'NONE',  ( 96.46446609406721961, 3.535533905932755072, 6.874999999999999112 ) ) ;
#23499 = ORIENTED_EDGE ( 'NONE', *, *, #13831, .T. ) ;
#23500 = CARTESIAN_POINT ( 'NONE',  ( 195.0000000000000000, 36.78320312608393294, 13.14518615778179544 ) ) ;
#23501 = DIRECTION ( 'NONE',  ( 0.000000000000000000, 0.000000000000000000, -1.000000000000000000 ) ) ;
#23502 = CARTESIAN_POINT ( 'NONE',  ( 143.1451861577818079, 37.77539062608393294, -1.609821015232357215E-15 ) ) ;
#23503 = CARTESIAN_POINT ( 'NONE',  ( 0.000000000000000000, -7.395377635281828788, 0.000000000000000000 ) ) ;
#23504 =( BOUNDED_CURVE ( )  B_SPLINE_CURVE ( 2, ( #6123, #23652, #18947, #18814, #4127, #12507, #20824, #19229, #27521 ),
 .UNSPECIFIED., .F., .F. ) 
 B_SPLINE_CURVE_WITH_KNOTS ( ( 3, 2, 2, 2, 3 ),
 ( 0.5208333333333332593, 0.5312500000000000000, 0.5416666666666667407, 0.5520833333333337034, 0.5625000000000004441 ),
 .UNSPECIFIED. ) 
 CURVE ( )  GEOMETRIC_REPRESENTATION_ITEM ( )  RATIONAL_B_SPLINE_CURVE ( ( 1.000000000000000888, 0.9238795325112859613, 1.000000000000000000, 0.9238795325112867385, 1.000000000000000000, 0.9238795325112867385, 1.000000000000000000, 0.9238795325112835188, 1.000000000000003331 ) ) 
 REPRESENTATION_ITEM ( '' )  );
#23505 = DIRECTION ( 'NONE',  ( -0.000000000000000000, -1.000000000000000000, -0.000000000000000000 ) ) ;
#23506 = CARTESIAN_POINT ( 'NONE',  ( 99.99999999999998579, 94.56249999863440792, -4.458734124999994997 ) ) ;
#23507 = CARTESIAN_POINT ( 'NONE',  ( 107.0000000000000142, 110.0000000000000000, -55.00000000000000711 ) ) ;
#23508 = AXIS2_PLACEMENT_3D ( 'NONE', #11710, #3184, #1335 ) ;
#23509 = CARTESIAN_POINT ( 'NONE',  ( -13.14518615778179900, 40.50390625108394005, -5.444914386472297529 ) ) ;
#23510 = CARTESIAN_POINT ( 'NONE',  ( 185.4011555911795597, 36.33671874999999574, 9.598844408820459861 ) ) ;
#23511 = APPLICATION_PROTOCOL_DEFINITION ( 'draft international standard', 'automotive_design', 1998, #24064 ) ;
#23512 = CYLINDRICAL_SURFACE ( 'NONE', #25981, 5.000000000000004441 ) ;
#23513 = CARTESIAN_POINT ( 'NONE',  ( 98.15313185440925281, -4.458734124999987891, 3.875000001365592084 ) ) ;
#23514 = CARTESIAN_POINT ( 'NONE',  ( 78.14518615778179367, 39.31328125108392868, 5.444914386472293977 ) ) ;
#23515 = CARTESIAN_POINT ( 'NONE',  ( 95.54126587499996504, 1.387778780781445676E-14, 5.437500001365591196 ) ) ;
#23516 = DIRECTION ( 'NONE',  ( 1.000000000000000000, 0.000000000000000000, 0.000000000000000000 ) ) ;
#23517 = CARTESIAN_POINT ( 'NONE',  ( 104.4587341249999781, 91.31249999863440792, -6.938893903907228378E-15 ) ) ;
#23518 = VECTOR ( 'NONE', #10890, 1000.000000000000000 ) ;
#23519 = DIRECTION ( 'NONE',  ( 0.000000000000000000, 1.000000000000000000, 0.000000000000000000 ) ) ;
#23520 = CARTESIAN_POINT ( 'NONE',  ( -9.598844408820454532, 38.71796874999999716, 9.598844408820459861 ) ) ;
#23521 = CARTESIAN_POINT ( 'NONE',  ( 143.1451861577818079, 39.51171875108392584, 5.444914386472293977 ) ) ;
#23522 = ORIENTED_EDGE ( 'NONE', *, *, #10708, .F. ) ;
#23523 = CARTESIAN_POINT ( 'NONE',  ( 104.4587341249999639, 83.18750000136560629, -1.442382525525748735E-14 ) ) ;
#23524 = CARTESIAN_POINT ( 'NONE',  ( -5.622872871577965448, 31.72304687716787086, 13.57481594606295161 ) ) ;
#23525 = ORIENTED_EDGE ( 'NONE', *, *, #25892, .F. ) ;
#23526 = CARTESIAN_POINT ( 'NONE',  ( 107.0000000000000000, 110.0000000000000000, -46.00000000000001421 ) ) ;
#23527 = CARTESIAN_POINT ( 'NONE',  ( 65.00000000000000000, 36.18789062608393436, 13.14518615778179544 ) ) ;
#23528 = VERTEX_POINT ( 'NONE', #28024 ) ;
#23529 = AXIS2_PLACEMENT_3D ( 'NONE', #1348, #23145, #3620 ) ;
#23530 = DIRECTION ( 'NONE',  ( -0.000000000000000000, -0.000000000000000000, -1.000000000000000000 ) ) ;
#23531 = CARTESIAN_POINT ( 'NONE',  ( 95.54126587499996504, 1.387778780781445676E-14, 1.687500001365591418 ) ) ;
#23532 = EDGE_CURVE ( 'NONE', #5414, #5755, #5657, .T. ) ;
#23533 = ORIENTED_EDGE ( 'NONE', *, *, #14737, .T. ) ;
#23534 = CARTESIAN_POINT ( 'NONE',  ( -8.049105076161786076E-16, 34.20351562608394147, -13.14518615778179544 ) ) ;
#23535 = CARTESIAN_POINT ( 'NONE',  ( 9.295050272127047819, 34.50117187608393010, 9.295050272127046043 ) ) ;
#23536 = CARTESIAN_POINT ( 'NONE',  ( 189.3771271284221314, 36.48554687716787015, 13.57481594606304753 ) ) ;
#23537 = CARTESIAN_POINT ( 'NONE',  ( -13.14518615778179722, 38.91640625108393436, -5.444914386472297529 ) ) ;
#23538 = LINE ( 'NONE', #19256, #13471 ) ;
#23539 = CARTESIAN_POINT ( 'NONE',  ( 204.1801758136480203, 50.00000000000000711, 14.99999999999995559 ) ) ;
#23540 = CARTESIAN_POINT ( 'NONE',  ( 120.7049497278729575, 40.65273437608393436, -9.295050272127046043 ) ) ;
#23541 = CARTESIAN_POINT ( 'NONE',  ( -13.14518615778179544, 38.37070312608393152, 0.000000000000000000 ) ) ;
#23542 = ORIENTED_EDGE ( 'NONE', *, *, #26955, .T. ) ;
#23543 = CARTESIAN_POINT ( 'NONE',  ( 78.57481594606305464, 37.42812499999999432, -1.662435489736055892E-15 ) ) ;
#23544 = CARTESIAN_POINT ( 'NONE',  ( 2.493653234604083739E-15, 38.12265625216787157, 13.57481594606304576 ) ) ;
#23545 = CARTESIAN_POINT ( 'NONE',  ( 98.15313185440925281, 4.458734125000016313, 13.50000000136559208 ) ) ;
#23546 = CYLINDRICAL_SURFACE ( 'NONE', #16711, 7.000000000000006217 ) ;
#23547 = CARTESIAN_POINT ( 'NONE',  ( 95.54126587499995082, 1.846868145590750077, 3.375000001365592972 ) ) ;
#23548 = CARTESIAN_POINT ( 'NONE',  ( 91.91746824999999887, 110.0000000000000000, -53.12500000273119838 ) ) ;
#23549 = CARTESIAN_POINT ( 'NONE',  ( 96.84719886470459471, 3.152801135295383084, 4.562500001365592084 ) ) ;
#23550 = CIRCLE ( 'NONE', #18555, 5.000000000000004441 ) ;
#23551 = CARTESIAN_POINT ( 'NONE',  ( 104.4587341249999781, 81.12500000136560629, 1.846868145590721655 ) ) ;
#23552 = CARTESIAN_POINT ( 'NONE',  ( 13.14518615778179544, 32.21914062608393436, -1.609821015232357215E-15 ) ) ;
#23553 = CARTESIAN_POINT ( 'NONE',  ( 13.14518615778179900, 40.30546875108393579, 5.444914386472293977 ) ) ;
#23554 = CARTESIAN_POINT ( 'NONE',  ( 95.00472066334982912, 103.1245878333314323, -49.57499999726881157 ) ) ;
#23555 = ORIENTED_EDGE ( 'NONE', *, *, #18000, .T. ) ;
#23556 = CARTESIAN_POINT ( 'NONE',  ( 204.1801758136479918, 55.00000000000000000, -10.00000000000000000 ) ) ;
#23557 = CARTESIAN_POINT ( 'NONE',  ( 99.14382582708708469, 124.4000000010924794, -2.066987299999998751 ) ) ;
#23558 = CARTESIAN_POINT ( 'NONE',  ( 97.92893218813451028, 5.000000000000018652, 5.812500000000000000 ) ) ;
#23559 = CARTESIAN_POINT ( 'NONE',  ( 102.0710678118654329, 81.81250000273119838, -5.000000000000018652 ) ) ;
#23560 = CARTESIAN_POINT ( 'NONE',  ( 2.493653234604083739E-15, 40.40468749999999432, 13.57481594606304576 ) ) ;
#23561 = CARTESIAN_POINT ( 'NONE',  ( 200.4449143864723055, 39.21406250108392300, 13.14518615778179189 ) ) ;
#23562 = EDGE_LOOP ( 'NONE', ( #12022, #27234, #21246, #19213 ) ) ;
#23563 = CARTESIAN_POINT ( 'NONE',  ( 65.00000000000000000, 37.37851562608393863, -13.14518615778179544 ) ) ;
#23564 = PLANE ( 'NONE',  #17341 ) ;
#23565 = CARTESIAN_POINT ( 'NONE',  ( -8.312177448680279460E-16, 39.21406249999999716, -13.57481594606304576 ) ) ;
#23566 = ORIENTED_EDGE ( 'NONE', *, *, #3941, .T. ) ;
#23567 = CARTESIAN_POINT ( 'NONE',  ( 95.67376207875072680, 104.0454443415356991, -51.70000000000001705 ) ) ;
#23568 = CARTESIAN_POINT ( 'NONE',  ( 99.99999999999998579, 136.0000000000000000, -5.204170427930421283E-15 ) ) ;
#23569 = CARTESIAN_POINT ( 'NONE',  ( 101.4615807364564546, 123.6500000010924651, -1.461580736456474794 ) ) ;
#23570 = CARTESIAN_POINT ( 'NONE',  ( 139.5988444088204403, 34.45156250216787441, -9.598844408820458085 ) ) ;
#23571 = CARTESIAN_POINT ( 'NONE',  ( 104.9999999999999716, 81.56250000273119838, 2.071067811865462627 ) ) ;
#23572 = CARTESIAN_POINT ( 'NONE',  ( -9.598844408820454532, 34.84843750216787583, 9.598844408820459861 ) ) ;
#23573 = CARTESIAN_POINT ( 'NONE',  ( 185.7049497278729575, 33.70742187608393436, 9.295050272127047819 ) ) ;
#23574 = VERTEX_POINT ( 'NONE', #6908 ) ;
#23575 = ORIENTED_EDGE ( 'NONE', *, *, #10051, .T. ) ;
#23576 = ORIENTED_EDGE ( 'NONE', *, *, #6126, .T. ) ;
#23577 = CARTESIAN_POINT ( 'NONE',  ( 5.444914386472302859, 34.45156250108393436, 13.14518615778179189 ) ) ;
#23578 = LINE ( 'NONE', #6058, #2141 ) ;
#23579 = CARTESIAN_POINT ( 'NONE',  ( 99.99999999999995737, 82.68750000136560629, 4.458734124999988779 ) ) ;
#23580 = CARTESIAN_POINT ( 'NONE',  ( 78.57481594606305464, 39.90859375216787441, -1.662435489736055892E-15 ) ) ;
#23581 = CARTESIAN_POINT ( 'NONE',  ( -20.00000000000000000, 55.00000000000000000, 10.00000000000000178 ) ) ;
#23582 = DIRECTION ( 'NONE',  ( -0.000000000000000000, -1.000000000000000000, -0.000000000000000000 ) ) ;
#23583 = CARTESIAN_POINT ( 'NONE',  ( 185.7049497278729575, 40.05742187608393579, 9.295050272127047819 ) ) ;
#23584 = CARTESIAN_POINT ( 'NONE',  ( 97.50236033167490746, 102.3130555110000159, -47.22499999726881725 ) ) ;
#23585 = CIRCLE ( 'NONE', #13094, 13.57481594606304576 ) ;
#23586 = ORIENTED_EDGE ( 'NONE', *, *, #27480, .F. ) ;
#23587 = EDGE_CURVE ( 'NONE', #21530, #10042, #25212, .T. ) ;
#23588 = CARTESIAN_POINT ( 'NONE',  ( -8.312177448680279460E-16, 40.00781250000000000, -13.57481594606304576 ) ) ;
#23589 = CARTESIAN_POINT ( 'NONE',  ( 13.14518615778179544, 40.15664062608393436, -1.609821015232357215E-15 ) ) ;
#23590 = CARTESIAN_POINT ( 'NONE',  ( 104.9999999999999716, 1.449011120738813565E-14, 2.625000002731185500 ) ) ;
#23591 = CARTESIAN_POINT ( 'NONE',  ( 124.5550856135277087, 36.93203125108394147, 13.14518615778179722 ) ) ;
#23592 = CARTESIAN_POINT ( 'NONE',  ( 65.00000000000000000, 36.38632812608393152, -13.14518615778179544 ) ) ;
#23593 = CARTESIAN_POINT ( 'NONE',  ( 208.1451861577817795, 40.40468750108393436, -5.444914386472297529 ) ) ;
#23594 = DIRECTION ( 'NONE',  ( -0.000000000000000000, -0.000000000000000000, -1.000000000000000000 ) ) ;
#23595 = CARTESIAN_POINT ( 'NONE',  ( 9.295050272127046043, 36.28710937608393294, -9.295050272127046043 ) ) ;
#23596 = CARTESIAN_POINT ( 'NONE',  ( 129.5539587432196811, 49.99999999978092546, -13.57776691409254433 ) ) ;
#23597 = EDGE_CURVE ( 'NONE', #24544, #2199, #16386, .T. ) ;
#23598 = DIRECTION ( 'NONE',  ( -5.782411586589357392E-17, 0.000000000000000000, -1.000000000000000000 ) ) ;
#23599 = CARTESIAN_POINT ( 'NONE',  ( 97.92893218813455292, 81.81250000000001421, -5.000000000000053291 ) ) ;
#23600 = EDGE_CURVE ( 'NONE', #11913, #291, #11454, .T. ) ;
#23601 = CARTESIAN_POINT ( 'NONE',  ( 13.14518615778179900, 40.10703125108393152, 5.444914386472293977 ) ) ;
#23602 = DIRECTION ( 'NONE',  ( 0.000000000000000000, -1.000000000000000000, 0.000000000000000000 ) ) ;
#23603 = CARTESIAN_POINT ( 'NONE',  ( 102.4999999999999858, 123.9000000021849530, -9.847140817659276890E-15 ) ) ;
#23604 = EDGE_CURVE ( 'NONE', #17147, #24017, #15596, .T. ) ;
#23605 = VECTOR ( 'NONE', #2992, 1000.000000000000000 ) ;
#23606 = CARTESIAN_POINT ( 'NONE',  ( 58.88224005446349452, 54.65941425414899868, 14.99999999999998401 ) ) ;
#23607 = CARTESIAN_POINT ( 'NONE',  ( 97.93301270000000613, 123.1500000010924651, -9.540979117872439019E-15 ) ) ;
#23608 = DIRECTION ( 'NONE',  ( 1.000000000000000000, 0.000000000000000000, 0.000000000000000000 ) ) ;
#23609 = CIRCLE ( 'NONE', #17233, 13.57481594606304398 ) ;
#23610 = CARTESIAN_POINT ( 'NONE',  ( 95.54126587499995082, 1.846868145590750077, 9.375000001365592084 ) ) ;
#23611 = CARTESIAN_POINT ( 'NONE',  ( 94.33688103937537051, 105.8855032339526758, -48.30000000546237970 ) ) ;
#23612 = VERTEX_POINT ( 'NONE', #2506 ) ;
#23613 = CARTESIAN_POINT ( 'NONE',  ( 94.33688103937537051, 105.8855032339526758, -53.80000000000000426 ) ) ;
#23614 = CARTESIAN_POINT ( 'NONE',  ( 95.54126587499996504, 1.387778780781445676E-14, 12.43750000136559208 ) ) ;
#23615 = CARTESIAN_POINT ( 'NONE',  ( -5.444914386472299306, 32.76484375108393010, 13.14518615778179722 ) ) ;
#23616 = ADVANCED_FACE ( 'NONE', ( #24167 ), #513, .T. ) ;
#23617 = CARTESIAN_POINT ( 'NONE',  ( 9.295050272127046043, 40.25585937608393294, -9.295050272127046043 ) ) ;
#23618 = CARTESIAN_POINT ( 'NONE',  ( 130.0000000000000000, 36.53515625216787299, 13.57481594606304576 ) ) ;
#23619 = CARTESIAN_POINT ( 'NONE',  ( 96.84719886470459471, 83.81250000136560629, 3.152801135295355994 ) ) ;
#23620 = CARTESIAN_POINT ( 'NONE',  ( 74.29505027212704249, 37.87460937608393863, 9.295050272127046043 ) ) ;
#23621 = CARTESIAN_POINT ( 'NONE',  ( 102.4976396683250925, 102.3130555110000159, -50.77500000273119696 ) ) ;
#23622 = DIRECTION ( 'NONE',  ( 1.000000000000000000, 0.000000000000000000, 0.000000000000000000 ) ) ;
#23623 =( BOUNDED_CURVE ( )  B_SPLINE_CURVE ( 2, ( #17837, #4736, #319, #19985, #6856, #13107, #463, #24114, #35, #6442, #178, #21702, #10979, #8578, #2322, #4882, #17268, #10840, #9144, #2035, #25969, #19691, #8860, #23832, #28114, #26542, #17699, #19554, #6998, #15257, #4591, #13546, #24394, #15546, #24254, #12970, #17551 ),
 .UNSPECIFIED., .F., .F. ) 
 B_SPLINE_CURVE_WITH_KNOTS ( ( 3, 2, 2, 2, 2, 2, 2, 2, 2, 2, 2, 2, 2, 2, 2, 2, 2, 2, 3 ),
 ( 0.000000000000000000, 0.04166666666666666435, 0.08333333333333332871, 0.1250000000000000000, 0.1666666666666666574, 0.2083333333333333148, 0.2500000000000000000, 0.2916666666666666852, 0.3333333333333333148, 0.3750000000000000000, 0.4166666666666666297, 0.4583333333333333148, 0.5000000000000000000, 0.5416666666666666297, 0.5833333333333333703, 0.6250000000000000000, 0.6666666666666666297, 0.7083333333333334814, 0.7291666671045423653 ),
 .UNSPECIFIED. ) 
 CURVE ( )  GEOMETRIC_REPRESENTATION_ITEM ( )  RATIONAL_B_SPLINE_CURVE ( ( 1.000000000000000000, 0.9238795325112867385, 1.000000000000000000, 0.9238795325112867385, 1.000000000000000000, 0.9238795325112867385, 1.000000000000000000, 0.9238795325112867385, 1.000000000000000000, 0.9238795325112867385, 1.000000000000000000, 0.9238795325112867385, 1.000000000000000000, 0.9238795325112867385, 1.000000000000000000, 0.9238795325112867385, 1.000000000000000000, 0.9238795325112867385, 1.000000000000000000, 0.9238795325112867385, 1.000000000000000000, 0.9238795325112867385, 1.000000000000000000, 0.9238795325112867385, 1.000000000000000000, 0.9238795325112867385, 1.000000000000000000, 0.9238795325112867385, 1.000000000000000000, 0.9238795325112867385, 1.000000000000000000, 0.9238795325112867385, 1.000000000000000000, 0.9238795325112867385, 1.000000000000000000, 0.9619397654556921529, 0.9619397662556433692 ) ) 
 REPRESENTATION_ITEM ( '' )  );
#23624 = DIRECTION ( 'NONE',  ( 0.8660254037844404840, 0.000000000000000000, 0.4999999999999967804 ) ) ;
#23625 = DIRECTION ( 'NONE',  ( 7.228014483236696740E-18, -0.000000000000000000, 1.000000000000000000 ) ) ;
#23626 = CARTESIAN_POINT ( 'NONE',  ( 99.99999999999997158, 102.6397644303321215, -49.99999999453764588 ) ) ;
#23627 = CARTESIAN_POINT ( 'NONE',  ( 116.8548138422182063, 32.76484375108393010, -5.444914386472297529 ) ) ;
#23628 = ORIENTED_EDGE ( 'NONE', *, *, #8973, .F. ) ;
#23629 = DIRECTION ( 'NONE',  ( -0.000000000000000000, 1.000000000000000000, -0.000000000000000000 ) ) ;
#23630 = CARTESIAN_POINT ( 'NONE',  ( -13.14518615778179544, 40.75195312608393294, 0.000000000000000000 ) ) ;
#23631 = CARTESIAN_POINT ( 'NONE',  ( 96.84719886470459471, 79.56250000136559208, 3.152801135295355994 ) ) ;
#23632 = CARTESIAN_POINT ( 'NONE',  ( 143.1451861577818079, 35.34453125108392868, 5.444914386472293977 ) ) ;
#23633 = CARTESIAN_POINT ( 'NONE',  ( 70.62287287157788285, 38.17226562716786731, 13.57481594606304576 ) ) ;
#23634 = EDGE_CURVE ( 'NONE', #9074, #23612, #2744, .T. ) ;
#23635 = CARTESIAN_POINT ( 'NONE',  ( 91.91746824999998466, 110.0000000000000000, -51.62499999726882294 ) ) ;
#23636 = CARTESIAN_POINT ( 'NONE',  ( 2.493653234604083739E-15, 35.74140625216787015, 13.57481594606304576 ) ) ;
#23637 = VECTOR ( 'NONE', #27975, 1000.000000000000000 ) ;
#23638 = CARTESIAN_POINT ( 'NONE',  ( 94.99999999999995737, 1.387778780781445676E-14, 4.000000000000000000 ) ) ;
#23639 = ORIENTED_EDGE ( 'NONE', *, *, #20977, .F. ) ;
#23640 = EDGE_CURVE ( 'NONE', #4741, #14316, #22030, .T. ) ;
#23641 = CARTESIAN_POINT ( 'NONE',  ( 189.5550856135277229, 37.22968750108393721, -13.14518615778179900 ) ) ;
#23642 = CARTESIAN_POINT ( 'NONE',  ( -5.622872871577839327, 38.76757812499998579, 13.57481594606308128 ) ) ;
#23643 = ADVANCED_FACE ( 'NONE', ( #13445 ), #224, .T. ) ;
#23644 = CARTESIAN_POINT ( 'NONE',  ( 120.7049497278729575, 39.66054687608393436, -9.295050272127046043 ) ) ;
#23645 = CARTESIAN_POINT ( 'NONE',  ( 99.99999999999998579, 122.5000000021849615, -2.499999999999997780 ) ) ;
#23646 = CARTESIAN_POINT ( 'NONE',  ( 99.99999999999995737, 5.000000000000018652, 4.875000002731185944 ) ) ;
#23647 = CARTESIAN_POINT ( 'NONE',  ( 130.0000000000000000, 50.00000000000000000, -1.503427012513233026E-14 ) ) ;
#23648 = CARTESIAN_POINT ( 'NONE',  ( 107.0000000000000142, 107.7255621263696668, -48.10000000000001563 ) ) ;
#23649 = CARTESIAN_POINT ( 'NONE',  ( 9.295050272127046043, 38.86679687608393863, -9.295050272127046043 ) ) ;
#23650 = CARTESIAN_POINT ( 'NONE',  ( 9.295050272127046043, 38.66835937608393436, -9.295050272127046043 ) ) ;
#23651 = CARTESIAN_POINT ( 'NONE',  ( 200.6228728715778686, 36.48554687499999716, 13.57481594606304576 ) ) ;
#23652 = CARTESIAN_POINT ( 'NONE',  ( 5.622872871577825116, 35.98945312500000426, -13.57481594606309372 ) ) ;
#23653 = CARTESIAN_POINT ( 'NONE',  ( 99.99999999999995737, -4.458734124999988779, 4.937500001365592972 ) ) ;
#23654 = CARTESIAN_POINT ( 'NONE',  ( 74.29505027212704249, 37.67617187608393436, 9.295050272127046043 ) ) ;
#23655 = CARTESIAN_POINT ( 'NONE',  ( 96.84719886470459471, 3.152801135295383084, 7.312500001365592084 ) ) ;
#23656 = CARTESIAN_POINT ( 'NONE',  ( 99.99999999999998579, 110.0000000000000000, -145.0000000000000284 ) ) ;
#23657 = CARTESIAN_POINT ( 'NONE',  ( 103.1528011352953484, 92.43749999863440792, -3.152801135295366208 ) ) ;
#23658 = AXIS2_PLACEMENT_3D ( 'NONE', #9567, #18553, #24963 ) ;
#23659 = CARTESIAN_POINT ( 'NONE',  ( -6.338290792349636327, 36.00000000000000000, 11.53992004315014164 ) ) ;
#23660 = CARTESIAN_POINT ( 'NONE',  ( -5.622872871577873077, 37.97382812499999716, 13.57481594606304753 ) ) ;
#23661 = LINE ( 'NONE', #2140, #7136 ) ;
#23662 = ORIENTED_EDGE ( 'NONE', *, *, #19418, .F. ) ;
#23663 = CARTESIAN_POINT ( 'NONE',  ( 95.54126587499996504, 79.68750000136559208, -1.387778780781445676E-14 ) ) ;
#23664 = CARTESIAN_POINT ( 'NONE',  ( 98.15313185440925281, 90.62499999863439371, -4.458734124999994997 ) ) ;
#23665 = VERTEX_POINT ( 'NONE', #13593 ) ;
#23666 = VECTOR ( 'NONE', #7125, 1000.000000000000114 ) ;
#23667 = FACE_OUTER_BOUND ( 'NONE', #25279, .T. ) ;
#23668 = CARTESIAN_POINT ( 'NONE',  ( 59.55508561352770158, 33.75703125108393721, 13.14518615778179722 ) ) ;
#23669 = ORIENTED_EDGE ( 'NONE', *, *, #15132, .F. ) ;
#23670 = CARTESIAN_POINT ( 'NONE',  ( 84.99999999999998579, 100.0000000000000000, -15.00000000000000533 ) ) ;
#23671 = CARTESIAN_POINT ( 'NONE',  ( 103.1528011352953342, 3.152801135295383084, 4.312500001365592084 ) ) ;
#23672 = ORIENTED_EDGE ( 'NONE', *, *, #4590, .T. ) ;
#23673 = CARTESIAN_POINT ( 'NONE',  ( -13.14518615778179544, 35.98945312608393721, 0.000000000000000000 ) ) ;
#23674 =( BOUNDED_CURVE ( )  B_SPLINE_CURVE ( 2, ( #4053, #8455, #23572, #13129, #10996, #8597, #6457, #4187, #8312 ),
 .UNSPECIFIED., .F., .F. ) 
 B_SPLINE_CURVE_WITH_KNOTS ( ( 3, 2, 2, 2, 3 ),
 ( 0.5624999999999996669, 0.5729166666666664076, 0.5833333333333332593, 0.5937500000000001110, 0.6041666666666668517 ),
 .UNSPECIFIED. ) 
 CURVE ( )  GEOMETRIC_REPRESENTATION_ITEM ( )  RATIONAL_B_SPLINE_CURVE ( ( 1.000000000000002442, 0.9238795325112842960, 1.000000000000000000, 0.9238795325112867385, 1.000000000000000000, 0.9238795325112867385, 1.000000000000000000, 0.9238795325112850731, 1.000000000000001554 ) ) 
 REPRESENTATION_ITEM ( '' )  );
#23675 = CARTESIAN_POINT ( 'NONE',  ( 13.14518615778179544, 37.97382812608393721, -1.609821015232357215E-15 ) ) ;
#23676 = CARTESIAN_POINT ( 'NONE',  ( 195.0000000000000000, 37.32890625216786873, 13.57481594606304576 ) ) ;
#23677 = CARTESIAN_POINT ( 'NONE',  ( 13.14518615778179722, 36.23750000108393010, -5.444914386472297529 ) ) ;
#23678 = DIRECTION ( 'NONE',  ( 1.000000000000000000, 0.000000000000000000, -2.385244779468110248E-16 ) ) ;
#23679 = CARTESIAN_POINT ( 'NONE',  ( 195.0000000000000000, -7.395377635281828788, -13.57481594606306707 ) ) ;
#23680 = CARTESIAN_POINT ( 'NONE',  ( 135.4449143864723339, 39.41250000108393436, 13.14518615778179189 ) ) ;
#23682 = AXIS2_PLACEMENT_3D ( 'NONE', #17048, #13032, #16782 ) ;
#23681 = CARTESIAN_POINT ( 'NONE',  ( 5.444914386472302859, 37.03125000108393294, 13.14518615778179189 ) ) ;
#23683 = CARTESIAN_POINT ( 'NONE',  ( 124.5550856135277087, 33.55859375108393294, 13.14518615778179722 ) ) ;
#23684 = CARTESIAN_POINT ( 'NONE',  ( 59.37712712842213136, 36.88242187499999858, -13.57481594606304753 ) ) ;
#23685 = CARTESIAN_POINT ( 'NONE',  ( 96.46446609406721961, 3.535533905932755072, 9.874999999999998224 ) ) ;
#23686 = CARTESIAN_POINT ( 'NONE',  ( 96.84719886470459471, 3.152801135295383084, 2.312500001365592084 ) ) ;
#23687 = FACE_OUTER_BOUND ( 'NONE', #15081, .T. ) ;
#23688 = CARTESIAN_POINT ( 'NONE',  ( 95.54126587499996504, 1.387778780781445676E-14, 4.437500001365592084 ) ) ;
#23689 = CARTESIAN_POINT ( 'NONE',  ( 99.99999999999995737, 5.000000000000018652, 3.875000002731185056 ) ) ;
#23690 = DIRECTION ( 'NONE',  ( 5.782411586589357392E-17, -0.000000000000000000, 1.000000000000000000 ) ) ;
#23691 = DIRECTION ( 'NONE',  ( 0.000000000000000000, 0.000000000000000000, -1.000000000000000000 ) ) ;
#23692 = CARTESIAN_POINT ( 'NONE',  ( -5.444914386472297529, 32.46718750108393436, -13.14518615778179900 ) ) ;
#23693 = CARTESIAN_POINT ( 'NONE',  ( 2.414731522848535132E-15, 39.36289062608393152, 13.14518615778179544 ) ) ;
#23694 = CARTESIAN_POINT ( 'NONE',  ( 108.0825317499999869, 112.6261737610028320, -50.77499999726882152 ) ) ;
#23695 = ORIENTED_EDGE ( 'NONE', *, *, #20668, .F. ) ;
#23696 = CARTESIAN_POINT ( 'NONE',  ( -13.14518615778179189, 32.07031250108393294, 5.444914386472304635 ) ) ;
#23697 = CARTESIAN_POINT ( 'NONE',  ( 95.67376207875072680, 104.0454443415356991, -54.19999999453764872 ) ) ;
#23698 = CARTESIAN_POINT ( 'NONE',  ( 107.0000000000000142, 110.0000000000000000, -54.25000000273119838 ) ) ;
#23699 = CARTESIAN_POINT ( 'NONE',  ( 181.4251840539369596, 36.28710937499999289, 5.622872871577880183 ) ) ;
#23700 = CARTESIAN_POINT ( 'NONE',  ( 204.2950502721270425, 39.26367187608393294, 9.295050272127046043 ) ) ;
#23701 = ORIENTED_EDGE ( 'NONE', *, *, #26598, .T. ) ;
#23702 = CARTESIAN_POINT ( 'NONE',  ( 0.000000000000000000, 36.00000000000000000, 0.000000000000000000 ) ) ;
#23703 = CARTESIAN_POINT ( 'NONE',  ( 214.9999999999999716, 55.00000000000000000, 9.999999999999946709 ) ) ;
#23704 = CARTESIAN_POINT ( 'NONE',  ( 68.11659208046573610, 53.90895096933308395, -14.99999999999999822 ) ) ;
#23705 = ORIENTED_EDGE ( 'NONE', *, *, #8241, .T. ) ;
#23706 = CARTESIAN_POINT ( 'NONE',  ( 94.33688103937537051, 105.8855032339526758, -47.80000000000001137 ) ) ;
#23707 = CARTESIAN_POINT ( 'NONE',  ( -13.14518615778179544, 38.96601562608393721, 0.000000000000000000 ) ) ;
#23708 = FACE_OUTER_BOUND ( 'NONE', #27224, .T. ) ;
#23709 = CARTESIAN_POINT ( 'NONE',  ( 120.4011555911795455, 35.44375000216787441, -9.598844408820458085 ) ) ;
#23710 =( BOUNDED_CURVE ( )  B_SPLINE_CURVE ( 2, ( #5395, #14064, #22784, #20643, #3254, #9795, #7661, #16354, #5539, #14202, #10897 ),
 .UNSPECIFIED., .F., .F. ) 
 B_SPLINE_CURVE_WITH_KNOTS ( ( 3, 2, 2, 2, 2, 3 ),
 ( 0.6999999999999998446, 0.7199999999999998623, 0.7399999999999998801, 0.7600000000000000089, 0.7800000000000000266, 0.8000000000000000444 ),
 .UNSPECIFIED. ) 
 CURVE ( )  GEOMETRIC_REPRESENTATION_ITEM ( )  RATIONAL_B_SPLINE_CURVE ( ( 1.000000000000000222, 0.9510565162951533091, 1.000000000000000000, 0.9510565162951535312, 1.000000000000000000, 0.9510565162951535312, 1.000000000000000000, 0.9510565162951535312, 1.000000000000000000, 0.9510565162951535312, 1.000000000000000000 ) ) 
 REPRESENTATION_ITEM ( '' )  );
#23711 = CARTESIAN_POINT ( 'NONE',  ( 107.0000000000000142, 107.7255621263696526, -43.60000000546237686 ) ) ;
#23712 = CARTESIAN_POINT ( 'NONE',  ( 5.622872871577946796, 37.27929687499999289, 13.57481594606297115 ) ) ;
#23713 = AXIS2_PLACEMENT_3D ( 'NONE', #21853, #18997, #1768 ) ;
#23714 = CARTESIAN_POINT ( 'NONE',  ( 208.1451861577817795, 35.64218750108393152, -5.444914386472297529 ) ) ;
#23715 = ORIENTED_EDGE ( 'NONE', *, *, #8047, .T. ) ;
#23716 = ORIENTED_EDGE ( 'NONE', *, *, #19539, .F. ) ;
#23717 = EDGE_LOOP ( 'NONE', ( #25627, #11522, #8968 ) ) ;
#23718 = CARTESIAN_POINT ( 'NONE',  ( -13.14518615778179544, 39.95820312608393010, 0.000000000000000000 ) ) ;
#23719 = SURFACE_STYLE_FILL_AREA ( #8320 ) ;
#23720 = DIRECTION ( 'NONE',  ( 0.000000000000000000, 1.000000000000000000, 0.000000000000000000 ) ) ;
#23721 = CARTESIAN_POINT ( 'NONE',  ( 65.00000000000000000, 40.35507812608393152, -13.14518615778179544 ) ) ;
#23722 = CARTESIAN_POINT ( 'NONE',  ( 96.84719886470459471, 81.56250000136559208, 3.152801135295355994 ) ) ;
#23723 = CARTESIAN_POINT ( 'NONE',  ( 189.5550856135277229, 40.40468750108393436, -13.14518615778179722 ) ) ;
#23724 = CARTESIAN_POINT ( 'NONE',  ( 99.99999999999995737, 83.37500000273119838, 4.999999999999990230 ) ) ;
#23725 = ADVANCED_FACE ( 'NONE', ( #17747 ), #6768, .F. ) ;
#23726 = DIRECTION ( 'NONE',  ( 0.000000000000000000, 0.000000000000000000, 1.000000000000000000 ) ) ;
#23727 = CARTESIAN_POINT ( 'NONE',  ( -9.598844408820458085, 37.72578124999999005, -9.598844408820458085 ) ) ;
#23728 = DIRECTION ( 'NONE',  ( 0.000000000000000000, 0.000000000000000000, -1.000000000000000000 ) ) ;
#23729 = CARTESIAN_POINT ( 'NONE',  ( 108.0825317499999869, 112.6261737610028320, -48.52499999726882152 ) ) ;
#23730 = EDGE_LOOP ( 'NONE', ( #13249, #10958, #22513, #963 ) ) ;
#23731 = CARTESIAN_POINT ( 'NONE',  ( 9.598844408820456309, 36.73359374999999716, -9.598844408820458085 ) ) ;
#23732 = CARTESIAN_POINT ( 'NONE',  ( 13.14518615778179544, 36.18789062608393436, -1.609821015232357215E-15 ) ) ;
#23733 =( REPRESENTATION_RELATIONSHIP ('NONE','NONE', #2411, #9145 ) REPRESENTATION_RELATIONSHIP_WITH_TRANSFORMATION ( #4691 )SHAPE_REPRESENTATION_RELATIONSHIP( ) );
#23734 = CARTESIAN_POINT ( 'NONE',  ( 94.99999999999995737, 2.071067811865491048, 1.062500002731185944 ) ) ;
#23735 = CARTESIAN_POINT ( 'NONE',  ( 139.2950502721270425, 37.08085937608393579, 9.295050272127046043 ) ) ;
#23736 = CARTESIAN_POINT ( 'NONE',  ( 51.85481384221820633, 32.66562500108393863, 5.444914386472304635 ) ) ;
#23737 = CARTESIAN_POINT ( 'NONE',  ( 185.7049497278729575, 36.88242187608393152, 9.295050272127047819 ) ) ;
#23738 = CARTESIAN_POINT ( 'NONE',  ( 94.33688103937537051, 105.8855032339526758, -46.30000000546237970 ) ) ;
#23739 = CARTESIAN_POINT ( 'NONE',  ( 9.295050272127046043, 37.08085937608393579, -9.295050272127046043 ) ) ;
#23740 = CARTESIAN_POINT ( 'NONE',  ( 139.1801758136479918, 50.00000000000000000, -10.00000000000000888 ) ) ;
#23741 = CARTESIAN_POINT ( 'NONE',  ( 194.4067442974505866, 36.00000000000001421, 13.13889047851778180 ) ) ;
#23742 = DIRECTION ( 'NONE',  ( 0.000000000000000000, 0.000000000000000000, -1.000000000000000000 ) ) ;
#23743 = CARTESIAN_POINT ( 'NONE',  ( 9.295050272127047819, 38.46992187608393010, 9.295050272127046043 ) ) ;
#23744 = CARTESIAN_POINT ( 'NONE',  ( 99.99999999999998579, 130.0000000000000000, -5.204170427930421283E-15 ) ) ;
#23745 = DIRECTION ( 'NONE',  ( 0.000000000000000000, 0.000000000000000000, -1.000000000000000000 ) ) ;
#23746 = CARTESIAN_POINT ( 'NONE',  ( 94.99999999999995737, 1.387778780781445676E-14, 9.999999999999998224 ) ) ;
#23747 = CARTESIAN_POINT ( 'NONE',  ( 104.4587341249999781, 1.846868145590750299, 10.00000000136559208 ) ) ;
#23748 = CARTESIAN_POINT ( 'NONE',  ( 73.19315564490973713, 36.00000000000001421, 10.45682415286417921 ) ) ;
#23749 = CARTESIAN_POINT ( 'NONE',  ( 108.0825317500000153, 110.0000000000000000, -44.25000000273119838 ) ) ;
#23750 = CARTESIAN_POINT ( 'NONE',  ( 99.99999999999995737, -4.458734124999988779, 13.68750000136559208 ) ) ;
#23751 = DIRECTION ( 'NONE',  ( -0.000000000000000000, -1.000000000000000000, -0.000000000000000000 ) ) ;
#23752 = CARTESIAN_POINT ( 'NONE',  ( -9.295050272127044266, 38.27148437608393294, 9.295050272127047819 ) ) ;
#23753 = LINE ( 'NONE', #6636, #12637 ) ;
#23754 = CARTESIAN_POINT ( 'NONE',  ( 0.000000000000000000, -7.395377635281828788, 0.000000000000000000 ) ) ;
#23755 = CARTESIAN_POINT ( 'NONE',  ( 51.85481384221819923, 39.90859375108394147, -5.444914386472297529 ) ) ;
#23756 = CARTESIAN_POINT ( 'NONE',  ( 104.9952793366501851, 103.1245878333314323, -50.42500000273119554 ) ) ;
#23757 = CARTESIAN_POINT ( 'NONE',  ( 99.99999999999998579, 124.7999999999999972, -2.499999999999997780 ) ) ;
#23758 = EDGE_CURVE ( 'NONE', #2357, #24537, #7909, .T. ) ;
#23759 = DIRECTION ( 'NONE',  ( 1.000000000000000000, 0.000000000000000000, 0.000000000000000000 ) ) ;
#23760 = LINE ( 'NONE', #23900, #24975 ) ;
#23761 = CARTESIAN_POINT ( 'NONE',  ( 95.67376207875069838, 115.9545556584642867, -48.79999999453764303 ) ) ;
#23762 = CARTESIAN_POINT ( 'NONE',  ( 135.6228728715778686, 39.95820312499999716, -13.57481594606304753 ) ) ;
#23763 = ORIENTED_EDGE ( 'NONE', *, *, #17318, .T. ) ;
#23764 = DIRECTION ( 'NONE',  ( -1.000000000000000000, -0.000000000000000000, 2.385244779468110248E-16 ) ) ;
#23765 = EDGE_CURVE ( 'NONE', #15725, #15812, #2649, .T. ) ;
#23766 = CARTESIAN_POINT ( 'NONE',  ( -5.444914386472299306, 36.93203125108394147, 13.14518615778179722 ) ) ;
#23767 = CARTESIAN_POINT ( 'NONE',  ( -5.622872871577873077, 38.07304687716787583, 13.57481594606304753 ) ) ;
#23768 = CARTESIAN_POINT ( 'NONE',  ( 143.1451861577818079, 35.44375000108393436, -5.444914386472297529 ) ) ;
#23769 = CARTESIAN_POINT ( 'NONE',  ( 70.62287287157788285, 35.79101562716787299, 13.57481594606304576 ) ) ;
#23770 = CARTESIAN_POINT ( 'NONE',  ( 1.137167824541903460, 36.00000000000000000, 13.09590655363594180 ) ) ;
#23771 = CARTESIAN_POINT ( 'NONE',  ( 5.622872871577878406, 36.58476562716787583, 13.57481594606304576 ) ) ;
#23772 = CARTESIAN_POINT ( 'NONE',  ( 103.5355339059327093, -3.535533905932726206, 5.375000000000000000 ) ) ;
#23773 = EDGE_CURVE ( 'NONE', #13309, #13582, #26885, .T. ) ;
#23774 = CARTESIAN_POINT ( 'NONE',  ( 104.3262379212492590, 115.9545556584642867, -47.20000000546237828 ) ) ;
#23775 = CARTESIAN_POINT ( 'NONE',  ( 181.8548138422181921, 38.12265625108393152, -5.444914386472297529 ) ) ;
#23776 = CARTESIAN_POINT ( 'NONE',  ( 104.9999999999999716, 81.43750000000002842, 2.071067811865462627 ) ) ;
#23777 = CARTESIAN_POINT ( 'NONE',  ( 100.0000000000000000, 110.0000000000000000, -45.00000000000000711 ) ) ;
#23778 = CARTESIAN_POINT ( 'NONE',  ( 104.9999999999999716, 2.071067811865491937, 6.562499999999998224 ) ) ;
#23779 = CARTESIAN_POINT ( 'NONE',  ( 128.3947281234234197, 53.60388944777321996, 14.99999999999996803 ) ) ;
#23780 = CARTESIAN_POINT ( 'NONE',  ( 13.57481594606304576, 36.63437499999999858, -1.662435489736055892E-15 ) ) ;
#23781 =( BOUNDED_CURVE ( )  B_SPLINE_CURVE ( 2, ( #24886, #18037, #24457, #14032, #13606, #11888, #20613, #22328, #2799 ),
 .UNSPECIFIED., .F., .F. ) 
 B_SPLINE_CURVE_WITH_KNOTS ( ( 3, 2, 2, 2, 3 ),
 ( 0.2708333333333330928, 0.2812499999999998890, 0.2916666666666666852, 0.3020833333333334259, 0.3125000000000002220 ),
 .UNSPECIFIED. ) 
 CURVE ( )  GEOMETRIC_REPRESENTATION_ITEM ( )  RATIONAL_B_SPLINE_CURVE ( ( 1.000000000000001554, 0.9238795325112850731, 1.000000000000000000, 0.9238795325112867385, 1.000000000000000000, 0.9238795325112867385, 1.000000000000000000, 0.9238795325112850731, 1.000000000000001554 ) ) 
 REPRESENTATION_ITEM ( '' )  );
#23782 = CARTESIAN_POINT ( 'NONE',  ( 130.0000000000000000, -7.395377635281828788, 13.57481594606302799 ) ) ;
#23783 = CARTESIAN_POINT ( 'NONE',  ( 9.295050272127047819, 36.28710937608393294, 9.295050272127046043 ) ) ;
#23784 = CARTESIAN_POINT ( 'NONE',  ( -13.14518615778179544, 38.17226562608393436, 0.000000000000000000 ) ) ;
#23785 = CARTESIAN_POINT ( 'NONE',  ( 204.5988444088204403, 34.35234374999999574, -9.598844408820458085 ) ) ;
#23786 = ADVANCED_FACE ( 'NONE', ( #657 ), #13876, .T. ) ;
#23787 = CARTESIAN_POINT ( 'NONE',  ( 104.9952793366501709, 103.1245878333314465, -44.67500000273118843 ) ) ;
#23788 = DIRECTION ( 'NONE',  ( 0.000000000000000000, 0.000000000000000000, -1.000000000000000000 ) ) ;
#23789 = CARTESIAN_POINT ( 'NONE',  ( 78.14518615778179367, 39.41250000108393436, -5.444914386472297529 ) ) ;
#23790 = CARTESIAN_POINT ( 'NONE',  ( 99.99999999999995737, -4.458734124999988779, 0.6875000013655923059 ) ) ;
#23791 = DIRECTION ( 'NONE',  ( 0.000000000000000000, 0.000000000000000000, 1.000000000000000000 ) ) ;
#23792 = CARTESIAN_POINT ( 'NONE',  ( 99.99999999999998579, 94.56249999863440792, -4.458734124999994997 ) ) ;
#23793 = CARTESIAN_POINT ( 'NONE',  ( -8.312177448680279460E-16, 40.00781250000000000, -13.57481594606304576 ) ) ;
#23794 = CARTESIAN_POINT ( 'NONE',  ( 2.493653234604083739E-15, 34.84843749999999574, 13.57481594606304576 ) ) ;
#23795 = DIRECTION ( 'NONE',  ( 0.000000000000000000, 0.000000000000000000, -1.000000000000000000 ) ) ;
#23796 = ORIENTED_EDGE ( 'NONE', *, *, #26568, .F. ) ;
#23797 = CARTESIAN_POINT ( 'NONE',  ( 98.15313185440925281, 80.87500000136560629, 4.458734124999987891 ) ) ;
#23798 = CARTESIAN_POINT ( 'NONE',  ( 99.99999999999998579, 92.06249999863440792, 4.458734124999981674 ) ) ;
#23799 = VERTEX_POINT ( 'NONE', #26595 ) ;
#23800 = ADVANCED_FACE ( 'NONE', ( #22316 ), #21021, .T. ) ;
#23801 = VECTOR ( 'NONE', #16289, 1000.000000000000000 ) ;
#23802 = CARTESIAN_POINT ( 'NONE',  ( 102.1631189606246153, 116.6573956140660897, -51.60000000000001563 ) ) ;
#23803 = CARTESIAN_POINT ( 'NONE',  ( 78.14518615778179367, 35.59257812608393579, -1.609821015232357215E-15 ) ) ;
#23804 = EDGE_LOOP ( 'NONE', ( #9813, #6412, #22002 ) ) ;
#23805 = CARTESIAN_POINT ( 'NONE',  ( 137.6239419619254534, 54.99999999999999289, -14.99999999999999822 ) ) ;
#23806 = CARTESIAN_POINT ( 'NONE',  ( 104.4587341249999639, 1.442382525525748735E-14, 3.187500001365592972 ) ) ;
#23807 = ORIENTED_EDGE ( 'NONE', *, *, #2897, .T. ) ;
#23808 = CARTESIAN_POINT ( 'NONE',  ( 13.14518615778179722, 34.84843750108393579, -5.444914386472297529 ) ) ;
#23809 = CARTESIAN_POINT ( 'NONE',  ( -13.14518615778179900, 40.70234375108393721, -5.444914386472297529 ) ) ;
#23810 = UNCERTAINTY_MEASURE_WITH_UNIT (LENGTH_MEASURE( 1.000000000000000082E-05 ), #15640, 'distance_accuracy_value', 'NONE');
#23811 = CARTESIAN_POINT ( 'NONE',  ( 208.5748159460630120, 39.16445312716788152, -5.622872871577873077 ) ) ;
#23812 = CARTESIAN_POINT ( 'NONE',  ( -5.444914386472297529, 35.64218750108393152, -13.14518615778179722 ) ) ;
#23813 = CARTESIAN_POINT ( 'NONE',  ( 76.10484805054758795, 36.02027164848242791, -8.092840767093349541 ) ) ;
#23814 = CARTESIAN_POINT ( 'NONE',  ( 99.99999999999995737, 85.00000000000000000, 4.999999999999990230 ) ) ;
#23815 = CARTESIAN_POINT ( 'NONE',  ( 117.3184072029388290, 36.04503594658365984, 5.908507747192915716 ) ) ;
#23816 = ORIENTED_EDGE ( 'NONE', *, *, #3756, .T. ) ;
#23817 = CARTESIAN_POINT ( 'NONE',  ( -9.295050272127044266, 36.88242187608393152, 9.295050272127047819 ) ) ;
#23818 = CARTESIAN_POINT ( 'NONE',  ( 130.0000000000000000, 33.60820312608392868, 13.14518615778179544 ) ) ;
#23819 = CARTESIAN_POINT ( 'NONE',  ( 55.40115559117954547, 33.16171874999999858, 9.598844408820459861 ) ) ;
#23820 = CARTESIAN_POINT ( 'NONE',  ( 99.99999999999998579, 90.00000000000000000, 4.999999999999983125 ) ) ;
#23821 = CIRCLE ( 'NONE', #21547, 10.50000000000001599 ) ;
#23822 = CARTESIAN_POINT ( 'NONE',  ( 95.54126587499996504, 1.387778780781445676E-14, 13.68750000136559386 ) ) ;
#23823 = CARTESIAN_POINT ( 'NONE',  ( 97.83688103937538472, 116.6573956140660897, -46.40000000000001279 ) ) ;
#23824 = CARTESIAN_POINT ( 'NONE',  ( 96.84719886470459471, 3.152801135295383084, 13.31250000136559386 ) ) ;
#23825 = CARTESIAN_POINT ( 'NONE',  ( 102.4976396683250925, 117.6869444889999841, -53.72500000273119980 ) ) ;
#23826 = CARTESIAN_POINT ( 'NONE',  ( 101.7677669529663547, 123.8999999999999915, -1.767766952966370209 ) ) ;
#23827 = DIRECTION ( 'NONE',  ( 1.000000000000000000, 0.000000000000000000, -0.000000000000000000 ) ) ;
#23828 = CARTESIAN_POINT ( 'NONE',  ( -5.444914386472297529, 31.67343750108393863, -13.14518615778179900 ) ) ;
#23829 = CARTESIAN_POINT ( 'NONE',  ( 13.14518615778179900, 38.71796875108393721, 5.444914386472293977 ) ) ;
#23830 = CARTESIAN_POINT ( 'NONE',  ( 97.50236033167490746, 102.3130555110000159, -47.47499999726881725 ) ) ;
#23831 = VERTEX_POINT ( 'NONE', #23158 ) ;
#23832 = CARTESIAN_POINT ( 'NONE',  ( 102.0669873000000081, 123.6000000010924680, -0.8561741729129508371 ) ) ;
#23833 = CARTESIAN_POINT ( 'NONE',  ( 100.8561741729129295, 122.7000000010924765, -2.066987299999998751 ) ) ;
#23834 = CARTESIAN_POINT ( 'NONE',  ( 99.47614712164786965, 123.0000000000000000, 2.223611564848176236 ) ) ;
#23835 = CARTESIAN_POINT ( 'NONE',  ( 130.0000000000000000, -7.395377635281828788, 13.57481594606302799 ) ) ;
#23836 =( BOUNDED_CURVE ( )  B_SPLINE_CURVE ( 2, ( #8861, #15113, #4314, #21704, #4592, #19555, #8719, #15547, #17412 ),
 .UNSPECIFIED., .F., .T. ) 
 B_SPLINE_CURVE_WITH_KNOTS ( ( 3, 2, 2, 2, 3 ),
 ( 0.3125000000000002220, 0.3229166666666668517, 0.3333333333333334259, 0.3437500000000000555, 0.3541666666666666852 ),
 .UNSPECIFIED. ) 
 CURVE ( )  GEOMETRIC_REPRESENTATION_ITEM ( )  RATIONAL_B_SPLINE_CURVE ( ( 0.9999999999999983347, 0.9238795325112884038, 1.000000000000000000, 0.9238795325112867385, 1.000000000000000000, 0.9238795325112867385, 1.000000000000000000, 0.9238795325112867385, 1.000000000000000000 ) ) 
 REPRESENTATION_ITEM ( '' )  );
#23837 = CARTESIAN_POINT ( 'NONE',  ( 189.5550856135277229, 39.90859375108393436, 13.14518615778179722 ) ) ;
#23838 = EDGE_LOOP ( 'NONE', ( #13294, #27094, #5454, #3929 ) ) ;
#23839 = DIRECTION ( 'NONE',  ( 0.000000000000000000, 0.000000000000000000, -1.000000000000000000 ) ) ;
#23840 = DIRECTION ( 'NONE',  ( 1.000000000000000000, 0.000000000000000000, 0.000000000000000000 ) ) ;
#23841 = CARTESIAN_POINT ( 'NONE',  ( 61.20254813104200764, 54.08938259242988522, -15.00000000000000355 ) ) ;
#23842 = CIRCLE ( 'NONE', #7437, 10.50000000000001599 ) ;
#23843 = ORIENTED_EDGE ( 'NONE', *, *, #23286, .T. ) ;
#23844 = CARTESIAN_POINT ( 'NONE',  ( 102.1631189606246295, 116.6573956140660897, -50.60000000000000853 ) ) ;
#23845 = CARTESIAN_POINT ( 'NONE',  ( 5.622872871577786924, 33.40976562716787157, 13.57481594606313813 ) ) ;
#23846 = CARTESIAN_POINT ( 'NONE',  ( 99.14382582708707048, 124.1000000010924964, 2.066987299999979211 ) ) ;
#23847 = CARTESIAN_POINT ( 'NONE',  ( 139.2950502721270425, 39.46210937608393010, -9.295050272127046043 ) ) ;
#23848 = CARTESIAN_POINT ( 'NONE',  ( -13.57481594606304576, 33.85624999999999574, 0.000000000000000000 ) ) ;
#23849 = CARTESIAN_POINT ( 'NONE',  ( 94.99999999999998579, 110.0000000000000000, -45.00000000000000711 ) ) ;
#23850 = DIRECTION ( 'NONE',  ( -0.000000000000000000, -1.000000000000000000, -0.000000000000000000 ) ) ;
#23851 = CARTESIAN_POINT ( 'NONE',  ( 185.7049497278729575, 35.89023437608393152, -9.295050272127046043 ) ) ;
#23852 = ORIENTED_EDGE ( 'NONE', *, *, #10719, .F. ) ;
#23853 = ORIENTED_EDGE ( 'NONE', *, *, #22551, .F. ) ;
#23854 = CARTESIAN_POINT ( 'NONE',  ( 5.444914386472297529, 40.50390625108394005, -13.14518615778179900 ) ) ;
#23855 =( NAMED_UNIT ( * ) SI_UNIT ( $, .STERADIAN. ) SOLID_ANGLE_UNIT ( ) );
#23856 = CARTESIAN_POINT ( 'NONE',  ( 99.99999999999995737, 4.458734125000016313, 11.43750000136559208 ) ) ;
#23857 = CARTESIAN_POINT ( 'NONE',  ( 94.99999999999995737, 80.00000000000000000, -1.387778780781445676E-14 ) ) ;
#23858 = CARTESIAN_POINT ( 'NONE',  ( 95.54126587499996504, 81.37500000136563472, -1.846868145590750077 ) ) ;
#23859 = CARTESIAN_POINT ( 'NONE',  ( 208.1451861577818079, 39.41250000108393436, -5.444914386472297529 ) ) ;
#23860 = CARTESIAN_POINT ( 'NONE',  ( 13.14518615778179722, 37.92421875108393436, 5.444914386472293977 ) ) ;
#23861 = CARTESIAN_POINT ( 'NONE',  ( 130.0000000000000000, 50.00000000000000000, -1.503427012513233026E-14 ) ) ;
#23862 = CARTESIAN_POINT ( 'NONE',  ( -13.57481594606304398, 37.87460937499999147, 5.622872871577880183 ) ) ;
#23863 = CARTESIAN_POINT ( 'NONE',  ( 189.5550856135277229, 40.60312500108393863, -13.14518615778179722 ) ) ;
#23864 = CARTESIAN_POINT ( 'NONE',  ( 104.9952793366501709, 103.1245878333314323, -54.92499999726882720 ) ) ;
#23865 = ORIENTED_EDGE ( 'NONE', *, *, #22029, .F. ) ;
#23866 = AXIS2_PLACEMENT_3D ( 'NONE', #18121, #7282, #18271 ) ;
#23867 = CARTESIAN_POINT ( 'NONE',  ( -9.598844408820454532, 35.54296874999999289, 9.598844408820459861 ) ) ;
#23868 = CARTESIAN_POINT ( 'NONE',  ( -13.14518615778179189, 38.22187500108393010, 5.444914386472304635 ) ) ;
#23869 =( BOUNDED_CURVE ( )  B_SPLINE_CURVE ( 2, ( #1235, #9899, #14588, #21304, #27316, #1786, #10453, #19159, #12306, #27863, #16460, #25154, #18611, #17008, #8323, #16602, #25712, #3501, #18746, #27446, #25294, #5783, #3642, #21028, #1511, #2206, #347, #28001, #23579, #8745, #10869, #24003, #17436, #25855, #26283, #8887, #4480, #21585, #26428, #15285, #6888, #15140, #6326, #4197, #15428, #21872, #23722, #26135, #21732, #23858, #17153, #6601, #11005, #13136, #15000, #2349, #12856, #19302, #17293, #4060, #12722, #8465, #2061, #10731, #6743, #19579, #11144, #1926, #63, #202, #19717, #12992, #24142, #17577, #4619, #13277, #22007, #19440, #2484, #21448, #6466 ),
 .UNSPECIFIED., .F., .F. ) 
 B_SPLINE_CURVE_WITH_KNOTS ( ( 3, 2, 2, 2, 2, 2, 2, 2, 2, 2, 2, 2, 2, 2, 2, 2, 2, 2, 2, 2, 2, 2, 2, 2, 2, 2, 2, 2, 2, 2, 2, 2, 2, 2, 2, 2, 2, 2, 2, 2, 3 ),
 ( 0.000000000000000000, 0.02500000000000000139, 0.05000000000000000278, 0.07499999999999999722, 0.1000000000000000056, 0.1250000000000000000, 0.1499999999999999944, 0.1749999999999999889, 0.2000000000000000111, 0.2250000000000000056, 0.2500000000000000000, 0.2750000000000000222, 0.2999999999999999889, 0.3250000000000000111, 0.3499999999999999778, 0.3750000000000000000, 0.4000000000000000222, 0.4249999999999999889, 0.4500000000000000111, 0.4749999999999999778, 0.5000000000000000000, 0.5250000000000000222, 0.5500000000000000444, 0.5749999999999999556, 0.5999999999999999778, 0.6250000000000000000, 0.6500000000000000222, 0.6750000000000000444, 0.6999999999999999556, 0.7249999999999999778, 0.7500000000000000000, 0.7750000000000000222, 0.8000000000000000444, 0.8249999999999999556, 0.8499999999999999778, 0.8750000000000000000, 0.9000000000000000222, 0.9250000000000000444, 0.9499999999999999556, 0.9749999999999999778, 1.000000000000000000 ),
 .UNSPECIFIED. ) 
 CURVE ( )  GEOMETRIC_REPRESENTATION_ITEM ( )  RATIONAL_B_SPLINE_CURVE ( ( 1.000000000000000000, 0.9238795325112867385, 1.000000000000000000, 0.9238795325112867385, 1.000000000000000000, 0.9238795325112867385, 1.000000000000000000, 0.9238795325112867385, 1.000000000000000000, 0.9238795325112867385, 1.000000000000000000, 0.9238795325112867385, 1.000000000000000000, 0.9238795325112867385, 1.000000000000000000, 0.9238795325112867385, 1.000000000000000000, 0.9238795325112867385, 1.000000000000000000, 0.9238795325112867385, 1.000000000000000000, 0.9238795325112867385, 1.000000000000000000, 0.9238795325112867385, 1.000000000000000000, 0.9238795325112867385, 1.000000000000000000, 0.9238795325112867385, 1.000000000000000000, 0.9238795325112867385, 1.000000000000000000, 0.9238795325112867385, 1.000000000000000000, 0.9238795325112867385, 1.000000000000000000, 0.9238795325112867385, 1.000000000000000000, 0.9238795325112867385, 1.000000000000000000, 0.9238795325112867385, 1.000000000000000000, 0.9238795325112867385, 1.000000000000000000, 0.9238795325112867385, 1.000000000000000000, 0.9238795325112867385, 1.000000000000000000, 0.9238795325112867385, 1.000000000000000000, 0.9238795325112867385, 1.000000000000000000, 0.9238795325112867385, 1.000000000000000000, 0.9238795325112867385, 1.000000000000000000, 0.9238795325112867385, 1.000000000000000000, 0.9238795325112867385, 1.000000000000000000, 0.9238795325112867385, 1.000000000000000000, 0.9238795325112867385, 1.000000000000000000, 0.9238795325112867385, 1.000000000000000000, 0.9238795325112867385, 1.000000000000000000, 0.9238795325112867385, 1.000000000000000000, 0.9238795325112867385, 1.000000000000000000, 0.9238795325112867385, 1.000000000000000000, 0.9238795325112867385, 1.000000000000000000, 0.9238795325112867385, 1.000000000000000000, 0.9238795325112867385, 1.000000000000000000, 0.9238795325112867385, 1.000000000000000000 ) ) 
 REPRESENTATION_ITEM ( '' )  );
#23870 = CARTESIAN_POINT ( 'NONE',  ( 102.0710678118654329, -4.999999999999989342, 3.437500002731184612 ) ) ;
#23871 = CARTESIAN_POINT ( 'NONE',  ( 124.5550856135277087, 37.42812500108394147, -13.14518615778179900 ) ) ;
#23872 = CARTESIAN_POINT ( 'NONE',  ( 78.14518615778179367, 32.26875000108393721, -5.444914386472297529 ) ) ;
#23873 = CARTESIAN_POINT ( 'NONE',  ( 208.1451861577818079, 38.76757812608393294, -1.609821015232357215E-15 ) ) ;
#23874 = DIRECTION ( 'NONE',  ( 1.000000000000000000, -0.000000000000000000, -5.782411586589357392E-17 ) ) ;
#23875 = CARTESIAN_POINT ( 'NONE',  ( -9.295050272127046043, 32.51679687608393721, -9.295050272127046043 ) ) ;
#23876 = CARTESIAN_POINT ( 'NONE',  ( 138.7583343923579093, 50.00000000000000000, -10.38725784494287296 ) ) ;
#23877 = DIRECTION ( 'NONE',  ( 0.000000000000000000, 0.000000000000000000, -1.000000000000000000 ) ) ;
#23878 = SPHERICAL_SURFACE ( 'NONE', #10852, 5.000000000000000000 ) ;
#23879 = CARTESIAN_POINT ( 'NONE',  ( 99.99999999999998579, 90.00000000000000000, 4.999999999999983125 ) ) ;
#23880 = EDGE_CURVE ( 'NONE', #24292, #15436, #17116, .T. ) ;
#23881 = CARTESIAN_POINT ( 'NONE',  ( 9.295050272127047819, 36.08867187608392868, 9.295050272127046043 ) ) ;
#23882 = CARTESIAN_POINT ( 'NONE',  ( -15.00000000000000355, 80.00000000000000000, -14.99999999999999822 ) ) ;
#23883 = CARTESIAN_POINT ( 'NONE',  ( 104.9999999999999716, 79.56250000273118417, 2.071067811865462627 ) ) ;
#23884 = DIRECTION ( 'NONE',  ( -1.000000000000000000, 0.000000000000000000, 0.000000000000000000 ) ) ;
#23885 = CONICAL_SURFACE ( 'NONE', #26630, 19.22649730810373470, 0.5235987755983000369 ) ;
#23886 = CARTESIAN_POINT ( 'NONE',  ( 2.493653234604083739E-15, 37.22968749999999716, 13.57481594606304576 ) ) ;
#23887 = CARTESIAN_POINT ( 'NONE',  ( 99.99999999999995737, 4.458734125000016313, 8.187500001365592084 ) ) ;
#23888 = VERTEX_POINT ( 'NONE', #16316 ) ;
#23889 = CARTESIAN_POINT ( 'NONE',  ( 99.99999999999998579, 123.9500000010924765, 2.066987299999980099 ) ) ;
#23890 = CARTESIAN_POINT ( 'NONE',  ( 95.54126587499995082, 1.846868145590750077, 13.37500000136559386 ) ) ;
#23891 = CARTESIAN_POINT ( 'NONE',  ( 125.9374164594230763, 50.00000000116060761, 12.98908657125170940 ) ) ;
#23892 = CARTESIAN_POINT ( 'NONE',  ( -13.14518615778179544, 38.17226562608393436, 0.000000000000000000 ) ) ;
#23893 = FACE_OUTER_BOUND ( 'NONE', #23161, .T. ) ;
#23894 = CARTESIAN_POINT ( 'NONE',  ( 99.99999999999995737, 81.43750000136559208, -4.458734125000016313 ) ) ;
#23895 = CARTESIAN_POINT ( 'NONE',  ( 78.14518615778179367, 34.79882812608394005, -1.609821015232357215E-15 ) ) ;
#23896 = CARTESIAN_POINT ( 'NONE',  ( 91.91746824999998466, 112.6261737610028320, -49.22500000273119269 ) ) ;
#23897 = FACE_OUTER_BOUND ( 'NONE', #10030, .T. ) ;
#23898 = APPLICATION_CONTEXT ( 'automotive_design' ) ;
#23899 = FACE_OUTER_BOUND ( 'NONE', #24126, .T. ) ;
#23900 = CARTESIAN_POINT ( 'NONE',  ( 99.99999999999995737, 85.00000000000000000, -3.000000000000018208 ) ) ;
#23901 = CARTESIAN_POINT ( 'NONE',  ( 135.6228728715778971, 38.86679687499999858, 13.57481594606304576 ) ) ;
#23902 = ORIENTED_EDGE ( 'NONE', *, *, #14212, .T. ) ;
#23903 = LINE ( 'NONE', #245, #16375 ) ;
#23904 = CARTESIAN_POINT ( 'NONE',  ( -13.14518615778179900, 36.73359375108393010, -5.444914386472297529 ) ) ;
#23905 = CARTESIAN_POINT ( 'NONE',  ( -13.57481594606304753, 38.66835937716786731, -5.622872871577873077 ) ) ;
#23906 = CARTESIAN_POINT ( 'NONE',  ( 124.5550856135277087, 38.02343750108394005, -13.14518615778179900 ) ) ;
#23907 = CARTESIAN_POINT ( 'NONE',  ( 65.00000000000000000, 34.15390625216787157, 13.57481594606304576 ) ) ;
#23908 = VECTOR ( 'NONE', #24773, 1000.000000000000000 ) ;
#23909 = CARTESIAN_POINT ( 'NONE',  ( 12.66784425494596000, 35.99999999999998579, 4.396229039743023037 ) ) ;
#23910 = CARTESIAN_POINT ( 'NONE',  ( -8.312177448680279460E-16, 32.16953125216787157, -13.57481594606304576 ) ) ;
#23911 = CARTESIAN_POINT ( 'NONE',  ( 103.5355339059327093, -3.535533905932726206, 6.374999999999999112 ) ) ;
#23912 = CARTESIAN_POINT ( 'NONE',  ( 104.9952793366501567, 103.1245878333314465, -49.17499999726881299 ) ) ;
#23913 =( BOUNDED_CURVE ( )  B_SPLINE_CURVE ( 2, ( #28138, #13276, #17725, #4335, #6325, #12855, #24140, #2348, #4196 ),
 .UNSPECIFIED., .F., .F. ) 
 B_SPLINE_CURVE_WITH_KNOTS ( ( 3, 2, 2, 2, 3 ),
 ( 0.08333333333333389770, 0.1250000000000003886, 0.1666666666666668517, 0.2083333333333333426, 0.2499999999999998335 ),
 .UNSPECIFIED. ) 
 CURVE ( )  GEOMETRIC_REPRESENTATION_ITEM ( )  RATIONAL_B_SPLINE_CURVE ( ( 0.9999999999999990008, 0.9238795325112877377, 1.000000000000000000, 0.9238795325112867385, 1.000000000000000000, 0.9238795325112867385, 1.000000000000000000, 0.9238795325112870716, 0.9999999999999996669 ) ) 
 REPRESENTATION_ITEM ( '' )  );
#23914 = CARTESIAN_POINT ( 'NONE',  ( 181.8548138422181921, 34.25312500108393010, 5.444914386472304635 ) ) ;
#23915 = AXIS2_PLACEMENT_3D ( 'NONE', #13116, #27847, #12460 ) ;
#23916 = AXIS2_PLACEMENT_3D ( 'NONE', #23934, #278, #19794 ) ;
#23917 = CARTESIAN_POINT ( 'NONE',  ( -20.00000000000000000, 50.00000000000000000, 10.00000000000000178 ) ) ;
#23918 = CARTESIAN_POINT ( 'NONE',  ( 102.0710678118654755, 81.68750000000001421, -4.999999999999983125 ) ) ;
#23919 = LINE ( 'NONE', #6116, #21440 ) ;
#23920 = EDGE_CURVE ( 'NONE', #8833, #6277, #11018, .T. ) ;
#23921 = LINE ( 'NONE', #17359, #891 ) ;
#23922 = CARTESIAN_POINT ( 'NONE',  ( 208.5748159460630688, 36.63437499999999858, -1.662435489736055892E-15 ) ) ;
#23923 = CARTESIAN_POINT ( 'NONE',  ( -9.598844408820454532, 37.13046874999999147, 9.598844408820459861 ) ) ;
#23924 = CARTESIAN_POINT ( 'NONE',  ( 65.00000000000000000, -7.395377635281828788, -13.57481594606305109 ) ) ;
#23925 = CARTESIAN_POINT ( 'NONE',  ( 13.14518615778179544, 37.97382812608393721, -1.609821015232357215E-15 ) ) ;
#23926 = CARTESIAN_POINT ( 'NONE',  ( -13.14518615778179189, 39.01562500108393294, 5.444914386472304635 ) ) ;
#23927 = CARTESIAN_POINT ( 'NONE',  ( 200.6228728715778686, 34.10429687499999574, 13.57481594606304576 ) ) ;
#23928 = CARTESIAN_POINT ( 'NONE',  ( 112.9999999999999858, 118.0000000000000000, -15.00000000000000533 ) ) ;
#23929 = CARTESIAN_POINT ( 'NONE',  ( 5.622872871577928144, 39.16445312500000142, -13.57481594606299247 ) ) ;
#23930 = CARTESIAN_POINT ( 'NONE',  ( 51.85481384221820633, 36.58476562608393579, 0.000000000000000000 ) ) ;
#23931 = DIRECTION ( 'NONE',  ( 0.000000000000000000, 1.000000000000000000, 0.000000000000000000 ) ) ;
#23932 = FACE_BOUND ( 'NONE', #8599, .T. ) ;
#23933 = CARTESIAN_POINT ( 'NONE',  ( 99.99999999999998579, 93.56249999863440792, -4.458734124999994997 ) ) ;
#23934 = CARTESIAN_POINT ( 'NONE',  ( 65.00000000000000000, 50.00000000000000000, -7.517135062566165128E-15 ) ) ;
#23935 = CARTESIAN_POINT ( 'NONE',  ( 13.57481594606304753, 37.47773437500001137, -5.622872871577873077 ) ) ;
#23936 = ORIENTED_EDGE ( 'NONE', *, *, #19570, .T. ) ;
#23937 = ORIENTED_EDGE ( 'NONE', *, *, #17851, .T. ) ;
#23938 = CARTESIAN_POINT ( 'NONE',  ( 104.9999999999999574, 83.43750000000001421, 2.071067811865462627 ) ) ;
#23939 = VECTOR ( 'NONE', #387, 1000.000000000000000 ) ;
#23940 = CARTESIAN_POINT ( 'NONE',  ( 104.4587341249999781, 95.31249999863440792, -6.938893903907228378E-15 ) ) ;
#23941 = CARTESIAN_POINT ( 'NONE',  ( 99.99999999999998579, 94.81249999863440792, -4.458734124999994997 ) ) ;
#23942 = ORIENTED_EDGE ( 'NONE', *, *, #21918, .T. ) ;
#23943 = EDGE_CURVE ( 'NONE', #1875, #17592, #8309, .T. ) ;
#23944 = CARTESIAN_POINT ( 'NONE',  ( 97.83688103937535629, 116.6573956140660897, -51.40000000000001279 ) ) ;
#23945 = CARTESIAN_POINT ( 'NONE',  ( 70.44491438647230552, 34.65000000108393863, 13.14518615778179189 ) ) ;
#23946 = EDGE_LOOP ( 'NONE', ( #18244, #19186, #18489, #15315, #3344, #18305, #24962, #2286, #1546 ) ) ;
#23947 = CARTESIAN_POINT ( 'NONE',  ( 143.5748159460630688, 39.11484375216787157, -1.662435489736055892E-15 ) ) ;
#23948 = CARTESIAN_POINT ( 'NONE',  ( 101.8468681455906903, -4.458734124999987891, 2.000000001365591640 ) ) ;
#23949 = ORIENTED_EDGE ( 'NONE', *, *, #10285, .F. ) ;
#23950 = CARTESIAN_POINT ( 'NONE',  ( 5.444914386472297529, 34.94765625108394147, -13.14518615778179722 ) ) ;
#23951 = CARTESIAN_POINT ( 'NONE',  ( 9.295050272127047819, 38.66835937608393436, 9.295050272127046043 ) ) ;
#23952 = CARTESIAN_POINT ( 'NONE',  ( 204.5988444088204687, 39.01562500216787299, 9.598844408820456309 ) ) ;
#23953 =( BOUNDED_SURFACE ( )  B_SPLINE_SURFACE ( 1, 2, ( 
 ( #8401, #16951, #14665, #21108, #7855, #23664, #16550, #23387, #4140, #18693, #27808, #25241, #5732, #1595, #27533, #3859, #7990, #23252, #1730, #3727, #10394, #19100, #8264, #25652, #28081, #2145, #11232, #21523, #23798, #26366, #15662, #6680, #19949, #19660, #17377, #26511, #8971, #10807, #25936, #8545, #6826, #24362, #142, #286, #26221, #13075, #19522, #21814, #22093, #15516, #3, #4421, #4704, #9113, #2290, #24224, #10949, #13365, #8828, #8688, #2430, #17518, #6967, #15366, #26073, #17808, #6542, #2571, #4850, #4277, #427, #2003, #10669, #19378, #15222, #4558, #17234, #6411, #15080, #12935, #23940 ),
 ( #24082, #21668, #13220, #21952, #11091, #19802, #17659, #18379, #13795, #27084, #2984, #20233, #22664, #20380, #18524, #9538, #18087, #1150, #2846, #5418, #16374, #15803, #3275, #7537, #14087, #25075, #716, #24790, #22807, #22234, #16235, #20666, #22373, #11658, #5128, #7389, #11515, #13514, #2713, #27229, #9817, #7682, #7248, #22518, #865, #7106, #11374, #11944, #1008, #9391, #20096, #5272, #574, #9255, #17947, #24932, #26658, #24507, #18237, #4994, #13658, #26946, #16082, #26799, #15939, #24655, #13938, #9677, #3134, #11803, #20527, #21216, #5835, #27774, #8232, #20942, #25490, #1700, #25210, #5968, #14772 ) ),
 .UNSPECIFIED., .F., .F., .T. ) 
 B_SPLINE_SURFACE_WITH_KNOTS ( ( 2, 2 ),
 ( 3, 2, 2, 2, 2, 2, 2, 2, 2, 2, 2, 2, 2, 2, 2, 2, 2, 2, 2, 2, 2, 2, 2, 2, 2, 2, 2, 2, 2, 2, 2, 2, 2, 2, 2, 2, 2, 2, 2, 2, 3 ),
 ( 0.000000000000000000, 1.000000000000000000 ),
 ( 0.000000000000000000, 0.02500000000000000139, 0.05000000000000000278, 0.07499999999999999722, 0.1000000000000000056, 0.1250000000000000000, 0.1499999999999999944, 0.1749999999999999889, 0.2000000000000000111, 0.2250000000000000056, 0.2500000000000000000, 0.2750000000000000222, 0.2999999999999999889, 0.3250000000000000111, 0.3499999999999999778, 0.3750000000000000000, 0.4000000000000000222, 0.4249999999999999889, 0.4500000000000000111, 0.4749999999999999778, 0.5000000000000000000, 0.5250000000000000222, 0.5500000000000000444, 0.5749999999999999556, 0.5999999999999999778, 0.6250000000000000000, 0.6500000000000000222, 0.6750000000000000444, 0.6999999999999999556, 0.7249999999999999778, 0.7500000000000000000, 0.7750000000000000222, 0.8000000000000000444, 0.8249999999999999556, 0.8499999999999999778, 0.8750000000000000000, 0.9000000000000000222, 0.9250000000000000444, 0.9499999999999999556, 0.9749999999999999778, 1.000000000000000000 ),
 .UNSPECIFIED. ) 
 GEOMETRIC_REPRESENTATION_ITEM ( )  RATIONAL_B_SPLINE_SURFACE ( (
 ( 1.000000000000000000, 0.9238795325112867385, 1.000000000000000000, 0.9238795325112867385, 1.000000000000000000, 0.9238795325112867385, 1.000000000000000000, 0.9238795325112867385, 1.000000000000000000, 0.9238795325112867385, 1.000000000000000000, 0.9238795325112867385, 1.000000000000000000, 0.9238795325112867385, 1.000000000000000000, 0.9238795325112867385, 1.000000000000000000, 0.9238795325112867385, 1.000000000000000000, 0.9238795325112867385, 1.000000000000000000, 0.9238795325112867385, 1.000000000000000000, 0.9238795325112867385, 1.000000000000000000, 0.9238795325112867385, 1.000000000000000000, 0.9238795325112867385, 1.000000000000000000, 0.9238795325112867385, 1.000000000000000000, 0.9238795325112867385, 1.000000000000000000, 0.9238795325112867385, 1.000000000000000000, 0.9238795325112867385, 1.000000000000000000, 0.9238795325112867385, 1.000000000000000000, 0.9238795325112867385, 1.000000000000000000, 0.9238795325112867385, 1.000000000000000000, 0.9238795325112867385, 1.000000000000000000, 0.9238795325112867385, 1.000000000000000000, 0.9238795325112867385, 1.000000000000000000, 0.9238795325112867385, 1.000000000000000000, 0.9238795325112867385, 1.000000000000000000, 0.9238795325112867385, 1.000000000000000000, 0.9238795325112867385, 1.000000000000000000, 0.9238795325112867385, 1.000000000000000000, 0.9238795325112867385, 1.000000000000000000, 0.9238795325112867385, 1.000000000000000000, 0.9238795325112867385, 1.000000000000000000, 0.9238795325112867385, 1.000000000000000000, 0.9238795325112867385, 1.000000000000000000, 0.9238795325112867385, 1.000000000000000000, 0.9238795325112867385, 1.000000000000000000, 0.9238795325112867385, 1.000000000000000000, 0.9238795325112867385, 1.000000000000000000, 0.9238795325112867385, 1.000000000000000000, 0.9238795325112867385, 1.000000000000000000),
 ( 1.000000000000000000, 0.9238795325112867385, 1.000000000000000000, 0.9238795325112867385, 1.000000000000000000, 0.9238795325112867385, 1.000000000000000000, 0.9238795325112867385, 1.000000000000000000, 0.9238795325112867385, 1.000000000000000000, 0.9238795325112867385, 1.000000000000000000, 0.9238795325112867385, 1.000000000000000000, 0.9238795325112867385, 1.000000000000000000, 0.9238795325112867385, 1.000000000000000000, 0.9238795325112867385, 1.000000000000000000, 0.9238795325112867385, 1.000000000000000000, 0.9238795325112867385, 1.000000000000000000, 0.9238795325112867385, 1.000000000000000000, 0.9238795325112867385, 1.000000000000000000, 0.9238795325112867385, 1.000000000000000000, 0.9238795325112867385, 1.000000000000000000, 0.9238795325112867385, 1.000000000000000000, 0.9238795325112867385, 1.000000000000000000, 0.9238795325112867385, 1.000000000000000000, 0.9238795325112867385, 1.000000000000000000, 0.9238795325112867385, 1.000000000000000000, 0.9238795325112867385, 1.000000000000000000, 0.9238795325112867385, 1.000000000000000000, 0.9238795325112867385, 1.000000000000000000, 0.9238795325112867385, 1.000000000000000000, 0.9238795325112867385, 1.000000000000000000, 0.9238795325112867385, 1.000000000000000000, 0.9238795325112867385, 1.000000000000000000, 0.9238795325112867385, 1.000000000000000000, 0.9238795325112867385, 1.000000000000000000, 0.9238795325112867385, 1.000000000000000000, 0.9238795325112867385, 1.000000000000000000, 0.9238795325112867385, 1.000000000000000000, 0.9238795325112867385, 1.000000000000000000, 0.9238795325112867385, 1.000000000000000000, 0.9238795325112867385, 1.000000000000000000, 0.9238795325112867385, 1.000000000000000000, 0.9238795325112867385, 1.000000000000000000, 0.9238795325112867385, 1.000000000000000000, 0.9238795325112867385, 1.000000000000000000) ) ) 
 REPRESENTATION_ITEM ( '' )  SURFACE ( )  );
#23954 = EDGE_CURVE ( 'NONE', #17777, #15111, #23019, .T. ) ;
#23955 = CARTESIAN_POINT ( 'NONE',  ( -13.14518615778179189, 35.04687500108393294, 5.444914386472304635 ) ) ;
#23956 = CARTESIAN_POINT ( 'NONE',  ( 108.0825317500000011, 107.3738262389971680, -44.22500000273119269 ) ) ;
#23957 = CARTESIAN_POINT ( 'NONE',  ( 135.4449143864723339, 37.03125000108393294, 13.14518615778179189 ) ) ;
#23958 = ORIENTED_EDGE ( 'NONE', *, *, #25711, .F. ) ;
#23959 = CARTESIAN_POINT ( 'NONE',  ( -13.14518615778179900, 38.32109375108394289, -5.444914386472297529 ) ) ;
#23960 = CARTESIAN_POINT ( 'NONE',  ( 135.4449143864723055, 34.74921875108394431, -13.14518615778179900 ) ) ;
#23961 = CARTESIAN_POINT ( 'NONE',  ( 55.40115559117954547, 33.75703124999999005, -9.598844408820458085 ) ) ;
#23962 = CARTESIAN_POINT ( 'NONE',  ( 112.9999999999999858, 125.0000000000000000, -13.00000000000001066 ) ) ;
#23963 = EDGE_CURVE ( 'NONE', #12415, #3280, #26032, .T. ) ;
#23964 = CARTESIAN_POINT ( 'NONE',  ( 103.1528011352953342, -3.152801135295355106, 12.06250000136559208 ) ) ;
#23965 = DIRECTION ( 'NONE',  ( 0.000000000000000000, 1.000000000000000000, 0.000000000000000000 ) ) ;
#23966 = CARTESIAN_POINT ( 'NONE',  ( 98.15313185440923860, 4.458734125000016313, 13.25000000136559564 ) ) ;
#23967 = CARTESIAN_POINT ( 'NONE',  ( 97.50236033167492167, 102.3130555110000159, -52.72500000273119980 ) ) ;
#23968 = CARTESIAN_POINT ( 'NONE',  ( 102.4999999999999858, 123.7999999999999972, -9.847140817659276890E-15 ) ) ;
#23969 = CARTESIAN_POINT ( 'NONE',  ( 98.15313185440923860, 80.50000000136560629, -4.458734125000016313 ) ) ;
#23970 = CARTESIAN_POINT ( 'NONE',  ( 104.9952793366501567, 116.8754121666685393, -46.32499999726881867 ) ) ;
#23971 = CARTESIAN_POINT ( 'NONE',  ( 9.295050272127047819, 37.87460937608393863, 9.295050272127046043 ) ) ;
#23972 = ADVANCED_FACE ( 'NONE', ( #14164 ), #18736, .F. ) ;
#23973 = CARTESIAN_POINT ( 'NONE',  ( 91.91746824999997045, 112.6261737610028320, -49.97499999726881725 ) ) ;
#23974 = ORIENTED_EDGE ( 'NONE', *, *, #7379, .F. ) ;
#23975 = CARTESIAN_POINT ( 'NONE',  ( 93.00000000000000000, 112.2744378736303190, -50.60000000546237686 ) ) ;
#23976 = AXIS2_PLACEMENT_3D ( 'NONE', #15212, #23931, #2280 ) ;
#23977 = CARTESIAN_POINT ( 'NONE',  ( 97.92893218813456713, 79.93750000273118417, -5.000000000000067502 ) ) ;
#23978 = CARTESIAN_POINT ( 'NONE',  ( 99.99999999999998579, 137.0000000000000000, -5.204170427930421283E-15 ) ) ;
#23979 = CARTESIAN_POINT ( 'NONE',  ( 195.0000000000000000, 40.35507812608393152, -13.14518615778179544 ) ) ;
#23980 = ORIENTED_EDGE ( 'NONE', *, *, #4292, .F. ) ;
#23981 = CARTESIAN_POINT ( 'NONE',  ( 78.14518615778180788, 36.43593750108394147, -5.444914386472297529 ) ) ;
#23982 = DIRECTION ( 'NONE',  ( 0.000000000000000000, -0.000000000000000000, 1.000000000000000000 ) ) ;
#23983 = CARTESIAN_POINT ( 'NONE',  ( 99.99999999999995737, 4.458734125000016313, 13.43750000136559386 ) ) ;
#23984 = ORIENTED_EDGE ( 'NONE', *, *, #5147, .F. ) ;
#23985 = CARTESIAN_POINT ( 'NONE',  ( 104.3262379212492590, 115.9545556584642867, -52.70000000000000284 ) ) ;
#23986 = CARTESIAN_POINT ( 'NONE',  ( -8.049105076161786076E-16, 39.56132812608393579, -13.14518615778179544 ) ) ;
#23987 = CARTESIAN_POINT ( 'NONE',  ( 99.99999999999998579, 92.62499999726881583, 4.999999999999984013 ) ) ;
#23988 = CARTESIAN_POINT ( 'NONE',  ( 116.8548138422182063, 39.80937500108392868, 5.444914386472304635 ) ) ;
#23989 = CARTESIAN_POINT ( 'NONE',  ( 5.444914386472302859, 40.20625000108394431, 13.14518615778179189 ) ) ;
#23990 = CARTESIAN_POINT ( 'NONE',  ( 102.0710678118654613, 93.06249999726880162, -4.999999999999997335 ) ) ;
#23991 = VECTOR ( 'NONE', #2733, 1000.000000000000000 ) ;
#23992 = CARTESIAN_POINT ( 'NONE',  ( 65.00000000000000000, 37.77539062608393294, 13.14518615778179544 ) ) ;
#23993 = DIRECTION ( 'NONE',  ( 1.000000000000000000, 0.000000000000000000, -5.782411586589357392E-17 ) ) ;
#23994 = ORIENTED_EDGE ( 'NONE', *, *, #16966, .F. ) ;
#23995 = EDGE_CURVE ( 'NONE', #25848, #11744, #15105, .T. ) ;
#23996 = CARTESIAN_POINT ( 'NONE',  ( 195.0000000000000000, 36.18789062608393436, 13.14518615778179544 ) ) ;
#23997 = ORIENTED_EDGE ( 'NONE', *, *, #88, .F. ) ;
#23998 = EDGE_LOOP ( 'NONE', ( #26726, #24173, #3163, #26741 ) ) ;
#23999 = VERTEX_POINT ( 'NONE', #14020 ) ;
#24000 = CARTESIAN_POINT ( 'NONE',  ( 2.414731522848535132E-15, 37.77539062608393294, 13.14518615778179544 ) ) ;
#24001 = CARTESIAN_POINT ( 'NONE',  ( 98.15313185440923860, 4.458734125000016313, 9.500000001365593860 ) ) ;
#24002 = CARTESIAN_POINT ( 'NONE',  ( 74.29505027212704249, 40.05742187608392868, 9.295050272127046043 ) ) ;
#24003 = CARTESIAN_POINT ( 'NONE',  ( 95.54126587499996504, 82.50000000136560629, 1.846868145590724986 ) ) ;
#24004 = CARTESIAN_POINT ( 'NONE',  ( 195.0000000000000000, 40.35507812608393152, -13.14518615778179544 ) ) ;
#24005 = CARTESIAN_POINT ( 'NONE',  ( 13.14518615778179722, 37.13046875108393863, 5.444914386472293977 ) ) ;
#24006 = CARTESIAN_POINT ( 'NONE',  ( 188.8389378251398796, 51.27996893916986210, 14.99999999999857891 ) ) ;
#24007 = DIRECTION ( 'NONE',  ( 0.000000000000000000, 0.000000000000000000, 1.000000000000000000 ) ) ;
#24008 = CARTESIAN_POINT ( 'NONE',  ( 208.1451861577818079, 40.35507812608393863, -1.609821015232357215E-15 ) ) ;
#24009 = CARTESIAN_POINT ( 'NONE',  ( 99.99999999999997158, 101.5015231886685854, -51.12499999726882294 ) ) ;
#24010 = ORIENTED_EDGE ( 'NONE', *, *, #9714, .T. ) ;
#24011 = CARTESIAN_POINT ( 'NONE',  ( 2.493653234604083739E-15, 38.02343749999999289, 13.57481594606304576 ) ) ;
#24012 = CARTESIAN_POINT ( 'NONE',  ( -5.444914386472297529, 38.02343750108394005, -13.14518615778179900 ) ) ;
#24013 = CARTESIAN_POINT ( 'NONE',  ( 94.99999999999995737, -2.071067811865466624, 0.1875000027311852502 ) ) ;
#24014 = CARTESIAN_POINT ( 'NONE',  ( 143.1451861577818079, 36.38632812608393863, -1.609821015232357215E-15 ) ) ;
#24015 = CARTESIAN_POINT ( 'NONE',  ( 70.44491438647230552, 35.24531250108393010, 13.14518615778179189 ) ) ;
#24016 = CARTESIAN_POINT ( 'NONE',  ( 185.7049497278729575, 35.89023437608393152, -9.295050272127046043 ) ) ;
#24017 = VERTEX_POINT ( 'NONE', #8036 ) ;
#24018 = FACE_OUTER_BOUND ( 'NONE', #27566, .T. ) ;
#24019 = SURFACE_STYLE_FILL_AREA ( #219 ) ;
#24020 = CARTESIAN_POINT ( 'NONE',  ( 136.4508793426651607, 50.00000000106927445, -11.97362904075493084 ) ) ;
#24021 = CARTESIAN_POINT ( 'NONE',  ( -18.00000000000000355, 80.00000000000000000, 15.00000000000000178 ) ) ;
#24022 = CARTESIAN_POINT ( 'NONE',  ( -20.00000000000000355, 55.00000000000000000, -14.99999999999999822 ) ) ;
#24023 = CARTESIAN_POINT ( 'NONE',  ( 91.91746824999999887, 110.0000000000000000, -53.12500000273119838 ) ) ;
#24024 = CARTESIAN_POINT ( 'NONE',  ( -13.14518615778179189, 36.63437500108393152, 5.444914386472304635 ) ) ;
#24025 = CARTESIAN_POINT ( 'NONE',  ( -9.180175813647995398, 55.00000000000000000, 15.00000000000000000 ) ) ;
#24026 = CARTESIAN_POINT ( 'NONE',  ( 102.0710678118653760, 79.43750000273119838, 5.000000000000054179 ) ) ;
#24027 = CARTESIAN_POINT ( 'NONE',  ( 55.81982418635200816, 50.00000000000000000, 9.999999999999984013 ) ) ;
#24028 = DIRECTION ( 'NONE',  ( 0.000000000000000000, 0.000000000000000000, 1.000000000000000000 ) ) ;
#24029 = CARTESIAN_POINT ( 'NONE',  ( 103.1528011352953342, -3.152801135295355106, 6.812500001365592084 ) ) ;
#24030 = CARTESIAN_POINT ( 'NONE',  ( 98.53841926354351699, 124.4500000010924765, -1.461580736456474794 ) ) ;
#24031 = CARTESIAN_POINT ( 'NONE',  ( 101.8468681455906903, -4.458734124999987891, 12.75000000136559386 ) ) ;
#24032 = CARTESIAN_POINT ( 'NONE',  ( 130.8765262653674881, 51.45968077934806217, 14.99999999999996625 ) ) ;
#24033 = CARTESIAN_POINT ( 'NONE',  ( -9.295050272127046043, 39.66054687608393436, -9.295050272127046043 ) ) ;
#24034 = CARTESIAN_POINT ( 'NONE',  ( 124.3771271284221740, 38.56914062716787583, -13.57481594606310260 ) ) ;
#24035 = DIRECTION ( 'NONE',  ( 0.000000000000000000, 0.000000000000000000, 1.000000000000000000 ) ) ;
#24036 = CARTESIAN_POINT ( 'NONE',  ( 78.14518615778179367, 35.59257812608393579, -1.609821015232357215E-15 ) ) ;
#24037 = CARTESIAN_POINT ( 'NONE',  ( 104.9952793366501851, 116.8754121666685393, -53.82500000273119412 ) ) ;
#24038 = CARTESIAN_POINT ( 'NONE',  ( 5.444914386472297529, 37.92421875108393436, -13.14518615778179722 ) ) ;
#24039 =( BOUNDED_CURVE ( )  B_SPLINE_CURVE ( 2, ( #20952, #5844, #27783, #5979, #20814, #14646, #1292, #1162, #14514 ),
 .UNSPECIFIED., .F., .F. ) 
 B_SPLINE_CURVE_WITH_KNOTS ( ( 3, 2, 2, 2, 3 ),
 ( 0.000000000000000000, 0.008928571428571436749, 0.01785714285714287350, 0.02678571428571431198, 0.03571428571428574700 ),
 .UNSPECIFIED. ) 
 CURVE ( )  GEOMETRIC_REPRESENTATION_ITEM ( )  RATIONAL_B_SPLINE_CURVE ( ( 1.000000000000000000, 0.9238795325112867385, 1.000000000000000000, 0.9238795325112867385, 1.000000000000000000, 0.9238795325112867385, 1.000000000000000000, 0.9238795325112864054, 1.000000000000000222 ) ) 
 REPRESENTATION_ITEM ( '' )  );
#24040 =( BOUNDED_CURVE ( )  B_SPLINE_CURVE ( 2, ( #882, #18255, #24947, #17823, #26528, #26819, #5434, #14101, #9269, #9406, #734 ),
 .UNSPECIFIED., .F., .F. ) 
 B_SPLINE_CURVE_WITH_KNOTS ( ( 3, 2, 2, 2, 2, 3 ),
 ( 0.3000000000000002109, 0.3200000000000001177, 0.3400000000000000244, 0.3599999999999998757, 0.3799999999999997824, 0.3999999999999996891 ),
 .UNSPECIFIED. ) 
 CURVE ( )  GEOMETRIC_REPRESENTATION_ITEM ( )  RATIONAL_B_SPLINE_CURVE ( ( 0.9999999999999994449, 0.9510565162951540863, 1.000000000000000000, 0.9510565162951535312, 1.000000000000000000, 0.9510565162951535312, 1.000000000000000000, 0.9510565162951535312, 1.000000000000000000, 0.9510565162951543083, 0.9999999999999992228 ) ) 
 REPRESENTATION_ITEM ( '' )  );
#24041 = CARTESIAN_POINT ( 'NONE',  ( -2.407595600654690178E-15, 10.00000000000000178, -16.91709623134523000 ) ) ;
#24042 = CARTESIAN_POINT ( 'NONE',  ( 116.4251840539369738, 36.28710937499999289, 5.622872871577880183 ) ) ;
#24043 = CARTESIAN_POINT ( 'NONE',  ( 99.99999999999995737, 82.75000000000000000, -5.000000000000018652 ) ) ;
#24044 = CARTESIAN_POINT ( 'NONE',  ( 139.5988444088204687, 36.53515624999999289, 9.598844408820456309 ) ) ;
#24045 = ORIENTED_EDGE ( 'NONE', *, *, #14556, .T. ) ;
#24046 = DIRECTION ( 'NONE',  ( 0.000000000000000000, -1.000000000000000000, 0.000000000000000000 ) ) ;
#24047 = EDGE_CURVE ( 'NONE', #26226, #15733, #3770, .T. ) ;
#24048 = CARTESIAN_POINT ( 'NONE',  ( -5.444914386472297529, 36.63437500108393152, -13.14518615778179900 ) ) ;
#24049 = CARTESIAN_POINT ( 'NONE',  ( -13.57481594606304753, 37.08085937716786873, -5.622872871577873077 ) ) ;
#24050 = CARTESIAN_POINT ( 'NONE',  ( 120.7049497278729575, 36.48554687608393721, -9.295050272127046043 ) ) ;
#24051 = CARTESIAN_POINT ( 'NONE',  ( 74.59884440882045453, 32.66562500216787157, 9.598844408820456309 ) ) ;
#24052 = LINE ( 'NONE', #13189, #5244 ) ;
#24053 = CARTESIAN_POINT ( 'NONE',  ( -13.57481594606304753, 33.90585937716787868, -5.622872871577873077 ) ) ;
#24054 = CARTESIAN_POINT ( 'NONE',  ( 102.0710678118654329, 5.000000000000018652, 6.687499999999999112 ) ) ;
#24055 = CARTESIAN_POINT ( 'NONE',  ( 91.91746824999997045, 107.3738262389971680, -47.77499999726881441 ) ) ;
#24056 = MECHANICAL_DESIGN_GEOMETRIC_PRESENTATION_REPRESENTATION (  '', ( #24512 ), #9022 ) ;
#24057 = CARTESIAN_POINT ( 'NONE',  ( 204.2950502721270425, 33.90585937608393152, -9.295050272127046043 ) ) ;
#24058 = CYLINDRICAL_SURFACE ( 'NONE', #24743, 4.999999999999989342 ) ;
#24060 = ORIENTED_EDGE ( 'NONE', *, *, #20331, .T. ) ;
#24059 = FACE_OUTER_BOUND ( 'NONE', #9073, .T. ) ;
#24061 = CARTESIAN_POINT ( 'NONE',  ( 65.00000000000000000, 37.32890625216786873, 13.57481594606304576 ) ) ;
#24062 = CARTESIAN_POINT ( 'NONE',  ( 133.7974518689580350, 54.08938259242986391, 14.99999999999996447 ) ) ;
#24063 = CARTESIAN_POINT ( 'NONE',  ( -5.622872871577873077, 36.38632812499999858, 13.57481594606304753 ) ) ;
#24064 = APPLICATION_CONTEXT ( 'automotive_design' ) ;
#24065 = CARTESIAN_POINT ( 'NONE',  ( 1.464337720320554093, 36.00000000000002842, -13.46163418879032037 ) ) ;
#24066 = CARTESIAN_POINT ( 'NONE',  ( -13.14518615778179900, 37.52734375108393294, -5.444914386472297529 ) ) ;
#24067 = CARTESIAN_POINT ( 'NONE',  ( -13.14518615778179900, 35.74140625108393721, -5.444914386472297529 ) ) ;
#24068 = CARTESIAN_POINT ( 'NONE',  ( 181.4251840539369596, 35.49335937499999005, 5.622872871577880183 ) ) ;
#24069 = CARTESIAN_POINT ( 'NONE',  ( 102.4976396683250925, 117.6869444889999841, -45.97500000273119269 ) ) ;
#24070 = CARTESIAN_POINT ( 'NONE',  ( 5.622872871577912157, 38.86679687500001279, 13.57481594606301023 ) ) ;
#24071 = CARTESIAN_POINT ( 'NONE',  ( 55.70494972787295751, 34.10429687608393579, -9.295050272127046043 ) ) ;
#24072 = CARTESIAN_POINT ( 'NONE',  ( 96.84719886470459471, 3.152801135295383084, 2.312500001365592084 ) ) ;
#24073 = CARTESIAN_POINT ( 'NONE',  ( 99.99999999999998579, 102.6397644303321215, -44.00000000546238255 ) ) ;
#24074 = CARTESIAN_POINT ( 'NONE',  ( 103.1528011352953484, 95.18749999863440792, 3.152801135295352886 ) ) ;
#24075 = CARTESIAN_POINT ( 'NONE',  ( -13.57481594606304576, 37.82499999999999574, 0.000000000000000000 ) ) ;
#24076 = CARTESIAN_POINT ( 'NONE',  ( 143.1451861577818079, 36.38632812608393863, -1.609821015232357215E-15 ) ) ;
#24077 = VERTEX_POINT ( 'NONE', #9614 ) ;
#24078 = CARTESIAN_POINT ( 'NONE',  ( 94.99999999999995737, 84.06250000000000000, 2.071067811865466624 ) ) ;
#24079 = EDGE_CURVE ( 'NONE', #19393, #16078, #26539, .T. ) ;
#24080 = AXIS2_PLACEMENT_3D ( 'NONE', #19502, #15346, #3984 ) ;
#24081 = CARTESIAN_POINT ( 'NONE',  ( 104.9999999999999574, 80.68750000273119838, -2.071067811865491937 ) ) ;
#24082 = CARTESIAN_POINT ( 'NONE',  ( 104.9999999999999858, 90.00000000000000000, -6.938893903907228378E-15 ) ) ;
#24083 = CARTESIAN_POINT ( 'NONE',  ( 53.30962175448677698, 35.99999999999999289, -6.307928093363390332 ) ) ;
#24084 = B_SPLINE_CURVE_WITH_KNOTS ( 'NONE', 3,
 ( #12337, #26922, #27479, #13915, #1401, #18639, #5250, #27343, #22642, #16207, #3110, #23056, #14338, #3382, #12053, #24911, #842, #11779, #985, #1125, #12190, #20779, #5394, #18213, #3533, #1261, #14063, #9923, #20919, #3675, #7802 ),
 .UNSPECIFIED., .F., .F.,
 ( 4, 2, 2, 2, 2, 2, 2, 2, 2, 2, 1, 2, 2, 2, 2, 4 ),
 ( 1.261830988103825351E-15, 0.001656255954915028267, 0.003312511909828794957, 0.004968767864742561213, 0.005796895842199402925, 0.006625023819656245504, 0.008281279774569928059, 0.009937535729483611482, 0.01325004763931101823, 0.01490630359422470512, 0.01656255954913839548, 0.01821881550405208064, 0.01987507145896576580, 0.02318758336879312223, 0.02484383932370680045, 0.02650009527862047173 ),
 .UNSPECIFIED. ) ;
#24085 =( BOUNDED_CURVE ( )  B_SPLINE_CURVE ( 2, ( #19567, #17425, #9161, #4604, #17991, #26416, #26701, #10993, #24555, #191, #13263, #23989, #5036, #13125, #26123, #17714, #15559, #6589, #2615, #21860, #2335, #19706, #8873, #22137, #11278, #17853, #478, #26556, #9436, #3457, #20427, #26849, #3318, #15985, #7586, #9581, #7728, #9863, #16419, #14269, #25116, #11849, #9724, #5603, #16279, #20571, #12123, #911, #20276, #1052, #27134, #3179, #5742, #11989, #26991, #20849, #18285, #1329, #7867, #13981, #24699, #763, #7436, #24978, #5461, #9995, #11702, #22988, #18703, #16131, #14130, #22419, #18136, #27406, #7296, #16561, #20713, #5177, #1195, #13841, #24839, #22709, #25252, #22566, #3033, #2890, #11560, #5322, #27273, #18426, #22851, #18570, #12535, #10264, #23127, #27958, #10410 ),
 .UNSPECIFIED., .F., .F. ) 
 B_SPLINE_CURVE_WITH_KNOTS ( ( 3, 2, 2, 2, 2, 2, 2, 2, 2, 2, 2, 2, 2, 2, 2, 2, 2, 2, 2, 2, 2, 2, 2, 2, 2, 2, 2, 2, 2, 2, 2, 2, 2, 2, 2, 2, 2, 2, 2, 2, 2, 2, 2, 2, 2, 2, 2, 2, 3 ),
 ( 0.000000000000000000, 0.01041666666666666609, 0.02083333333333333218, 0.03125000000000000000, 0.04166666666666666435, 0.05208333333333333565, 0.06250000000000000000, 0.07291666666666667129, 0.08333333333333332871, 0.09374999999999998612, 0.1041666666666666713, 0.1145833333333333287, 0.1250000000000000000, 0.1354166666666666574, 0.1458333333333333426, 0.1562500000000000000, 0.1666666666666666574, 0.1770833333333333426, 0.1874999999999999722, 0.1979166666666666574, 0.2083333333333333426, 0.2187500000000000000, 0.2291666666666666574, 0.2395833333333333426, 0.2500000000000000000, 0.2604166666666666852, 0.2708333333333333148, 0.2812500000000000000, 0.2916666666666666852, 0.3020833333333333148, 0.3125000000000000000, 0.3229166666666666852, 0.3333333333333333148, 0.3437500000000000000, 0.3541666666666666852, 0.3645833333333333148, 0.3749999999999999445, 0.3854166666666666852, 0.3958333333333333148, 0.4062500000000000000, 0.4166666666666666852, 0.4270833333333333148, 0.4375000000000000000, 0.4479166666666666852, 0.4583333333333333148, 0.4687500000000000000, 0.4791666666666666852, 0.4895833333333333148, 0.4988304892921909817 ),
 .UNSPECIFIED. ) 
 CURVE ( )  GEOMETRIC_REPRESENTATION_ITEM ( )  RATIONAL_B_SPLINE_CURVE ( ( 1.000000000000000000, 0.9238795325112867385, 1.000000000000000000, 0.9238795325112867385, 1.000000000000000000, 0.9238795325112867385, 1.000000000000000000, 0.9238795325112867385, 1.000000000000000000, 0.9238795325112867385, 1.000000000000000000, 0.9238795325112867385, 1.000000000000000000, 0.9238795325112867385, 1.000000000000000000, 0.9238795325112867385, 1.000000000000000000, 0.9238795325112867385, 1.000000000000000000, 0.9238795325112867385, 1.000000000000000000, 0.9238795325112867385, 1.000000000000000000, 0.9238795325112867385, 1.000000000000000000, 0.9238795325112867385, 1.000000000000000000, 0.9238795325112867385, 1.000000000000000000, 0.9238795325112867385, 1.000000000000000000, 0.9238795325112867385, 1.000000000000000000, 0.9238795325112867385, 1.000000000000000000, 0.9238795325112867385, 1.000000000000000000, 0.9238795325112867385, 1.000000000000000000, 0.9238795325112867385, 1.000000000000000000, 0.9238795325112867385, 1.000000000000000000, 0.9238795325112867385, 1.000000000000000000, 0.9238795325112867385, 1.000000000000000000, 0.9238795325112867385, 1.000000000000000000, 0.9238795325112867385, 1.000000000000000000, 0.9238795325112867385, 1.000000000000000000, 0.9238795325112867385, 1.000000000000000000, 0.9238795325112867385, 1.000000000000000000, 0.9238795325112867385, 1.000000000000000000, 0.9238795325112867385, 1.000000000000000000, 0.9238795325112867385, 1.000000000000000000, 0.9238795325112867385, 1.000000000000000000, 0.9238795325112867385, 1.000000000000000000, 0.9238795325112867385, 1.000000000000000000, 0.9238795325112867385, 1.000000000000000000, 0.9238795325112867385, 1.000000000000000000, 0.9238795325112867385, 1.000000000000000000, 0.9238795325112867385, 1.000000000000000000, 0.9238795325112867385, 1.000000000000000000, 0.9238795325112867385, 1.000000000000000000, 0.9238795325112867385, 1.000000000000000000, 0.9238795325112867385, 1.000000000000000000, 0.9238795325112867385, 1.000000000000000000, 0.9238795325112867385, 1.000000000000000000, 0.9238795325112867385, 1.000000000000000000, 0.9238795325112867385, 1.000000000000000000, 0.9238795325112867385, 1.000000000000000000, 0.9324258078851886955, 0.9848264816800353927 ) ) 
 REPRESENTATION_ITEM ( '' )  );
#24086 = CARTESIAN_POINT ( 'NONE',  ( 93.00000000000000000, 107.7255621263696526, -50.90000000000001990 ) ) ;
#24087 = CARTESIAN_POINT ( 'NONE',  ( 51.85481384221820633, 34.45156250108394147, 5.444914386472304635 ) ) ;
#24088 = ORIENTED_EDGE ( 'NONE', *, *, #19982, .T. ) ;
#24089 = CARTESIAN_POINT ( 'NONE',  ( 94.99999999999995737, 1.387778780781445676E-14, 0.000000000000000000 ) ) ;
#24090 = CARTESIAN_POINT ( 'NONE',  ( 98.15313185440925281, -4.458734124999987891, 2.875000001365592084 ) ) ;
#24091 = ORIENTED_EDGE ( 'NONE', *, *, #24711, .F. ) ;
#24092 = DIRECTION ( 'NONE',  ( 0.000000000000000000, -1.000000000000000000, 0.000000000000000000 ) ) ;
#24093 = CARTESIAN_POINT ( 'NONE',  ( 9.295050272127046043, 38.07304687608393579, -9.295050272127046043 ) ) ;
#24094 = CARTESIAN_POINT ( 'NONE',  ( 189.3771271284221314, 34.10429687716786873, 13.57481594606304753 ) ) ;
#24095 = CARTESIAN_POINT ( 'NONE',  ( -8.049105076161786076E-16, 34.79882812608393294, -13.14518615778179544 ) ) ;
#24096 = CARTESIAN_POINT ( 'NONE',  ( 5.622872871577870413, 36.88242187716787157, -13.57481594606304753 ) ) ;
#24097 = CARTESIAN_POINT ( 'NONE',  ( 130.0000000000000000, 36.18789062608393436, 13.14518615778179544 ) ) ;
#24098 = CARTESIAN_POINT ( 'NONE',  ( 5.444914386472297529, 39.71015625108393010, -13.14518615778179900 ) ) ;
#24099 = CARTESIAN_POINT ( 'NONE',  ( 124.5550856135277087, 34.05468750108393294, -13.14518615778179900 ) ) ;
#24100 = CARTESIAN_POINT ( 'NONE',  ( 70.62287287157788285, 35.69179687499999432, 13.57481594606304576 ) ) ;
#24101 = CARTESIAN_POINT ( 'NONE',  ( 103.5355339059327235, 91.87500000000000000, 3.535533905932724874 ) ) ;
#24102 = CARTESIAN_POINT ( 'NONE',  ( 98.15313185440925281, 4.458734125000016313, 10.50000000136559208 ) ) ;
#24103 = CARTESIAN_POINT ( 'NONE',  ( 181.4251840539369596, 37.08085937499999574, 5.622872871577880183 ) ) ;
#24104 = EDGE_CURVE ( 'NONE', #15121, #17145, #27872, .T. ) ;
#24105 = CARTESIAN_POINT ( 'NONE',  ( 101.8468681455906903, 4.458734125000016313, 1.125000001365592750 ) ) ;
#24106 = CARTESIAN_POINT ( 'NONE',  ( 108.0825317500000153, 110.0000000000000000, -52.12500000273119838 ) ) ;
#24107 = CARTESIAN_POINT ( 'NONE',  ( 5.622872871577742515, 38.96601562716787015, 13.57481594606318076 ) ) ;
#24108 = CYLINDRICAL_SURFACE ( 'NONE', #15250, 5.000000000000004441 ) ;
#24109 = CARTESIAN_POINT ( 'NONE',  ( 93.46109445667489979, 105.2492070361643215, -51.42499999726882010 ) ) ;
#24110 = CARTESIAN_POINT ( 'NONE',  ( -9.295050272127046043, 36.68398437608393436, -9.295050272127046043 ) ) ;
#24111 = VECTOR ( 'NONE', #26273, 1000.000000000000000 ) ;
#24112 = CARTESIAN_POINT ( 'NONE',  ( 95.00472066334982912, 103.1245878333314323, -51.57499999726880446 ) ) ;
#24113 = VERTEX_POINT ( 'NONE', #6051 ) ;
#24114 = CARTESIAN_POINT ( 'NONE',  ( 102.0669873000000081, 124.4000000010924651, -0.8561741729129508371 ) ) ;
#24116 = EDGE_CURVE ( 'NONE', #18823, #13418, #25868, .T. ) ;
#24115 = CARTESIAN_POINT ( 'NONE',  ( 101.4615807364564546, 123.2500000010924879, 1.461580736456455476 ) ) ;
#24117 = CARTESIAN_POINT ( 'NONE',  ( 214.9999999999999716, 55.00000000000000000, 14.99999999999994493 ) ) ;
#24118 = EDGE_CURVE ( 'NONE', #19624, #2438, #23339, .T. ) ;
#24119 = CARTESIAN_POINT ( 'NONE',  ( 181.8548138422181921, 39.80937500108392868, 5.444914386472304635 ) ) ;
#24120 =( BOUNDED_CURVE ( )  B_SPLINE_CURVE ( 2, ( #11672, #587, #17676, #22107, #15816 ),
 .UNSPECIFIED., .F., .F. ) 
 B_SPLINE_CURVE_WITH_KNOTS ( ( 3, 2, 3 ),
 ( 0.4375000000000003331, 0.4479166666666667962, 0.4520580917964571177 ),
 .UNSPECIFIED. ) 
 CURVE ( )  GEOMETRIC_REPRESENTATION_ITEM ( )  RATIONAL_B_SPLINE_CURVE ( ( 0.9999999999999975575, 0.9238795325112891810, 1.000000000000000000, 0.9697362671728813055, 0.9635368512068493985 ) ) 
 REPRESENTATION_ITEM ( '' )  );
#24121 = VERTEX_POINT ( 'NONE', #23849 ) ;
#24122 = DIRECTION ( 'NONE',  ( -0.000000000000000000, -1.000000000000000000, -0.000000000000000000 ) ) ;
#24123 = EDGE_CURVE ( 'NONE', #22244, #9281, #8454, .T. ) ;
#24124 = FACE_OUTER_BOUND ( 'NONE', #8432, .T. ) ;
#24125 = CARTESIAN_POINT ( 'NONE',  ( 99.99999999999995737, -4.458734124999988779, 13.93750000136559208 ) ) ;
#24126 = EDGE_LOOP ( 'NONE', ( #3520, #5075, #2463, #12863 ) ) ;
#24127 = CARTESIAN_POINT ( 'NONE',  ( 95.67376207875072680, 115.9545556584642867, -48.30000000000001137 ) ) ;
#24128 = CARTESIAN_POINT ( 'NONE',  ( 9.295050272127046043, 38.66835937608393436, -9.295050272127046043 ) ) ;
#24129 = CARTESIAN_POINT ( 'NONE',  ( 98.23223304703363112, 124.2999999999999972, 1.767766952966351557 ) ) ;
#24130 = EDGE_CURVE ( 'NONE', #8914, #15622, #18959, .T. ) ;
#24131 = CARTESIAN_POINT ( 'NONE',  ( 120.7049497278729575, 40.45429687608393721, -9.295050272127046043 ) ) ;
#24132 = CARTESIAN_POINT ( 'NONE',  ( 104.9999999999999858, 91.87499999726880162, -6.938893903907228378E-15 ) ) ;
#24133 = CARTESIAN_POINT ( 'NONE',  ( 65.00000000000000000, 38.17226562608394147, -13.14518615778179544 ) ) ;
#24134 = CARTESIAN_POINT ( 'NONE',  ( 74.18017581364799184, 50.00000000000000000, -10.00000000000000000 ) ) ;
#24135 = CARTESIAN_POINT ( 'NONE',  ( 195.0000000000000000, 33.80664062608393294, 13.14518615778179544 ) ) ;
#24136 = ORIENTED_EDGE ( 'NONE', *, *, #15560, .T. ) ;
#24137 = CARTESIAN_POINT ( 'NONE',  ( -9.295050272127044266, 39.26367187608393294, 9.295050272127047819 ) ) ;
#24138 = DIRECTION ( 'NONE',  ( 0.000000000000000000, 1.000000000000000000, 0.000000000000000000 ) ) ;
#24139 = CARTESIAN_POINT ( 'NONE',  ( 95.54126587499996504, 1.387778780781445676E-14, 10.68750000136559208 ) ) ;
#24140 = CARTESIAN_POINT ( 'NONE',  ( 101.7677669529663547, 124.5000000000000000, 1.767766952966350891 ) ) ;
#24141 = ADVANCED_FACE ( 'NONE', ( #4052 ), #1498, .T. ) ;
#24142 = CARTESIAN_POINT ( 'NONE',  ( 104.4587341249999639, 79.93750000136559208, -1.442382525525748735E-14 ) ) ;
#24143 = CARTESIAN_POINT ( 'NONE',  ( 204.2950502721270425, 37.87460937608393152, -9.295050272127046043 ) ) ;
#24144 = AXIS2_PLACEMENT_3D ( 'NONE', #18919, #7949, #10074 ) ;
#24145 = CARTESIAN_POINT ( 'NONE',  ( 9.295050272127047819, 39.46210937608393721, 9.295050272127046043 ) ) ;
#24146 = CARTESIAN_POINT ( 'NONE',  ( 84.99999999999998579, 125.0000000000000000, -13.00000000000000888 ) ) ;
#24147 = DIRECTION ( 'NONE',  ( -0.000000000000000000, -1.000000000000000000, -0.000000000000000000 ) ) ;
#24148 = CARTESIAN_POINT ( 'NONE',  ( 112.9999999999999858, 118.0000000000000000, -43.00000000000000000 ) ) ;
#24149 = CARTESIAN_POINT ( 'NONE',  ( 104.9952793366501709, 116.8754121666685393, -54.32499999726881867 ) ) ;
#24150 = ORIENTED_EDGE ( 'NONE', *, *, #6510, .T. ) ;
#24151 = EDGE_CURVE ( 'NONE', #20470, #1287, #20049, .T. ) ;
#24152 = CARTESIAN_POINT ( 'NONE',  ( -13.57481594606304576, 37.82499999999999574, 0.000000000000000000 ) ) ;
#24153 = CARTESIAN_POINT ( 'NONE',  ( -8.049105076161786076E-16, 37.97382812608393721, -13.14518615778179544 ) ) ;
#24154 = VERTEX_POINT ( 'NONE', #27925 ) ;
#24155 = CARTESIAN_POINT ( 'NONE',  ( 135.4449143864723055, 36.53515625108393294, -13.14518615778179900 ) ) ;
#24156 = CARTESIAN_POINT ( 'NONE',  ( 59.55508561352770158, 33.26093750108393721, -13.14518615778179900 ) ) ;
#24157 = ADVANCED_FACE ( 'NONE', ( #17071 ), #16672, .T. ) ;
#24158 = CARTESIAN_POINT ( 'NONE',  ( 185.7049497278729575, 37.67617187608393436, 9.295050272127047819 ) ) ;
#24159 = ORIENTED_EDGE ( 'NONE', *, *, #19766, .F. ) ;
#24160 = CARTESIAN_POINT ( 'NONE',  ( 84.99999999999998579, 99.99999999999998579, -45.00000000000000711 ) ) ;
#24161 = CARTESIAN_POINT ( 'NONE',  ( 13.14518615778179900, 32.26875000108393721, -5.444914386472297529 ) ) ;
#24162 = CARTESIAN_POINT ( 'NONE',  ( 129.0169348148962172, 49.99999999949010743, -13.54930971656700756 ) ) ;
#24163 = PLANE ( 'NONE',  #5779 ) ;
#24164 = CARTESIAN_POINT ( 'NONE',  ( 116.4251840539369454, 39.46210937716787726, -5.622872871577873077 ) ) ;
#24165 = FACE_BOUND ( 'NONE', #15831, .T. ) ;
#24166 = ADVANCED_FACE ( 'NONE', ( #18942 ), #5848, .T. ) ;
#24167 = FACE_OUTER_BOUND ( 'NONE', #8494, .T. ) ;
#24168 = CARTESIAN_POINT ( 'NONE',  ( 101.7677669529663547, 123.2000000021849502, -1.767766952966370209 ) ) ;
#24169 = CARTESIAN_POINT ( 'NONE',  ( 97.50000000000000000, 124.2500000000000000, 1.035533905932725096 ) ) ;
#24170 = EDGE_LOOP ( 'NONE', ( #3762, #23936, #5792, #12496, #13807, #5387 ) ) ;
#24171 = VERTEX_POINT ( 'NONE', #12648 ) ;
#24172 = CARTESIAN_POINT ( 'NONE',  ( 103.1528011352953342, -3.152801135295355106, 9.812500001365593860 ) ) ;
#24173 = ORIENTED_EDGE ( 'NONE', *, *, #15657, .T. ) ;
#24174 = CARTESIAN_POINT ( 'NONE',  ( 99.14382582708707048, 124.4000000010924794, -2.066987299999999195 ) ) ;
#24175 = CARTESIAN_POINT ( 'NONE',  ( 104.4587341249999781, 1.846868145590750299, 11.00000000136559208 ) ) ;
#24176 = CARTESIAN_POINT ( 'NONE',  ( 132.5295839951739367, 49.99999999938366813, 13.34625891065843994 ) ) ;
#24177 = CARTESIAN_POINT ( 'NONE',  ( 9.295050272127046043, 37.87460937608393152, -9.295050272127046043 ) ) ;
#24178 = CARTESIAN_POINT ( 'NONE',  ( 96.84719886470459471, 79.81250000136559208, 3.152801135295355994 ) ) ;
#24179 = CARTESIAN_POINT ( 'NONE',  ( 70.44491438647230552, 33.85625000108393579, 13.14518615778179189 ) ) ;
#24180 = CARTESIAN_POINT ( 'NONE',  ( 93.46109445667491400, 114.7507929638356785, -53.32500000273119412 ) ) ;
#24181 = CARTESIAN_POINT ( 'NONE',  ( 13.14518615778179544, 38.56914062608393579, -1.609821015232357215E-15 ) ) ;
#24182 = DIRECTION ( 'NONE',  ( -0.000000000000000000, -1.000000000000000000, -0.000000000000000000 ) ) ;
#24183 = CARTESIAN_POINT ( 'NONE',  ( 130.0000000000000000, 36.43593749999999432, 13.57481594606304576 ) ) ;
#24184 = CARTESIAN_POINT ( 'NONE',  ( 95.67376207875069838, 104.0454443415356991, -56.19999999453762740 ) ) ;
#24185 = CARTESIAN_POINT ( 'NONE',  ( 139.5988444088204403, 38.32109374999999574, -9.598844408820458085 ) ) ;
#24186 = EDGE_CURVE ( 'NONE', #12537, #21429, #6048, .T. ) ;
#24187 = ORIENTED_EDGE ( 'NONE', *, *, #13831, .F. ) ;
#24188 = LINE ( 'NONE', #4667, #9921 ) ;
#24189 = CARTESIAN_POINT ( 'NONE',  ( 5.444914386472302859, 37.82500000108392868, 13.14518615778179189 ) ) ;
#24190 = CARTESIAN_POINT ( 'NONE',  ( 9.598844408820459861, 37.42812500216787441, 9.598844408820456309 ) ) ;
#24191 = CARTESIAN_POINT ( 'NONE',  ( 94.99999999999995737, 2.071067811865491048, 8.062500002731185944 ) ) ;
#24192 = CARTESIAN_POINT ( 'NONE',  ( 135.4449143864723055, 36.83281250108392868, 13.14518615778179189 ) ) ;
#24193 = CARTESIAN_POINT ( 'NONE',  ( 65.00000000000000000, 34.55078125216787299, -13.57481594606304576 ) ) ;
#24194 = ORIENTED_EDGE ( 'NONE', *, *, #3949, .T. ) ;
#24195 = CARTESIAN_POINT ( 'NONE',  ( 99.99999999999995737, 83.25000000000000000, 4.999999999999990230 ) ) ;
#24196 = CARTESIAN_POINT ( 'NONE',  ( -9.598844408820454532, 33.26093750216787726, 9.598844408820459861 ) ) ;
#24197 = CARTESIAN_POINT ( 'NONE',  ( 94.99999999999995737, -2.071067811865466624, 1.062499999999999334 ) ) ;
#24198 = CARTESIAN_POINT ( 'NONE',  ( 94.99999999999995737, 84.93750000000001421, -2.071067811865491493 ) ) ;
#24199 = CARTESIAN_POINT ( 'NONE',  ( 208.1451861577818079, 35.39414062608393152, -1.609821015232357215E-15 ) ) ;
#24200 = DIRECTION ( 'NONE',  ( -0.000000000000000000, 1.000000000000000000, -0.000000000000000000 ) ) ;
#24201 = CARTESIAN_POINT ( 'NONE',  ( 124.5550856135277087, 36.43593750108394147, -13.14518615778179722 ) ) ;
#24203 = ORIENTED_EDGE ( 'NONE', *, *, #19414, .F. ) ;
#24202 = CARTESIAN_POINT ( 'NONE',  ( 204.5988444088204687, 38.91640624999999432, 9.598844408820456309 ) ) ;
#24204 = CARTESIAN_POINT ( 'NONE',  ( 84.99999999999998579, 97.00000000000000000, 12.99999999999999467 ) ) ;
#24205 = CARTESIAN_POINT ( 'NONE',  ( -9.598844408820458085, 32.26875000216787726, -9.598844408820458085 ) ) ;
#24206 = CARTESIAN_POINT ( 'NONE',  ( -9.598844408820458085, 36.93203124999999432, -9.598844408820458085 ) ) ;
#24207 = CARTESIAN_POINT ( 'NONE',  ( 139.5988444088204687, 38.12265624999999858, 9.598844408820456309 ) ) ;
#24208 =( BOUNDED_CURVE ( )  B_SPLINE_CURVE ( 2, ( #25679, #12694, #10563, #8429, #17118, #8574, #26250, #23970, #24390, #6994, #22120, #19687, #24535, #13392, #5020, #26537, #2738, #21698, #31, #6710, #6852, #24249, #19830, #13246, #15252, #15541, #9140, #2599, #4449, #11260, #13103, #17405, #15397, #2173, #10835, #21842, #2454, #8713, #21978, #26397, #19980, #26105, #4732, #15688, #458, #11116, #13542, #17833, #4878, #22264, #11403, #6570, #315, #9002, #20122, #17694, #19550, #600, #24109, #9279, #17547, #2318, #17976, #26685, #10975, #174, #4586, #7132, #15829, #8856, #3015, #16405, #7713, #18267, #5302, #13685, #11831, #18408, #26832, #14253, #3302, #22402, #5159, #22691, #20259, #13966, #27115, #11972, #22974, #1036, #18550, #27254, #3161, #5588, #25102, #22546, #20695, #9418, #14112, #25236, #11684 ),
 .UNSPECIFIED., .F., .F. ) 
 B_SPLINE_CURVE_WITH_KNOTS ( ( 3, 2, 2, 2, 2, 2, 2, 2, 2, 2, 2, 2, 2, 2, 2, 2, 2, 2, 2, 2, 2, 2, 2, 2, 2, 2, 2, 2, 2, 2, 2, 2, 2, 2, 2, 2, 2, 2, 2, 2, 2, 2, 2, 2, 2, 2, 2, 2, 2, 2, 3 ),
 ( 0.000000000000000000, 0.02000000000000000042, 0.04000000000000000083, 0.05999999999999999778, 0.08000000000000000167, 0.1000000000000000056, 0.1199999999999999956, 0.1400000000000000133, 0.1600000000000000033, 0.1799999999999999933, 0.2000000000000000111, 0.2200000000000000011, 0.2399999999999999911, 0.2600000000000000089, 0.2800000000000000266, 0.2999999999999999889, 0.3200000000000000067, 0.3400000000000000244, 0.3599999999999999867, 0.3800000000000000044, 0.4000000000000000222, 0.4199999999999999845, 0.4400000000000000022, 0.4600000000000000200, 0.4799999999999999822, 0.5000000000000000000, 0.5200000000000000178, 0.5400000000000000355, 0.5600000000000000533, 0.5799999999999999600, 0.5999999999999999778, 0.6199999999999999956, 0.6400000000000000133, 0.6600000000000000311, 0.6800000000000000488, 0.6999999999999999556, 0.7199999999999999734, 0.7399999999999999911, 0.7600000000000000089, 0.7800000000000000266, 0.8000000000000000444, 0.8199999999999999512, 0.8399999999999999689, 0.8599999999999999867, 0.8800000000000000044, 0.9000000000000000222, 0.9200000000000000400, 0.9399999999999999467, 0.9599999999999999645, 0.9799999999999999822, 1.000000000000000000 ),
 .UNSPECIFIED. ) 
 CURVE ( )  GEOMETRIC_REPRESENTATION_ITEM ( )  RATIONAL_B_SPLINE_CURVE ( ( 1.000000000000000000, 0.9510565162951535312, 1.000000000000000000, 0.9510565162951535312, 1.000000000000000000, 0.9510565162951535312, 1.000000000000000000, 0.9510565162951535312, 1.000000000000000000, 0.9510565162951535312, 1.000000000000000000, 0.9510565162951535312, 1.000000000000000000, 0.9510565162951535312, 1.000000000000000000, 0.9510565162951535312, 1.000000000000000000, 0.9510565162951535312, 1.000000000000000000, 0.9510565162951535312, 1.000000000000000000, 0.9510565162951535312, 1.000000000000000000, 0.9510565162951535312, 1.000000000000000000, 0.9510565162951535312, 1.000000000000000000, 0.9510565162951535312, 1.000000000000000000, 0.9510565162951535312, 1.000000000000000000, 0.9510565162951535312, 1.000000000000000000, 0.9510565162951535312, 1.000000000000000000, 0.9510565162951535312, 1.000000000000000000, 0.9510565162951535312, 1.000000000000000000, 0.9510565162951535312, 1.000000000000000000, 0.9510565162951535312, 1.000000000000000000, 0.9510565162951535312, 1.000000000000000000, 0.9510565162951535312, 1.000000000000000000, 0.9510565162951535312, 1.000000000000000000, 0.9510565162951535312, 1.000000000000000000, 0.9510565162951535312, 1.000000000000000000, 0.9510565162951535312, 1.000000000000000000, 0.9510565162951535312, 1.000000000000000000, 0.9510565162951535312, 1.000000000000000000, 0.9510565162951535312, 1.000000000000000000, 0.9510565162951535312, 1.000000000000000000, 0.9510565162951535312, 1.000000000000000000, 0.9510565162951535312, 1.000000000000000000, 0.9510565162951535312, 1.000000000000000000, 0.9510565162951535312, 1.000000000000000000, 0.9510565162951535312, 1.000000000000000000, 0.9510565162951535312, 1.000000000000000000, 0.9510565162951535312, 1.000000000000000000, 0.9510565162951535312, 1.000000000000000000, 0.9510565162951535312, 1.000000000000000000, 0.9510565162951535312, 1.000000000000000000, 0.9510565162951535312, 1.000000000000000000, 0.9510565162951535312, 1.000000000000000000, 0.9510565162951535312, 1.000000000000000000, 0.9510565162951535312, 1.000000000000000000, 0.9510565162951535312, 1.000000000000000000, 0.9510565162951535312, 1.000000000000000000, 0.9510565162951535312, 1.000000000000000000, 0.9510565162951535312, 1.000000000000000000, 0.9510565162951535312, 1.000000000000000000 ) ) 
 REPRESENTATION_ITEM ( '' )  );
#24209 = CARTESIAN_POINT ( 'NONE',  ( -5.444914386472299306, 37.72578125108395142, 13.14518615778179722 ) ) ;
#24210 = CARTESIAN_POINT ( 'NONE',  ( 5.444914386472297529, 37.13046875108393152, -13.14518615778179900 ) ) ;
#24211 = CARTESIAN_POINT ( 'NONE',  ( 185.4011555911795313, 34.55078124999999289, -9.598844408820458085 ) ) ;
#24212 = CARTESIAN_POINT ( 'NONE',  ( 108.0825317500000011, 107.3738262389971680, -44.47500000273118559 ) ) ;
#24213 = FACE_OUTER_BOUND ( 'NONE', #23268, .T. ) ;
#24214 = CARTESIAN_POINT ( 'NONE',  ( 78.14518615778179367, 36.93203125108394147, 5.444914386472293977 ) ) ;
#24215 = CARTESIAN_POINT ( 'NONE',  ( 104.4587341249999781, 1.846868145590750521, 1.000000001365592528 ) ) ;
#24216 = CARTESIAN_POINT ( 'NONE',  ( 100.5280963304672923, 123.0000000000000000, 2.448276570249286799 ) ) ;
#24217 = ORIENTED_EDGE ( 'NONE', *, *, #10126, .F. ) ;
#24218 = CARTESIAN_POINT ( 'NONE',  ( 101.0355339059327235, 123.9500000000000028, -2.499999999999996447 ) ) ;
#24219 = CARTESIAN_POINT ( 'NONE',  ( 9.598844408820459861, 34.94765624999999432, 9.598844408820456309 ) ) ;
#24220 = CARTESIAN_POINT ( 'NONE',  ( 116.8548138422182063, 36.83281250108393579, 5.444914386472304635 ) ) ;
#24221 = ORIENTED_EDGE ( 'NONE', *, *, #294, .T. ) ;
#24222 = CARTESIAN_POINT ( 'NONE',  ( 94.99999999999995737, 83.00000000000000000, -1.387778780781445676E-14 ) ) ;
#24223 = CARTESIAN_POINT ( 'NONE',  ( 97.92893218813451028, 82.93750000273119838, -5.000000000000018652 ) ) ;
#24224 = CARTESIAN_POINT ( 'NONE',  ( 95.54126587499999346, 93.74999999863439371, -1.846868145590737864 ) ) ;
#24225 = CARTESIAN_POINT ( 'NONE',  ( 104.4587341249999923, 95.49999999863442213, 1.846868145590726318 ) ) ;
#24226 = CARTESIAN_POINT ( 'NONE',  ( 95.67376207875069838, 104.0454443415356991, -48.70000000000000995 ) ) ;
#24227 = CARTESIAN_POINT ( 'NONE',  ( 78.57481594606304043, 39.85898437499999858, -5.622872871577873077 ) ) ;
#24228 = ORIENTED_EDGE ( 'NONE', *, *, #15195, .F. ) ;
#24229 = DIRECTION ( 'NONE',  ( -5.782411586589357392E-17, -1.156482317317871478E-16, -1.000000000000000000 ) ) ;
#24230 = CARTESIAN_POINT ( 'NONE',  ( 99.99999999999995737, 5.000000000000018652, 11.75000000000000000 ) ) ;
#24231 = ORIENTED_EDGE ( 'NONE', *, *, #116, .T. ) ;
#24232 = CARTESIAN_POINT ( 'NONE',  ( 5.444914386472297529, 32.56640625108394005, -13.14518615778179722 ) ) ;
#24233 = CARTESIAN_POINT ( 'NONE',  ( 5.444914386472297529, 38.91640625108393436, -13.14518615778179900 ) ) ;
#24234 = CARTESIAN_POINT ( 'NONE',  ( 181.4251840539369596, 35.49335937716787015, -5.622872871577873077 ) ) ;
#24235 = CARTESIAN_POINT ( 'NONE',  ( -5.444914386472299306, 35.93984375108392726, 13.14518615778179722 ) ) ;
#24236 = CARTESIAN_POINT ( 'NONE',  ( 130.0000000000000000, -7.395377635281828788, -11.57481594606305997 ) ) ;
#24237 = CARTESIAN_POINT ( 'NONE',  ( 130.0000000000000000, 36.58476562608393579, -13.14518615778179544 ) ) ;
#24238 = CARTESIAN_POINT ( 'NONE',  ( -9.295050272127044266, 34.50117187608393721, 9.295050272127047819 ) ) ;
#24239 = EDGE_CURVE ( 'NONE', #19624, #19393, #6254, .T. ) ;
#24240 = CARTESIAN_POINT ( 'NONE',  ( 130.0000000000000000, 34.00507812608393721, -13.14518615778179544 ) ) ;
#24241 = CARTESIAN_POINT ( 'NONE',  ( 78.57481594606305464, 35.84062499999999574, -1.662435489736055892E-15 ) ) ;
#24242 = CARTESIAN_POINT ( 'NONE',  ( -5.622872871577964560, 34.50117187499998295, -13.57481594606295339 ) ) ;
#24243 = CARTESIAN_POINT ( 'NONE',  ( 101.8468681455906903, -4.458734124999987891, 10.00000000136559386 ) ) ;
#24244 = CARTESIAN_POINT ( 'NONE',  ( 207.3201169669888770, 36.00000000000001421, -5.704949255836485378 ) ) ;
#24245 = CARTESIAN_POINT ( 'NONE',  ( 99.99999999999995737, -4.458734124999988779, 0.6875000013655923059 ) ) ;
#24246 = CARTESIAN_POINT ( 'NONE',  ( 102.1631189606246295, 116.6573956140660897, -53.10000000546238397 ) ) ;
#24247 = FACE_OUTER_BOUND ( 'NONE', #20870, .T. ) ;
#24248 = DIRECTION ( 'NONE',  ( -0.8660254037844418162, -0.000000000000000000, -0.4999999999999947264 ) ) ;
#24249 = CARTESIAN_POINT ( 'NONE',  ( 91.91746824999997045, 112.6261737610028320, -47.72499999726881725 ) ) ;
#24250 = CARTESIAN_POINT ( 'NONE',  ( 13.14518615778179544, 36.38632812608393863, -1.609821015232357215E-15 ) ) ;
#24251 = AXIS2_PLACEMENT_3D ( 'NONE', #21799, #22081, #2278 ) ;
#24252 = CARTESIAN_POINT ( 'NONE',  ( 104.9952793366501709, 116.8754121666685393, -54.57499999726882578 ) ) ;
#24253 = EDGE_LOOP ( 'NONE', ( #15620, #23715 ) ) ;
#24254 = CARTESIAN_POINT ( 'NONE',  ( 98.53841926354351699, 123.0500000010924850, -1.461580736456474794 ) ) ;
#24255 =( BOUNDED_CURVE ( )  B_SPLINE_CURVE ( 2, ( #27622, #5818, #3680, #18912, #8080, #16775, #10485, #4653, #22180 ),
 .UNSPECIFIED., .F., .T. ) 
 B_SPLINE_CURVE_WITH_KNOTS ( ( 3, 2, 2, 2, 3 ),
 ( 0.4285714285714285476, 0.4375000000000000000, 0.4464285714285713969, 0.4553571428571427937, 0.4642857142857142461 ),
 .UNSPECIFIED. ) 
 CURVE ( )  GEOMETRIC_REPRESENTATION_ITEM ( )  RATIONAL_B_SPLINE_CURVE ( ( 1.000000000000000000, 0.9238795325112867385, 1.000000000000000000, 0.9238795325112867385, 1.000000000000000000, 0.9238795325112867385, 1.000000000000000000, 0.9238795325112871826, 0.9999999999999995559 ) ) 
 REPRESENTATION_ITEM ( '' )  );
#24256 = CARTESIAN_POINT ( 'NONE',  ( 97.93301270000000613, 122.9500000010924765, -9.540979117872439019E-15 ) ) ;
#24257 = CARTESIAN_POINT ( 'NONE',  ( 84.99999999999998579, 125.0000000000000000, -15.00000000000000888 ) ) ;
#24258 = CARTESIAN_POINT ( 'NONE',  ( 189.5550856135277229, 35.64218750108392442, -13.14518615778179900 ) ) ;
#24259 = VERTEX_POINT ( 'NONE', #14927 ) ;
#24260 = CARTESIAN_POINT ( 'NONE',  ( 99.99999999999998579, 90.00000000000000000, 4.999999999999983125 ) ) ;
#24261 = CARTESIAN_POINT ( 'NONE',  ( 104.3262379212492448, 115.9545556584642867, -49.19999999453763451 ) ) ;
#24262 = DIRECTION ( 'NONE',  ( 0.000000000000000000, 0.000000000000000000, -1.000000000000000000 ) ) ;
#24263 = ORIENTED_EDGE ( 'NONE', *, *, #16134, .F. ) ;
#24264 = CARTESIAN_POINT ( 'NONE',  ( 107.0000000000000142, 107.7255621263696526, -47.10000000000000853 ) ) ;
#24265 = CARTESIAN_POINT ( 'NONE',  ( 13.14518615778179900, 39.31328125108392868, 5.444914386472293977 ) ) ;
#24266 = CARTESIAN_POINT ( 'NONE',  ( 99.99999999999998579, 124.3999999999999915, 2.499999999999978684 ) ) ;
#24267 = CARTESIAN_POINT ( 'NONE',  ( 133.8783854107797424, 31.34156310770110565, -13.57481594606304931 ) ) ;
#24268 = FACE_OUTER_BOUND ( 'NONE', #24563, .T. ) ;
#24269 =( REPRESENTATION_RELATIONSHIP ('NONE','NONE', #2411, #19878 ) REPRESENTATION_RELATIONSHIP_WITH_TRANSFORMATION ( #10379 )SHAPE_REPRESENTATION_RELATIONSHIP( ) );
#24270 = CARTESIAN_POINT ( 'NONE',  ( 103.5355339059327235, 92.99999999726881583, -3.535533905932738197 ) ) ;
#24271 = CARTESIAN_POINT ( 'NONE',  ( 78.14518615778179367, 38.71796875108393721, 5.444914386472293977 ) ) ;
#24272 = EDGE_CURVE ( 'NONE', #13933, #6189, #6479, .T. ) ;
#24273 = CARTESIAN_POINT ( 'NONE',  ( 57.91058272766510839, 49.99999999943660356, -11.59823041028830026 ) ) ;
#24274 = CARTESIAN_POINT ( 'NONE',  ( 208.5748159460630120, 39.75976562499999289, 5.622872871577869525 ) ) ;
#24275 = EDGE_CURVE ( 'NONE', #2287, #19200, #25226, .T. ) ;
#24276 = CARTESIAN_POINT ( 'NONE',  ( 78.39333672780520601, 36.00000000000000000, -2.034633736483404398 ) ) ;
#24277 = VERTEX_POINT ( 'NONE', #19782 ) ;
#24278 = CARTESIAN_POINT ( 'NONE',  ( -9.295050272127046043, 37.47773437608393010, -9.295050272127046043 ) ) ;
#24279 = CARTESIAN_POINT ( 'NONE',  ( 98.15313185440923860, 4.458734125000016313, 12.50000000136559208 ) ) ;
#24280 = CARTESIAN_POINT ( 'NONE',  ( 65.00000000000000000, 36.78320312608393294, 13.14518615778179544 ) ) ;
#24281 = CARTESIAN_POINT ( 'NONE',  ( 104.9999999999999858, 90.87499999726880162, -6.938893903907228378E-15 ) ) ;
#24282 = CARTESIAN_POINT ( 'NONE',  ( 200.4449143864723055, 40.30546875108393579, -13.14518615778179722 ) ) ;
#24283 = CARTESIAN_POINT ( 'NONE',  ( -5.444914386472297529, 37.42812500108394147, -13.14518615778179722 ) ) ;
#24284 = CARTESIAN_POINT ( 'NONE',  ( 5.622872871577786924, 34.10429687500000284, 13.57481594606313813 ) ) ;
#24285 = CARTESIAN_POINT ( 'NONE',  ( 208.1451861577818079, 39.61093750108393863, -5.444914386472297529 ) ) ;
#24286 = CARTESIAN_POINT ( 'NONE',  ( 108.0825317499999869, 107.3738262389971538, -54.72499999726881015 ) ) ;
#24287 = EDGE_CURVE ( 'NONE', #27029, #18432, #25605, .T. ) ;
#24288 = ORIENTED_EDGE ( 'NONE', *, *, #16134, .T. ) ;
#24289 = VECTOR ( 'NONE', #692, 1000.000000000000000 ) ;
#24290 = CARTESIAN_POINT ( 'NONE',  ( 5.622872871577871301, 35.19570312499999432, -13.57481594606304753 ) ) ;
#24291 = CARTESIAN_POINT ( 'NONE',  ( 5.444914386472302859, 37.62656250108393863, 13.14518615778179189 ) ) ;
#24292 = VERTEX_POINT ( 'NONE', #6948 ) ;
#24293 = CARTESIAN_POINT ( 'NONE',  ( 120.7049497278729575, 33.50898437608393010, -9.295050272127046043 ) ) ;
#24294 = CARTESIAN_POINT ( 'NONE',  ( 51.85481384221820633, 33.40976562608393863, 0.000000000000000000 ) ) ;
#24295 = CARTESIAN_POINT ( 'NONE',  ( 208.1451861577817795, 38.81718750108393579, -5.444914386472297529 ) ) ;
#24296 = ORIENTED_EDGE ( 'NONE', *, *, #5776, .T. ) ;
#24297 = CARTESIAN_POINT ( 'NONE',  ( 94.99999999999994316, 2.071067811865481278, 11.06250000273118594 ) ) ;
#24298 = PRESENTATION_STYLE_ASSIGNMENT (( #10888 ) ) ;
#24299 = LINE ( 'NONE', #22312, #1770 ) ;
#24300 = CARTESIAN_POINT ( 'NONE',  ( -8.312177448680279460E-16, 36.03906250000000000, -13.57481594606304576 ) ) ;
#24301 = LINE ( 'NONE', #9055, #6707 ) ;
#24302 = DIRECTION ( 'NONE',  ( 0.000000000000000000, -0.000000000000000000, 1.000000000000000000 ) ) ;
#24303 = EDGE_CURVE ( 'NONE', #7323, #9015, #16213, .T. ) ;
#24304 = CARTESIAN_POINT ( 'NONE',  ( 181.8548138422182205, 39.95820312608393010, 0.000000000000000000 ) ) ;
#24305 = CARTESIAN_POINT ( 'NONE',  ( 104.4587341249999781, -1.846868145590721655, 5.875000001365591196 ) ) ;
#24306 = ORIENTED_EDGE ( 'NONE', *, *, #8782, .T. ) ;
#24307 = CARTESIAN_POINT ( 'NONE',  ( 99.14382582708707048, 123.1000000010924822, 2.066987299999979211 ) ) ;
#24308 = CARTESIAN_POINT ( 'NONE',  ( 104.4587341249999781, 1.846868145590750299, 7.000000001365591196 ) ) ;
#24309 = CARTESIAN_POINT ( 'NONE',  ( 121.7886859848334353, 50.68678854790648103, 15.00000000000135003 ) ) ;
#24310 = EDGE_CURVE ( 'NONE', #27857, #11809, #7300, .T. ) ;
#24311 = CARTESIAN_POINT ( 'NONE',  ( 13.14518615778179900, 36.23750000108393010, -5.444914386472297529 ) ) ;
#24312 = CARTESIAN_POINT ( 'NONE',  ( 99.99999999999995737, 5.000000000000018652, 6.875000002731185056 ) ) ;
#24313 = CARTESIAN_POINT ( 'NONE',  ( 104.4587341249999639, 83.18750000136560629, -1.442382525525748735E-14 ) ) ;
#24314 = CARTESIAN_POINT ( 'NONE',  ( 70.44491438647230552, 36.23750000108393721, 13.14518615778179189 ) ) ;
#24315 = CARTESIAN_POINT ( 'NONE',  ( 91.91746824999999887, 110.0000000000000000, -45.12500000273119838 ) ) ;
#24316 = CARTESIAN_POINT ( 'NONE',  ( -5.444914386472299306, 38.32109375108394289, 13.14518615778179722 ) ) ;
#24317 = AXIS2_PLACEMENT_3D ( 'NONE', #20264, #750, #11689 ) ;
#24318 = CARTESIAN_POINT ( 'NONE',  ( 104.9999999999999716, 80.62500000273119838, -1.449011120738813565E-14 ) ) ;
#24319 = CARTESIAN_POINT ( 'NONE',  ( 107.0000000000000000, 110.0000000000000000, -145.0000000000000284 ) ) ;
#24320 = CARTESIAN_POINT ( 'NONE',  ( 99.99999999999997158, 102.6397644303321215, -55.99999999453763877 ) ) ;
#24321 = CARTESIAN_POINT ( 'NONE',  ( 116.4251840539369596, 37.08085937499999574, 5.622872871577880183 ) ) ;
#24322 = ORIENTED_EDGE ( 'NONE', *, *, #15599, .F. ) ;
#24323 = EDGE_CURVE ( 'NONE', #4141, #26410, #18440, .T. ) ;
#24324 = ORIENTED_EDGE ( 'NONE', *, *, #19777, .T. ) ;
#24325 = CARTESIAN_POINT ( 'NONE',  ( 13.57481594606304931, 33.40976562499999858, 5.622872871577868636 ) ) ;
#24326 = CARTESIAN_POINT ( 'NONE',  ( -5.444914386472299306, 36.13828125108393863, 13.14518615778179722 ) ) ;
#24327 = CARTESIAN_POINT ( 'NONE',  ( 9.598844408820456309, 37.62656250216787157, -9.598844408820458085 ) ) ;
#24328 = CARTESIAN_POINT ( 'NONE',  ( 103.5355339059327093, -3.535533905932726206, 11.50000000273118417 ) ) ;
#24329 = CARTESIAN_POINT ( 'NONE',  ( 120.7049497278729575, 32.51679687608393721, -9.295050272127046043 ) ) ;
#24330 = CARTESIAN_POINT ( 'NONE',  ( 78.57481594606305464, 35.14609375216787157, -1.662435489736055892E-15 ) ) ;
#24331 = ORIENTED_EDGE ( 'NONE', *, *, #18185, .T. ) ;
#24332 = CARTESIAN_POINT ( 'NONE',  ( 195.0000000000000000, 37.62656249999999858, -13.57481594606304576 ) ) ;
#24333 = CARTESIAN_POINT ( 'NONE',  ( -13.57481594606304753, 32.31835937716786589, -5.622872871577873077 ) ) ;
#24334 = CARTESIAN_POINT ( 'NONE',  ( 99.99999999999995737, -4.999999999999990230, 3.249999999999999556 ) ) ;
#24335 = CARTESIAN_POINT ( 'NONE',  ( 93.46109445667489979, 114.7507929638356785, -50.07499999726882578 ) ) ;
#24336 = AXIS2_PLACEMENT_3D ( 'NONE', #3662, #1252, #14468 ) ;
#24337 = CARTESIAN_POINT ( 'NONE',  ( 5.622872871577878406, 38.17226562716786731, 13.57481594606304576 ) ) ;
#24338 = CARTESIAN_POINT ( 'NONE',  ( 185.7049497278729575, 33.31054687608393294, -9.295050272127046043 ) ) ;
#24339 = CARTESIAN_POINT ( 'NONE',  ( 104.9999999999999716, 2.071067811865491937, 5.687500002731185056 ) ) ;
#24340 = CARTESIAN_POINT ( 'NONE',  ( 193.3974668693900298, 53.60343507248207118, 14.99999999999995026 ) ) ;
#24341 = DIRECTION ( 'NONE',  ( -0.000000000000000000, 1.000000000000000000, -0.000000000000000000 ) ) ;
#24342 = CARTESIAN_POINT ( 'NONE',  ( 9.598844408820459861, 37.32890624999999574, 9.598844408820456309 ) ) ;
#24343 = DIRECTION ( 'NONE',  ( -1.000000000000000000, 0.000000000000000000, 7.228014483236696740E-18 ) ) ;
#24344 = CARTESIAN_POINT ( 'NONE',  ( -5.444914386472299306, 33.75703125108393721, 13.14518615778179722 ) ) ;
#24345 = CARTESIAN_POINT ( 'NONE',  ( -9.295050272127046043, 36.48554687608393721, -9.295050272127046043 ) ) ;
#24346 = CARTESIAN_POINT ( 'NONE',  ( 195.0000000000000000, 34.05468749999999289, 13.57481594606304576 ) ) ;
#24347 = EDGE_CURVE ( 'NONE', #27535, #21141, #1656, .T. ) ;
#24348 = CARTESIAN_POINT ( 'NONE',  ( 91.91746824999999887, 110.0000000000000000, -45.37500000273119838 ) ) ;
#24349 = FACE_OUTER_BOUND ( 'NONE', #14753, .T. ) ;
#24350 = CARTESIAN_POINT ( 'NONE',  ( 70.44491438647230552, 34.74921875108394431, -13.14518615778179900 ) ) ;
#24351 = CARTESIAN_POINT ( 'NONE',  ( 98.15313185440923860, 4.458734125000016313, 1.250000001365592750 ) ) ;
#24352 = CARTESIAN_POINT ( 'NONE',  ( 102.5000695353236324, 123.0000000000000426, -0.2897305190755338211 ) ) ;
#24353 = ORIENTED_EDGE ( 'NONE', *, *, #19598, .F. ) ;
#24354 = CARTESIAN_POINT ( 'NONE',  ( 96.46446609406721961, 3.535533905932755072, 4.874999999999999112 ) ) ;
#24355 = CARTESIAN_POINT ( 'NONE',  ( 5.622872871577871301, 36.78320312499999289, -13.57481594606304753 ) ) ;
#24356 = CARTESIAN_POINT ( 'NONE',  ( 116.8548138422182205, 38.37070312608393152, 0.000000000000000000 ) ) ;
#24357 = ORIENTED_EDGE ( 'NONE', *, *, #2356, .F. ) ;
#24358 = CARTESIAN_POINT ( 'NONE',  ( 96.46446609406721961, 81.87500000000000000, -3.535533905932755072 ) ) ;
#24359 = AXIS2_PLACEMENT_3D ( 'NONE', #16936, #25429, #1715 ) ;
#24360 = CARTESIAN_POINT ( 'NONE',  ( 5.622872871577961895, 35.19570312499999432, -13.57481594606295339 ) ) ;
#24361 = CARTESIAN_POINT ( 'NONE',  ( 103.5355339059327093, 80.50000000273119838, 3.535533905932726206 ) ) ;
#24362 = CARTESIAN_POINT ( 'NONE',  ( 95.54126587499999346, 92.87499999863440792, 1.846868145590722543 ) ) ;
#24363 = CARTESIAN_POINT ( 'NONE',  ( 103.1528011352953484, 94.43749999863440792, 3.152801135295352886 ) ) ;
#24364 = CARTESIAN_POINT ( 'NONE',  ( 99.99999999999997158, 117.3602355696678501, -49.50000000000002132 ) ) ;
#24365 = CARTESIAN_POINT ( 'NONE',  ( 74.29505027212704249, 32.31835937608393294, 9.295050272127046043 ) ) ;
#24366 = VECTOR ( 'NONE', #15706, 1000.000000000000000 ) ;
#24367 = ORIENTED_EDGE ( 'NONE', *, *, #26815, .T. ) ;
#24368 = CARTESIAN_POINT ( 'NONE',  ( 99.99999999999998579, 138.0000000000000000, 11.50000000000001243 ) ) ;
#24369 = CARTESIAN_POINT ( 'NONE',  ( 94.99999999999995737, 2.071067811865491048, 11.93750000000000000 ) ) ;
#24370 = ORIENTED_EDGE ( 'NONE', *, *, #15750, .T. ) ;
#24371 = CARTESIAN_POINT ( 'NONE',  ( -9.295050272127044266, 35.29492187608393294, 9.295050272127047819 ) ) ;
#24372 = CARTESIAN_POINT ( 'NONE',  ( 181.4251840539369596, 33.21132812716787441, 5.622872871577880183 ) ) ;
#24373 =( BOUNDED_SURFACE ( )  B_SPLINE_SURFACE ( 1, 2, ( 
 ( #7528, #1275, #26793, #7674, #13788, #20517, #2839, #11650, #858, #20795, #17940, #24924, #20226, #20657, #13930, #25067, #18080, #1142, #20373, #5410, #14078, #3400, #26650, #12070, #7239, #7098, #24648, #15796, #5121, #15931, #22509, #14495, #5827, #1830, #17049, #8364, #16510, #21483, #14764, #10210, #25203 ),
 ( #10494, #25753, #18787, #8088, #1557, #3820, #27494, #12765, #18655, #21207, #21350, #5689, #12624, #10349, #19201, #18920, #1692, #23072, #10075, #12480, #16783, #27629, #3548, #23347, #25614, #19058, #20932, #27766, #1417, #14356, #3687, #9940, #27359, #7950, #25482, #12205, #5960, #14628, #8224, #27903, #16914 ) ),
 .UNSPECIFIED., .F., .F., .F. ) 
 B_SPLINE_SURFACE_WITH_KNOTS ( ( 2, 2 ),
 ( 3, 2, 2, 2, 2, 2, 2, 2, 2, 2, 2, 2, 2, 2, 2, 2, 2, 2, 2, 2, 3 ),
 ( 0.000000000000000000, 1.000000000000000000 ),
 ( 0.000000000000000000, 0.04166666666666666435, 0.08333333333333332871, 0.1250000000000000000, 0.1666666666666666574, 0.2083333333333333426, 0.2500000000000000000, 0.2916666666666666852, 0.3333333333333333148, 0.3750000000000000000, 0.4166666666666666852, 0.4583333333333333148, 0.5000000000000000000, 0.5416666666666666297, 0.5833333333333333703, 0.6250000000000000000, 0.6666666666666666297, 0.7083333333333333703, 0.7500000000000000000, 0.7916666666666666297, 0.8333333333333333703 ),
 .UNSPECIFIED. ) 
 GEOMETRIC_REPRESENTATION_ITEM ( )  RATIONAL_B_SPLINE_SURFACE ( (
 ( 1.000000000000000000, 0.9238795325112867385, 1.000000000000000000, 0.9238795325112867385, 1.000000000000000000, 0.9238795325112867385, 1.000000000000000000, 0.9238795325112867385, 1.000000000000000000, 0.9238795325112867385, 1.000000000000000000, 0.9238795325112867385, 1.000000000000000000, 0.9238795325112867385, 1.000000000000000000, 0.9238795325112867385, 1.000000000000000000, 0.9238795325112867385, 1.000000000000000000, 0.9238795325112867385, 1.000000000000000000, 0.9238795325112867385, 1.000000000000000000, 0.9238795325112867385, 1.000000000000000000, 0.9238795325112867385, 1.000000000000000000, 0.9238795325112867385, 1.000000000000000000, 0.9238795325112867385, 1.000000000000000000, 0.9238795325112867385, 1.000000000000000000, 0.9238795325112867385, 1.000000000000000000, 0.9238795325112867385, 1.000000000000000000, 0.9238795325112867385, 1.000000000000000000, 0.9238795325112867385, 1.000000000000000000),
 ( 1.000000000000000000, 0.9238795325112867385, 1.000000000000000000, 0.9238795325112867385, 1.000000000000000000, 0.9238795325112867385, 1.000000000000000000, 0.9238795325112867385, 1.000000000000000000, 0.9238795325112867385, 1.000000000000000000, 0.9238795325112867385, 1.000000000000000000, 0.9238795325112867385, 1.000000000000000000, 0.9238795325112867385, 1.000000000000000000, 0.9238795325112867385, 1.000000000000000000, 0.9238795325112867385, 1.000000000000000000, 0.9238795325112867385, 1.000000000000000000, 0.9238795325112867385, 1.000000000000000000, 0.9238795325112867385, 1.000000000000000000, 0.9238795325112867385, 1.000000000000000000, 0.9238795325112867385, 1.000000000000000000, 0.9238795325112867385, 1.000000000000000000, 0.9238795325112867385, 1.000000000000000000, 0.9238795325112867385, 1.000000000000000000, 0.9238795325112867385, 1.000000000000000000, 0.9238795325112867385, 1.000000000000000000) ) ) 
 REPRESENTATION_ITEM ( '' )  SURFACE ( )  );
#24374 = CARTESIAN_POINT ( 'NONE',  ( 13.14518615778179722, 34.55078125108393294, 5.444914386472293977 ) ) ;
#24375 = CARTESIAN_POINT ( 'NONE',  ( -5.622872871577965448, 32.41757812499999858, 13.57481594606295161 ) ) ;
#24376 = CARTESIAN_POINT ( 'NONE',  ( 200.6228728715779823, 40.05742187716787583, -13.57481594606294095 ) ) ;
#24377 = ORIENTED_EDGE ( 'NONE', *, *, #4744, .T. ) ;
#24378 = CARTESIAN_POINT ( 'NONE',  ( 9.295050272127046043, 35.69179687608394147, -9.295050272127046043 ) ) ;
#24379 = VECTOR ( 'NONE', #6191, 1000.000000000000114 ) ;
#24380 = CARTESIAN_POINT ( 'NONE',  ( 133.7556382656599112, 31.58960998161716560, -13.14518615778179900 ) ) ;
#24381 = CARTESIAN_POINT ( 'NONE',  ( 55.40115559117954547, 34.55078124999999289, -9.598844408820458085 ) ) ;
#24382 = CYLINDRICAL_SURFACE ( 'NONE', #10472, 13.57481594606304398 ) ;
#24383 = CARTESIAN_POINT ( 'NONE',  ( 96.84719886470459471, 3.152801135295383084, 9.562500001365593860 ) ) ;
#24384 = CARTESIAN_POINT ( 'NONE',  ( 208.3933367278050923, 36.00000000000000000, -2.034633736484581679 ) ) ;
#24385 = CARTESIAN_POINT ( 'NONE',  ( 104.4587341249999781, 1.846868145590750299, 1.000000001365592528 ) ) ;
#24386 = CARTESIAN_POINT ( 'NONE',  ( 99.99999999999998579, 101.5015231886685854, -44.62500000273119838 ) ) ;
#24387 = DIRECTION ( 'NONE',  ( 0.000000000000000000, -1.000000000000000000, 0.000000000000000000 ) ) ;
#24388 = AXIS2_PLACEMENT_3D ( 'NONE', #1590, #20968, #3437 ) ;
#24389 = LINE ( 'NONE', #15967, #25283 ) ;
#24390 = CARTESIAN_POINT ( 'NONE',  ( 106.5389055433250860, 114.7507929638356785, -46.42499999726882720 ) ) ;
#24391 = CARTESIAN_POINT ( 'NONE',  ( 5.444914386472297529, 34.94765625108394147, -13.14518615778179900 ) ) ;
#24392 = CARTESIAN_POINT ( 'NONE',  ( 91.91746824999997045, 112.6261737610028320, -51.97499999726882436 ) ) ;
#24393 = ORIENTED_EDGE ( 'NONE', *, *, #22564, .T. ) ;
#24394 = CARTESIAN_POINT ( 'NONE',  ( 97.93301270000000613, 123.1500000010924651, -9.540979117872439019E-15 ) ) ;
#24395 = CYLINDRICAL_SURFACE ( 'NONE', #25732, 13.57481594606304576 ) ;
#24396 = CARTESIAN_POINT ( 'NONE',  ( 99.99999999999995737, 85.00000000000000000, -1.387778780781445676E-14 ) ) ;
#24397 = EDGE_CURVE ( 'NONE', #18157, #17002, #19127, .T. ) ;
#24398 = CARTESIAN_POINT ( 'NONE',  ( 208.1451861577818079, 34.60039062608392868, -1.609821015232357215E-15 ) ) ;
#24399 = ORIENTED_EDGE ( 'NONE', *, *, #5130, .F. ) ;
#24400 = CARTESIAN_POINT ( 'NONE',  ( 13.57481594606304931, 39.85898437716787157, 5.622872871577868636 ) ) ;
#24401 = CARTESIAN_POINT ( 'NONE',  ( 103.1528011352953342, -3.152801135295355106, 10.06250000136559386 ) ) ;
#24402 = ORIENTED_EDGE ( 'NONE', *, *, #26943, .F. ) ;
#24403 = CARTESIAN_POINT ( 'NONE',  ( 105.6631189606246295, 105.8855032339526758, -45.20000000000000284 ) ) ;
#24404 = CARTESIAN_POINT ( 'NONE',  ( -13.14518615778179544, 35.79101562608393294, 0.000000000000000000 ) ) ;
#24405 = VECTOR ( 'NONE', #19306, 1000.000000000000000 ) ;
#24406 = CARTESIAN_POINT ( 'NONE',  ( 102.4999999999999716, 124.6500000000000199, -1.035533905932742638 ) ) ;
#24407 = CARTESIAN_POINT ( 'NONE',  ( 120.4011555911795455, 31.47500000216787441, -9.598844408820458085 ) ) ;
#24408 = CARTESIAN_POINT ( 'NONE',  ( 94.99999999999995737, 1.387778780781445676E-14, 34.79898987322334136 ) ) ;
#24409 = CARTESIAN_POINT ( 'NONE',  ( 99.99999999999998579, 93.12499999726881583, -4.999999999999997335 ) ) ;
#24410 = CARTESIAN_POINT ( 'NONE',  ( 74.29505027212704249, 38.66835937608393436, 9.295050272127046043 ) ) ;
#24411 = CARTESIAN_POINT ( 'NONE',  ( 56.79855381236158252, 50.69246985422713436, -14.99999999999860201 ) ) ;
#24412 = CARTESIAN_POINT ( 'NONE',  ( 93.46109445667491400, 114.7507929638356785, -49.57500000273120122 ) ) ;
#24413 = CARTESIAN_POINT ( 'NONE',  ( 195.0000000000000000, 40.00781250000000000, -13.57481594606304576 ) ) ;
#24414 = CARTESIAN_POINT ( 'NONE',  ( 99.99999999999998579, 110.0000000000000000, -145.0000000000000284 ) ) ;
#24415 =( BOUNDED_CURVE ( )  B_SPLINE_CURVE ( 2, ( #3648, #1379, #22897, #5651, #12168, #16608, #25580, #1793, #14456 ),
 .UNSPECIFIED., .F., .F. ) 
 B_SPLINE_CURVE_WITH_KNOTS ( ( 3, 2, 2, 2, 3 ),
 ( 0.3500000000000003109, 0.3750000000000003331, 0.4000000000000003553, 0.4250000000000003775, 0.4500000000000003997 ),
 .UNSPECIFIED. ) 
 CURVE ( )  GEOMETRIC_REPRESENTATION_ITEM ( )  RATIONAL_B_SPLINE_CURVE ( ( 0.9999999999999990008, 0.9238795325112877377, 1.000000000000000000, 0.9238795325112867385, 1.000000000000000000, 0.9238795325112867385, 1.000000000000000000, 0.9238795325112855172, 1.000000000000001110 ) ) 
 REPRESENTATION_ITEM ( '' )  );
#24416 = CARTESIAN_POINT ( 'NONE',  ( -5.444914386472299306, 34.55078125108393294, 13.14518615778179722 ) ) ;
#24417 = CARTESIAN_POINT ( 'NONE',  ( 101.8468681455907046, -4.458734124999987891, 12.00000000136559208 ) ) ;
#24418 = CONICAL_SURFACE ( 'NONE', #8035, 25.00000000000000711, 0.5235987755983000369 ) ;
#24419 = CARTESIAN_POINT ( 'NONE',  ( 55.70494972787295751, 38.27148437608393294, 9.295050272127047819 ) ) ;
#24420 = CARTESIAN_POINT ( 'NONE',  ( 65.00000000000000000, 36.13828125216787157, -13.57481594606304576 ) ) ;
#24421 = CARTESIAN_POINT ( 'NONE',  ( 103.5355339059327093, -3.535533905932726206, 2.374999999999998668 ) ) ;
#24422 = ORIENTED_EDGE ( 'NONE', *, *, #6530, .F. ) ;
#24423 = CARTESIAN_POINT ( 'NONE',  ( 13.14518615778179544, 38.76757812608393294, -1.609821015232357215E-15 ) ) ;
#24424 = CIRCLE ( 'NONE', #14391, 5.000000000000004441 ) ;
#24425 = CARTESIAN_POINT ( 'NONE',  ( 9.598844408820459861, 34.15390624999999858, 9.598844408820456309 ) ) ;
#24426 = CARTESIAN_POINT ( 'NONE',  ( 185.7049497278729575, 37.47773437608393010, -9.295050272127046043 ) ) ;
#24427 = CARTESIAN_POINT ( 'NONE',  ( 91.91746824999998466, 110.0000000000000000, -51.62499999726882294 ) ) ;
#24428 = VECTOR ( 'NONE', #17404, 1000.000000000000000 ) ;
#24429 = ORIENTED_EDGE ( 'NONE', *, *, #25360, .T. ) ;
#24430 = CARTESIAN_POINT ( 'NONE',  ( -9.598844408820458085, 34.55078124999999289, -9.598844408820458085 ) ) ;
#24431 = CARTESIAN_POINT ( 'NONE',  ( -9.295050272127044266, 34.30273437608393294, 9.295050272127047819 ) ) ;
#24432 = ORIENTED_EDGE ( 'NONE', *, *, #20493, .T. ) ;
#24433 = EDGE_LOOP ( 'NONE', ( #1704, #6756, #4664, #2624 ) ) ;
#24434 = CARTESIAN_POINT ( 'NONE',  ( 116.8548138422182063, 31.97109375108393436, -5.444914386472297529 ) ) ;
#24435 = CARTESIAN_POINT ( 'NONE',  ( 94.99999999999995737, -2.071067811865466624, 0.1875000027311852224 ) ) ;
#24436 = CARTESIAN_POINT ( 'NONE',  ( 204.2950502721270425, 34.89804687608393863, -9.295050272127046043 ) ) ;
#24437 = ORIENTED_EDGE ( 'NONE', *, *, #2814, .T. ) ;
#24438 = CARTESIAN_POINT ( 'NONE',  ( 101.4615807364564546, 123.4500000010924765, -1.461580736456474794 ) ) ;
#24439 = CARTESIAN_POINT ( 'NONE',  ( 9.295050272127046043, 33.11210937608393579, -9.295050272127046043 ) ) ;
#24440 = CARTESIAN_POINT ( 'NONE',  ( 101.7677669529663547, 124.0000000021849615, -1.767766952966370209 ) ) ;
#24441 = AXIS2_PLACEMENT_3D ( 'NONE', #14309, #16461, #3921 ) ;
#24442 = DIRECTION ( 'NONE',  ( -0.000000000000000000, -1.000000000000000000, -0.000000000000000000 ) ) ;
#24443 = DIRECTION ( 'NONE',  ( -0.000000000000000000, 1.000000000000000000, -0.000000000000000000 ) ) ;
#24444 = DIRECTION ( 'NONE',  ( 0.000000000000000000, 0.000000000000000000, 1.000000000000000000 ) ) ;
#24445 = CARTESIAN_POINT ( 'NONE',  ( 13.57481594606304576, 36.63437499999999858, -1.662435489736055892E-15 ) ) ;
#24446 = CARTESIAN_POINT ( 'NONE',  ( 71.08594421599755719, 54.65299103241510181, 14.99999999999997868 ) ) ;
#24447 = ORIENTED_EDGE ( 'NONE', *, *, #21332, .T. ) ;
#24448 = SURFACE_SIDE_STYLE ('',( #5216 ) ) ;
#24449 = CARTESIAN_POINT ( 'NONE',  ( 104.4587341249999781, -1.846868145590721655, 2.875000001365592084 ) ) ;
#24450 = ORIENTED_EDGE ( 'NONE', *, *, #8283, .T. ) ;
#24451 = CARTESIAN_POINT ( 'NONE',  ( 99.14382582708707048, 123.9000000010924794, 2.066987299999979211 ) ) ;
#24452 = CARTESIAN_POINT ( 'NONE',  ( 101.8468681455906903, -4.458734124999987891, 6.750000001365592972 ) ) ;
#24453 = CARTESIAN_POINT ( 'NONE',  ( 195.0000000000000000, 38.42031249999999432, -13.57481594606304576 ) ) ;
#24454 = CARTESIAN_POINT ( 'NONE',  ( -9.295050272127046043, 34.89804687608393152, -9.295050272127046043 ) ) ;
#24455 = CARTESIAN_POINT ( 'NONE',  ( 102.0710678118654329, 5.000000000000018652, 6.812500002731185056 ) ) ;
#24456 = DIRECTION ( 'NONE',  ( -0.000000000000000000, -1.000000000000000000, -0.000000000000000000 ) ) ;
#24457 = CARTESIAN_POINT ( 'NONE',  ( 74.59884440882045453, 37.62656250216787157, -9.598844408820458085 ) ) ;
#24458 = ADVANCED_FACE ( 'NONE', ( #553 ), #15782, .F. ) ;
#24459 = CARTESIAN_POINT ( 'NONE',  ( 185.4011555911795313, 37.72578124999999005, -9.598844408820458085 ) ) ;
#24460 = CARTESIAN_POINT ( 'NONE',  ( -5.444914386472297529, 38.02343750108394005, -13.14518615778179722 ) ) ;
#24461 = VECTOR ( 'NONE', #10613, 1000.000000000000000 ) ;
#24462 = AXIS2_PLACEMENT_3D ( 'NONE', #13122, #15269, #8591 ) ;
#24463 = CARTESIAN_POINT ( 'NONE',  ( 99.99999999999998579, 117.3602355696678643, -49.00000000546238255 ) ) ;
#24464 = CARTESIAN_POINT ( 'NONE',  ( -6.117759945536496602, 54.65941425414899868, 14.99999999999999822 ) ) ;
#24465 = CARTESIAN_POINT ( 'NONE',  ( 95.00000000000000000, 91.43749999726880162, 2.071067811865463959 ) ) ;
#24466 = CARTESIAN_POINT ( 'NONE',  ( 139.5988444088204687, 37.32890624999999574, 9.598844408820456309 ) ) ;
#24467 = ORIENTED_EDGE ( 'NONE', *, *, #7379, .T. ) ;
#24468 = ORIENTED_EDGE ( 'NONE', *, *, #2338, .F. ) ;
#24469 = CARTESIAN_POINT ( 'NONE',  ( 102.0710678118654329, -4.999999999999989342, 8.312500000000000000 ) ) ;
#24470 = CARTESIAN_POINT ( 'NONE',  ( 9.295050272127047819, 32.31835937608393294, 9.295050272127046043 ) ) ;
#24471 = CARTESIAN_POINT ( 'NONE',  ( 13.57481594606304576, 34.35234375216787583, -1.662435489736055892E-15 ) ) ;
#24472 = CARTESIAN_POINT ( 'NONE',  ( 94.99999999999995737, 2.071067811865491048, 11.06250000273118417 ) ) ;
#24473 = CARTESIAN_POINT ( 'NONE',  ( 135.4449143864723055, 32.07031250108393294, 13.14518615778179189 ) ) ;
#24474 = EDGE_CURVE ( 'NONE', #15169, #3638, #24487, .T. ) ;
#24475 = CARTESIAN_POINT ( 'NONE',  ( 51.42518405393695957, 35.49335937716787015, -5.622872871577873077 ) ) ;
#24476 = EDGE_CURVE ( 'NONE', #19007, #8752, #25054, .T. ) ;
#24477 = DIRECTION ( 'NONE',  ( 0.000000000000000000, -1.000000000000000000, -0.000000000000000000 ) ) ;
#24478 = CARTESIAN_POINT ( 'NONE',  ( 5.622872871577871301, 33.70742187716787441, -13.57481594606304753 ) ) ;
#24479 = FACE_OUTER_BOUND ( 'NONE', #14641, .T. ) ;
#24480 = CARTESIAN_POINT ( 'NONE',  ( -9.598844408820454532, 38.81718750216787583, 9.598844408820459861 ) ) ;
#24481 = CARTESIAN_POINT ( 'NONE',  ( 189.5550856135277229, 32.76484375108393010, 13.14518615778179722 ) ) ;
#24482 = DIRECTION ( 'NONE',  ( 1.000000000000000000, 0.000000000000000000, 0.000000000000000000 ) ) ;
#24483 = CARTESIAN_POINT ( 'NONE',  ( 95.67376207875072680, 104.0454443415356991, -52.70000000000000284 ) ) ;
#24484 = EDGE_CURVE ( 'NONE', #9459, #14663, #24913, .T. ) ;
#24485 = DIRECTION ( 'NONE',  ( 0.000000000000000000, 0.000000000000000000, 1.000000000000000000 ) ) ;
#24486 = CARTESIAN_POINT ( 'NONE',  ( 99.99999999999995737, 1.387778780781445676E-14, 15.00000000000000000 ) ) ;
#24487 = LINE ( 'NONE', #16210, #10113 ) ;
#24488 = CARTESIAN_POINT ( 'NONE',  ( 2.493653234604083739E-15, 34.84843749999999574, 13.57481594606304576 ) ) ;
#24489 = CARTESIAN_POINT ( 'NONE',  ( 92.99999999999998579, 112.2744378736303190, -45.10000000000001563 ) ) ;
#24490 = CARTESIAN_POINT ( 'NONE',  ( 13.14518615778179900, 34.74921875108395142, 5.444914386472293977 ) ) ;
#24491 = CARTESIAN_POINT ( 'NONE',  ( 2.414731522848535132E-15, 37.57695312608392868, 13.14518615778179544 ) ) ;
#24492 = CARTESIAN_POINT ( 'NONE',  ( 195.0000000000000000, 32.86406249999999574, -13.57481594606304576 ) ) ;
#24493 = CARTESIAN_POINT ( 'NONE',  ( 9.598844408820459861, 35.84062500216786873, 9.598844408820456309 ) ) ;
#24494 = CARTESIAN_POINT ( 'NONE',  ( 65.00000000000000000, 50.00000000000000000, -7.517135062566165128E-15 ) ) ;
#24495 = CARTESIAN_POINT ( 'NONE',  ( -13.57481594606304398, 35.49335937499999005, 5.622872871577880183 ) ) ;
#24496 = CARTESIAN_POINT ( 'NONE',  ( 78.14518615778179367, 34.55078125108393294, 5.444914386472293977 ) ) ;
#24497 = CARTESIAN_POINT ( 'NONE',  ( 99.99999999999998579, 101.5015231886685854, -52.87500000273119838 ) ) ;
#24498 = CARTESIAN_POINT ( 'NONE',  ( 97.51692799888628826, 122.9999999999999716, -0.4114429061860825354 ) ) ;
#24499 = CARTESIAN_POINT ( 'NONE',  ( 124.3771271284221598, 38.07304687716787583, 13.57481594606308128 ) ) ;
#24500 = CARTESIAN_POINT ( 'NONE',  ( 9.598844408820456309, 32.76484374999999716, -9.598844408820458085 ) ) ;
#24501 = CARTESIAN_POINT ( 'NONE',  ( 135.4449143864723055, 38.12265625108393152, -13.14518615778179900 ) ) ;
#24502 = EDGE_CURVE ( 'NONE', #22871, #24786, #22785, .T. ) ;
#24503 = ORIENTED_EDGE ( 'NONE', *, *, #8798, .T. ) ;
#24504 = CARTESIAN_POINT ( 'NONE',  ( 97.92893218813451028, 81.18750000000001421, 4.999999999999989342 ) ) ;
#24505 = CARTESIAN_POINT ( 'NONE',  ( 101.6232090348605510, 123.0000000000000426, 1.890011928979586697 ) ) ;
#24506 = CARTESIAN_POINT ( 'NONE',  ( 97.92893218813451028, 81.31250000273121259, 4.999999999999989342 ) ) ;
#24507 = CARTESIAN_POINT ( 'NONE',  ( 95.00000000000000000, 93.56249999999998579, 2.071067811865463959 ) ) ;
#24508 = CARTESIAN_POINT ( 'NONE',  ( 104.4587341249999781, 94.56249999863440792, -6.938893903907228378E-15 ) ) ;
#24509 = EDGE_CURVE ( 'NONE', #11544, #20981, #2577, .T. ) ;
#24510 = CARTESIAN_POINT ( 'NONE',  ( 94.33688103937534208, 114.1144967660473242, -53.20000000000000995 ) ) ;
#24511 = CARTESIAN_POINT ( 'NONE',  ( 51.85481384221820633, 32.81445312608393294, 0.000000000000000000 ) ) ;
#24512 = STYLED_ITEM ( 'NONE', ( #19436 ), #26371 ) ;
#24513 = VERTEX_POINT ( 'NONE', #7368 ) ;
#24514 = CARTESIAN_POINT ( 'NONE',  ( 130.0000000000000000, 39.31328125216787583, -13.57481594606304576 ) ) ;
#24515 = EDGE_CURVE ( 'NONE', #14596, #8895, #9235, .T. ) ;
#24516 = CARTESIAN_POINT ( 'NONE',  ( 103.5355339059327093, 3.535533905932755072, 11.62500000000000000 ) ) ;
#24517 = ORIENTED_EDGE ( 'NONE', *, *, #9191, .F. ) ;
#24518 = CARTESIAN_POINT ( 'NONE',  ( 9.295050272127047819, 36.28710937608393294, 9.295050272127046043 ) ) ;
#24519 = CARTESIAN_POINT ( 'NONE',  ( 204.5988444088204687, 35.04687500216787299, 9.598844408820456309 ) ) ;
#24520 = ORIENTED_EDGE ( 'NONE', *, *, #27964, .T. ) ;
#24521 = CARTESIAN_POINT ( 'NONE',  ( 13.14518615778179722, 33.75703125108393010, 5.444914386472293977 ) ) ;
#24522 = DIRECTION ( 'NONE',  ( 0.000000000000000000, 0.000000000000000000, -1.000000000000000000 ) ) ;
#24523 = CARTESIAN_POINT ( 'NONE',  ( 102.0710678118654329, -4.999999999999989342, 3.312499999999999556 ) ) ;
#24524 = CARTESIAN_POINT ( 'NONE',  ( -5.444914386472299306, 36.13828125108393863, 13.14518615778179722 ) ) ;
#24525 = DIRECTION ( 'NONE',  ( -0.000000000000000000, -0.000000000000000000, -1.000000000000000000 ) ) ;
#24526 = CARTESIAN_POINT ( 'NONE',  ( 98.15313185440923860, 91.62499999863439371, -4.458734124999994997 ) ) ;
#24527 = CARTESIAN_POINT ( 'NONE',  ( -13.57481594606304576, 34.64999999999999147, 0.000000000000000000 ) ) ;
#24528 = CARTESIAN_POINT ( 'NONE',  ( 120.8843427382055893, 35.99999999999998579, 9.510219181138795719 ) ) ;
#24529 = CARTESIAN_POINT ( 'NONE',  ( 96.84719886470459471, 3.152801135295383084, 12.56250000136559208 ) ) ;
#24530 = CARTESIAN_POINT ( 'NONE',  ( 95.54126587499996504, -1.846868145590724986, 8.500000001365592084 ) ) ;
#24531 = CARTESIAN_POINT ( 'NONE',  ( 108.0825317500000011, 112.6261737610028320, -46.02500000273120406 ) ) ;
#24532 = VECTOR ( 'NONE', #15063, 1000.000000000000000 ) ;
#24533 = FACE_OUTER_BOUND ( 'NONE', #27869, .T. ) ;
#24534 = CARTESIAN_POINT ( 'NONE',  ( 94.99999999999995737, 2.071067811865491493, 3.937500000000000000 ) ) ;
#24535 = CARTESIAN_POINT ( 'NONE',  ( 106.5389055433250860, 105.2492070361643215, -46.82499999726881867 ) ) ;
#24536 = CARTESIAN_POINT ( 'NONE',  ( -5.444914386472299306, 35.34453125108393579, 13.14518615778179722 ) ) ;
#24537 = VERTEX_POINT ( 'NONE', #20074 ) ;
#24538 =( NAMED_UNIT ( * ) PLANE_ANGLE_UNIT ( ) SI_UNIT ( $, .RADIAN. ) );
#24539 =( BOUNDED_CURVE ( )  B_SPLINE_CURVE ( 2, ( #19470, #14754, #23613, #21339, #16905, #25473, #25602, #17183, #19328, #14619, #27755 ),
 .UNSPECIFIED., .F., .T. ) 
 B_SPLINE_CURVE_WITH_KNOTS ( ( 3, 2, 2, 2, 2, 3 ),
 ( 0.1000000000000000056, 0.1200000000000000233, 0.1400000000000000688, 0.1600000000000001144, 0.1800000000000001044, 0.2000000000000001776 ),
 .UNSPECIFIED. ) 
 CURVE ( )  GEOMETRIC_REPRESENTATION_ITEM ( )  RATIONAL_B_SPLINE_CURVE ( ( 1.000000000000000000, 0.9510565162951535312, 1.000000000000000000, 0.9510565162951535312, 1.000000000000000000, 0.9510565162951535312, 1.000000000000000000, 0.9510565162951535312, 1.000000000000000000, 0.9510565162951530871, 1.000000000000000444 ) ) 
 REPRESENTATION_ITEM ( '' )  );
#24540 = LINE ( 'NONE', #9568, #7936 ) ;
#24541 = CARTESIAN_POINT ( 'NONE',  ( 2.493653234604083739E-15, 36.43593749999999432, 13.57481594606304576 ) ) ;
#24542 = EDGE_CURVE ( 'NONE', #4950, #20336, #13637, .T. ) ;
#24543 = CARTESIAN_POINT ( 'NONE',  ( 181.8548138422181921, 34.25312500108393010, 5.444914386472304635 ) ) ;
#24544 = VERTEX_POINT ( 'NONE', #13917 ) ;
#24545 =( BOUNDED_CURVE ( )  B_SPLINE_CURVE ( 2, ( #5805, #18895, #18632, #27605, #8064, #3375, #16758, #5939, #3244, #3104, #7505 ),
 .UNSPECIFIED., .F., .F. ) 
 B_SPLINE_CURVE_WITH_KNOTS ( ( 3, 2, 2, 2, 2, 3 ),
 ( 0.5999999999999998668, 0.6199999999999998845, 0.6399999999999999023, 0.6599999999999999201, 0.6799999999999999378, 0.6999999999999998446 ),
 .UNSPECIFIED. ) 
 CURVE ( )  GEOMETRIC_REPRESENTATION_ITEM ( )  RATIONAL_B_SPLINE_CURVE ( ( 1.000000000000000222, 0.9510565162951533091, 1.000000000000000000, 0.9510565162951535312, 1.000000000000000000, 0.9510565162951535312, 1.000000000000000000, 0.9510565162951535312, 1.000000000000000000, 0.9510565162951537532, 0.9999999999999997780 ) ) 
 REPRESENTATION_ITEM ( '' )  );
#24546 = CARTESIAN_POINT ( 'NONE',  ( 204.1801758136480203, 50.00000000000000000, -14.99999999999999822 ) ) ;
#24547 = CARTESIAN_POINT ( 'NONE',  ( 104.4587341249999639, 1.442382525525748735E-14, 9.187500001365592084 ) ) ;
#24548 = ORIENTED_EDGE ( 'NONE', *, *, #11040, .T. ) ;
#24549 = CARTESIAN_POINT ( 'NONE',  ( 104.3262379212492590, 104.0454443415356991, -47.30000000000000426 ) ) ;
#24550 = CARTESIAN_POINT ( 'NONE',  ( 5.444914386472302859, 36.83281250108392868, 13.14518615778179189 ) ) ;
#24551 =( GEOMETRIC_REPRESENTATION_CONTEXT ( 3 ) GLOBAL_UNCERTAINTY_ASSIGNED_CONTEXT ( ( #12945 ) ) GLOBAL_UNIT_ASSIGNED_CONTEXT ( ( #13881, #19743, #4648 ) ) REPRESENTATION_CONTEXT ( 'NONE', 'WORKASPACE' ) );
#24552 = CARTESIAN_POINT ( 'NONE',  ( 94.99999999999995737, 79.18750000273121259, 2.071067811865466624 ) ) ;
#24553 = MECHANICAL_DESIGN_GEOMETRIC_PRESENTATION_REPRESENTATION (  '', ( #26847 ), #20917 ) ;
#24554 = CARTESIAN_POINT ( 'NONE',  ( 143.1451861577818079, 37.77539062608393294, -1.609821015232357215E-15 ) ) ;
#24555 = CARTESIAN_POINT ( 'NONE',  ( 13.14518615778179544, 40.35507812608393863, -1.609821015232357215E-15 ) ) ;
#24556 = CARTESIAN_POINT ( 'NONE',  ( -13.14518615778179900, 34.94765625108392726, -5.444914386472297529 ) ) ;
#24557 = CARTESIAN_POINT ( 'NONE',  ( 95.00000000000000000, 93.37499999726881583, -7.551217303480904118E-15 ) ) ;
#24558 = CARTESIAN_POINT ( 'NONE',  ( 70.44491438647230552, 37.82500000108392868, 13.14518615778179189 ) ) ;
#24559 = CARTESIAN_POINT ( 'NONE',  ( 72.63624106799308322, 54.91786508990981730, -15.00000000000000000 ) ) ;
#24560 = CARTESIAN_POINT ( 'NONE',  ( 106.5389055433251002, 114.7507929638356785, -50.17500000273119554 ) ) ;
#24561 = CARTESIAN_POINT ( 'NONE',  ( 200.4449143864723055, 32.56640625108394005, -13.14518615778179900 ) ) ;
#24562 = DIRECTION ( 'NONE',  ( 0.000000000000000000, 0.000000000000000000, -1.000000000000000000 ) ) ;
#24563 = EDGE_LOOP ( 'NONE', ( #22054, #21560, #5767, #7031 ) ) ;
#24564 = CARTESIAN_POINT ( 'NONE',  ( -8.049105076161786076E-16, 36.58476562608393579, -13.14518615778179544 ) ) ;
#24565 = CARTESIAN_POINT ( 'NONE',  ( 98.15313185440923860, -4.458734124999987891, 8.875000001365592084 ) ) ;
#24566 = CARTESIAN_POINT ( 'NONE',  ( 78.14518615778179367, 37.77539062608393294, -1.609821015232357215E-15 ) ) ;
#24567 = CARTESIAN_POINT ( 'NONE',  ( 94.99999999999995737, 1.387778780781445676E-14, 7.125000002731185056 ) ) ;
#24568 = CARTESIAN_POINT ( 'NONE',  ( 102.0710678118654329, -4.999999999999989342, 14.31249999999999645 ) ) ;
#24569 = CARTESIAN_POINT ( 'NONE',  ( 5.444914386472297529, 33.36015625108393579, -13.14518615778179722 ) ) ;
#24570 = ORIENTED_EDGE ( 'NONE', *, *, #23409, .F. ) ;
#24571 = CARTESIAN_POINT ( 'NONE',  ( 130.0000000000000000, 39.21406249999999716, -13.57481594606304576 ) ) ;
#24572 = MECHANICAL_DESIGN_GEOMETRIC_PRESENTATION_REPRESENTATION (  '', ( #11342 ), #20016 ) ;
#24573 = CARTESIAN_POINT ( 'NONE',  ( 195.0000000000000000, 38.56914062608393579, 13.14518615778179544 ) ) ;
#24574 = CARTESIAN_POINT ( 'NONE',  ( 95.00472066334982912, 103.1245878333314323, -47.57499999726882578 ) ) ;
#24575 = ORIENTED_EDGE ( 'NONE', *, *, #19099, .F. ) ;
#24576 = CARTESIAN_POINT ( 'NONE',  ( 2.493653234604083739E-15, 34.84843749999999574, 13.57481594606304576 ) ) ;
#24577 = CARTESIAN_POINT ( 'NONE',  ( 13.14518615778179900, 32.96328125108393436, 5.444914386472293977 ) ) ;
#24578 = ORIENTED_EDGE ( 'NONE', *, *, #2702, .T. ) ;
#24579 = CARTESIAN_POINT ( 'NONE',  ( 143.1451861577818079, 34.00507812608393721, -1.609821015232357215E-15 ) ) ;
#24580 = AXIS2_PLACEMENT_3D ( 'NONE', #25446, #5927, #23313 ) ;
#24581 = CARTESIAN_POINT ( 'NONE',  ( 185.7049497278729575, 32.71523437608393436, -9.295050272127046043 ) ) ;
#24582 = VERTEX_POINT ( 'NONE', #20644 ) ;
#24583 = CARTESIAN_POINT ( 'NONE',  ( 104.9999999999999716, 1.449011120738813565E-14, 10.62500000273118594 ) ) ;
#24584 = CARTESIAN_POINT ( 'NONE',  ( 102.0710678118654329, 5.000000000000018652, 8.812500002731184168 ) ) ;
#24585 = CARTESIAN_POINT ( 'NONE',  ( 120.8198241863519655, 55.00000000000000000, -15.00000000000000000 ) ) ;
#24586 = CARTESIAN_POINT ( 'NONE',  ( 124.3771271284221314, 38.56914062716788294, -13.57481594606304753 ) ) ;
#24587 = CARTESIAN_POINT ( 'NONE',  ( 104.9952793366501709, 116.8754121666685393, -47.82500000273119412 ) ) ;
#24588 =( BOUNDED_CURVE ( )  B_SPLINE_CURVE ( 2, ( #11552, #7287, #6866, #13551, #11126, #7003, #26548, #24261, #19990, #9426, #20268 ),
 .UNSPECIFIED., .F., .T. ) 
 B_SPLINE_CURVE_WITH_KNOTS ( ( 3, 2, 2, 2, 2, 3 ),
 ( 0.2000000000000001776, 0.2200000000000001676, 0.2400000000000001854, 0.2600000000000002309, 0.2800000000000002487, 0.3000000000000002109 ),
 .UNSPECIFIED. ) 
 CURVE ( )  GEOMETRIC_REPRESENTATION_ITEM ( )  RATIONAL_B_SPLINE_CURVE ( ( 0.9999999999999995559, 0.9510565162951539753, 1.000000000000000000, 0.9510565162951535312, 1.000000000000000000, 0.9510565162951535312, 1.000000000000000000, 0.9510565162951535312, 1.000000000000000000, 0.9510565162951529761, 1.000000000000000444 ) ) 
 REPRESENTATION_ITEM ( '' )  );
#24589 = CARTESIAN_POINT ( 'NONE',  ( 103.5355339059327093, -3.535533905932726206, 2.500000002731185500 ) ) ;
#24590 = CARTESIAN_POINT ( 'NONE',  ( -5.622872871577873966, 34.10429687716786873, 13.57481594606304753 ) ) ;
#24591 = B_SPLINE_CURVE_WITH_KNOTS ( 'NONE', 3,
 ( #24025, #3945, #4503, #27748, #8346, #13160, #21471, #21899, #8208, #12604, #10616, #25595, #14745, #12878, #21328, #10474, #19182, #1947 ),
 .UNSPECIFIED., .F., .F.,
 ( 4, 2, 2, 2, 2, 2, 2, 2, 4 ),
 ( 0.000000000000000000, 0.004618502246277159280, 0.006927753369415741089, 0.009237004492554322030, 0.01039163005412361424, 0.01154625561569290644, 0.01385550673883148391, 0.01616475786197006312, 0.01847400898510863712 ),
 .UNSPECIFIED. ) ;
#24592 = CARTESIAN_POINT ( 'NONE',  ( 66.81435535458352604, 51.46618445021699273, 14.99999999999929834 ) ) ;
#24593 = PRODUCT_DEFINITION ( 'UNKNOWN', '', #26804, #14597 ) ;
#24594 = VECTOR ( 'NONE', #9666, 1000.000000000000000 ) ;
#24595 = ADVANCED_FACE ( 'NONE', ( #22496 ), #26781, .T. ) ;
#24596 = VERTEX_POINT ( 'NONE', #987 ) ;
#24597 = SURFACE_STYLE_USAGE ( .BOTH. , #24448 ) ;
#24598 = CARTESIAN_POINT ( 'NONE',  ( 95.54126587499995082, 1.846868145590750077, 4.375000001365592084 ) ) ;
#24599 = VERTEX_POINT ( 'NONE', #9796 ) ;
#24600 = CARTESIAN_POINT ( 'NONE',  ( 94.99999999999995737, 1.387778780781445676E-14, 4.000000000000000000 ) ) ;
#24601 = CARTESIAN_POINT ( 'NONE',  ( 101.8468681455906903, 4.458734125000016313, 8.125000001365592084 ) ) ;
#24602 = CARTESIAN_POINT ( 'NONE',  ( 130.0000000000000000, 38.12265625216787157, 13.57481594606304576 ) ) ;
#24603 = CARTESIAN_POINT ( 'NONE',  ( -9.295050272127044266, 37.47773437608393010, 9.295050272127047819 ) ) ;
#24604 = CARTESIAN_POINT ( 'NONE',  ( 195.0000000000000000, 40.10703125216787157, -13.57481594606304576 ) ) ;
#24605 = CARTESIAN_POINT ( 'NONE',  ( 105.0000000000000000, 110.0000000000000000, -45.00000000000000711 ) ) ;
#24606 = CARTESIAN_POINT ( 'NONE',  ( 104.4587341249999923, 92.37499999863440792, -1.846868145590737198 ) ) ;
#24607 = CARTESIAN_POINT ( 'NONE',  ( 99.99999999999998579, 101.5015231886685854, -48.62500000273119838 ) ) ;
#24608 = CARTESIAN_POINT ( 'NONE',  ( -13.14518615778179722, 38.12265625108393863, -5.444914386472297529 ) ) ;
#24609 = CARTESIAN_POINT ( 'NONE',  ( 13.57481594606304576, 35.14609375216787157, -1.662435489736055892E-15 ) ) ;
#24610 = CARTESIAN_POINT ( 'NONE',  ( 1.814355354584273661, 51.46618445021836408, 15.00000000000034106 ) ) ;
#24611 = CARTESIAN_POINT ( 'NONE',  ( 99.99999999999995737, 1.387778780781445676E-14, 0.000000000000000000 ) ) ;
#24612 = CARTESIAN_POINT ( 'NONE',  ( 139.5988444088204687, 34.15390624999999858, 9.598844408820456309 ) ) ;
#24613 = ORIENTED_EDGE ( 'NONE', *, *, #2854, .T. ) ;
#24614 = CARTESIAN_POINT ( 'NONE',  ( 2.493653234604083739E-15, 33.36015625216786873, 13.57481594606304576 ) ) ;
#24615 = CARTESIAN_POINT ( 'NONE',  ( 5.444914386472297529, 33.36015625108393579, -13.14518615778179900 ) ) ;
#24616 = CARTESIAN_POINT ( 'NONE',  ( -13.57481594606304753, 33.90585937716787868, -5.622872871577873077 ) ) ;
#24617 = CARTESIAN_POINT ( 'NONE',  ( 94.99999999999995737, 1.387778780781445676E-14, 9.125000002731184168 ) ) ;
#24618 = CARTESIAN_POINT ( 'NONE',  ( 139.2950502721270425, 33.11210937608393579, -9.295050272127046043 ) ) ;
#24619 = CARTESIAN_POINT ( 'NONE',  ( 51.42518405393695957, 31.52460937716787370, -5.622872871577873077 ) ) ;
#24620 = CIRCLE ( 'NONE', #12301, 7.000000000000006217 ) ;
#24621 = CARTESIAN_POINT ( 'NONE',  ( 2.493653234604083739E-15, 38.12265625216787157, 13.57481594606304576 ) ) ;
#24622 = CARTESIAN_POINT ( 'NONE',  ( 13.14518615778179544, 37.77539062608393294, -1.609821015232357215E-15 ) ) ;
#24623 = CARTESIAN_POINT ( 'NONE',  ( 102.0710678118654329, -4.999999999999989342, 2.312499999999998668 ) ) ;
#24624 = CARTESIAN_POINT ( 'NONE',  ( 106.5389055433250860, 105.2492070361643215, -51.07499999726882578 ) ) ;
#24625 = AXIS2_PLACEMENT_3D ( 'NONE', #18868, #27578, #23301 ) ;
#24626 = CARTESIAN_POINT ( 'NONE',  ( 5.622872871577878406, 39.75976562716787299, 13.57481594606304576 ) ) ;
#24627 = CARTESIAN_POINT ( 'NONE',  ( -9.295050272127046043, 40.45429687608393721, -9.295050272127046043 ) ) ;
#24628 = FACE_OUTER_BOUND ( 'NONE', #8214, .T. ) ;
#24629 = DIRECTION ( 'NONE',  ( 0.000000000000000000, 1.000000000000000000, -0.000000000000000000 ) ) ;
#24630 = LINE ( 'NONE', #5107, #27344 ) ;
#24631 = CARTESIAN_POINT ( 'NONE',  ( 181.4251840539369596, 40.25585937499999289, 5.622872871577880183 ) ) ;
#24632 = CARTESIAN_POINT ( 'NONE',  ( 97.92893218813451028, -4.999999999999989342, 10.31250000273118417 ) ) ;
#24633 = CARTESIAN_POINT ( 'NONE',  ( 99.99999999999998579, 89.99899999999999523, -9.540979117872439019E-15 ) ) ;
#24634 = CARTESIAN_POINT ( 'NONE',  ( 13.57481594606304931, 33.40976562499999858, 5.622872871577869525 ) ) ;
#24635 = CARTESIAN_POINT ( 'NONE',  ( 130.0000000000000000, -7.395377635281828788, -1.503427012513233026E-14 ) ) ;
#24636 = CARTESIAN_POINT ( 'NONE',  ( -13.14518615778179900, 35.14609375108393152, -5.444914386472297529 ) ) ;
#24637 = CARTESIAN_POINT ( 'NONE',  ( -5.444914386472297529, 37.22968750108393721, -13.14518615778179900 ) ) ;
#24638 = EDGE_CURVE ( 'NONE', #2105, #17002, #15917, .T. ) ;
#24639 = CARTESIAN_POINT ( 'NONE',  ( -13.14518615778179544, 35.79101562608393294, 0.000000000000000000 ) ) ;
#24640 = CIRCLE ( 'NONE', #25988, 5.000000000000004441 ) ;
#24641 = CARTESIAN_POINT ( 'NONE',  ( -13.57481594606304576, 34.74921875216787726, 0.000000000000000000 ) ) ;
#24642 = CARTESIAN_POINT ( 'NONE',  ( -5.622872871577964560, 37.77539062716787299, -13.57481594606295339 ) ) ;
#24643 = CARTESIAN_POINT ( 'NONE',  ( -13.57481594606304753, 35.39414062499999147, -5.622872871577872189 ) ) ;
#24644 = CARTESIAN_POINT ( 'NONE',  ( 78.14518615778179367, 40.40468750108393436, -5.444914386472297529 ) ) ;
#24645 = ADVANCED_FACE ( 'NONE', ( #7663 ), #18357, .F. ) ;
#24646 = CARTESIAN_POINT ( 'NONE',  ( 104.9952793366501851, 116.8754121666685393, -52.07500000273120122 ) ) ;
#24647 = CARTESIAN_POINT ( 'NONE',  ( 101.7406320503887684, 123.0000000000000000, -1.800178865752367408 ) ) ;
#24648 = CARTESIAN_POINT ( 'NONE',  ( 101.4615807364564546, 123.2500000010924879, 1.461580736456455476 ) ) ;
#24649 = CARTESIAN_POINT ( 'NONE',  ( 9.598844408820459861, 34.15390624999999858, 9.598844408820456309 ) ) ;
#24650 = CARTESIAN_POINT ( 'NONE',  ( 143.1451861577818079, 38.02343750108395426, -5.444914386472297529 ) ) ;
#24651 = VERTEX_POINT ( 'NONE', #11495 ) ;
#24652 = CARTESIAN_POINT ( 'NONE',  ( 94.99999999999995737, 81.93750000000001421, -2.071067811865491048 ) ) ;
#24653 = DIRECTION ( 'NONE',  ( 1.374060148949977908E-06, 0.9999999999986906030, 8.549343071804204525E-07 ) ) ;
#24654 = CARTESIAN_POINT ( 'NONE',  ( 99.99999999999995737, 84.18750000136560629, -4.458734125000016313 ) ) ;
#24655 = CARTESIAN_POINT ( 'NONE',  ( 104.9999999999999716, 94.06249999999998579, -2.071067811865478170 ) ) ;
#24656 = CARTESIAN_POINT ( 'NONE',  ( 59.37712712842213136, 39.36289062716787157, -13.57481594606304753 ) ) ;
#24657 = EDGE_CURVE ( 'NONE', #17053, #5414, #20211, .T. ) ;
#24658 = CARTESIAN_POINT ( 'NONE',  ( 102.1631189606246295, 103.3426043859339103, -54.40000000000001279 ) ) ;
#24659 = CARTESIAN_POINT ( 'NONE',  ( 74.29505027212704249, 33.11210937608393579, 9.295050272127046043 ) ) ;
#24660 = ADVANCED_BREP_SHAPE_REPRESENTATION ( '', ( #7835, #26844 ), #7245 ) ;
#24661 = ORIENTED_EDGE ( 'NONE', *, *, #15225, .T. ) ;
#24662 = CARTESIAN_POINT ( 'NONE',  ( 96.46446609406721961, 3.535533905932755072, 14.87500000000000000 ) ) ;
#24663 = ORIENTED_EDGE ( 'NONE', *, *, #23920, .T. ) ;
#24664 = CARTESIAN_POINT ( 'NONE',  ( 13.14518615778179900, 37.13046875108393863, 5.444914386472293977 ) ) ;
#24665 = CARTESIAN_POINT ( 'NONE',  ( 200.6228728715778686, 33.40976562716787157, 13.57481594606304576 ) ) ;
#24666 = CARTESIAN_POINT ( 'NONE',  ( 9.295050272127047819, 33.70742187608393436, 9.295050272127046043 ) ) ;
#24667 = CARTESIAN_POINT ( 'NONE',  ( -8.312177448680279460E-16, 32.07031249999999289, -13.57481594606304576 ) ) ;
#24668 = EDGE_CURVE ( 'NONE', #23118, #4924, #24796, .T. ) ;
#24669 = LINE ( 'NONE', #5287, #5277 ) ;
#24670 = CARTESIAN_POINT ( 'NONE',  ( -13.14518615778179544, 34.40195312608393152, 0.000000000000000000 ) ) ;
#24671 = CARTESIAN_POINT ( 'NONE',  ( 130.0000000000000000, 33.21132812608393436, -13.14518615778179544 ) ) ;
#24672 = CARTESIAN_POINT ( 'NONE',  ( 96.84719886470463734, 90.68749999863440792, -3.152801135295366208 ) ) ;
#24673 = CARTESIAN_POINT ( 'NONE',  ( 99.99999999999998579, 124.5500000010924708, -2.066987299999998751 ) ) ;
#24674 = DIRECTION ( 'NONE',  ( 1.000000000000000000, 0.000000000000000000, 0.000000000000000000 ) ) ;
#24675 = CARTESIAN_POINT ( 'NONE',  ( -9.598844408820458085, 32.96328124999999432, -9.598844408820458085 ) ) ;
#24676 = CARTESIAN_POINT ( 'NONE',  ( 95.54126587499996504, 1.387778780781445676E-14, 7.687500001365592084 ) ) ;
#24677 = CARTESIAN_POINT ( 'NONE',  ( 189.3771271284222735, 36.88242187499999858, -13.57481594606318254 ) ) ;
#24678 = CARTESIAN_POINT ( 'NONE',  ( 101.8468681455907046, -4.458734124999987891, 9.750000001365593860 ) ) ;
#24679 = CARTESIAN_POINT ( 'NONE',  ( 97.50236033167492167, 117.6869444889999841, -45.52500000273119696 ) ) ;
#24680 = CARTESIAN_POINT ( 'NONE',  ( 96.84719886470463734, 90.93749999863440792, -3.152801135295366208 ) ) ;
#24681 = CARTESIAN_POINT ( 'NONE',  ( 99.99999999999998579, 128.0000000000000000, -11.50000000000001954 ) ) ;
#24682 = CARTESIAN_POINT ( 'NONE',  ( 9.180175813647995398, 55.00000000000000000, 14.99999999999999467 ) ) ;
#24683 = CARTESIAN_POINT ( 'NONE',  ( 5.444914386472302859, 32.26875000108393721, 13.14518615778179189 ) ) ;
#24684 = ADVANCED_FACE ( 'NONE', ( #21057 ), #579, .F. ) ;
#24685 = ORIENTED_EDGE ( 'NONE', *, *, #7420, .F. ) ;
#24686 = CARTESIAN_POINT ( 'NONE',  ( 116.4251840539369596, 36.98164062499999005, -5.622872871577872189 ) ) ;
#24687 = DIRECTION ( 'NONE',  ( 0.000000000000000000, 0.000000000000000000, 1.000000000000000000 ) ) ;
#24688 = DIRECTION ( 'NONE',  ( 3.469446951953613696E-16, 0.000000000000000000, 1.000000000000000000 ) ) ;
#24689 = CARTESIAN_POINT ( 'NONE',  ( 185.7049497278729575, 36.48554687608393721, -9.295050272127046043 ) ) ;
#24690 = ORIENTED_EDGE ( 'NONE', *, *, #24303, .T. ) ;
#24691 = CARTESIAN_POINT ( 'NONE',  ( 186.6077847083615495, 54.99999999999997868, -14.99999999999999645 ) ) ;
#24692 = CARTESIAN_POINT ( 'NONE',  ( 98.15313185440925281, 4.458734125000016313, 9.500000001365593860 ) ) ;
#24693 = ORIENTED_EDGE ( 'NONE', *, *, #15166, .F. ) ;
#24694 = CARTESIAN_POINT ( 'NONE',  ( 104.3262379212492590, 115.9545556584642867, -46.69999999999999574 ) ) ;
#24695 = CARTESIAN_POINT ( 'NONE',  ( 13.14518615778179544, 37.77539062608393294, -1.609821015232357215E-15 ) ) ;
#24696 = CARTESIAN_POINT ( 'NONE',  ( 217.9999999999999716, 52.00000000000000711, -13.00000000000000000 ) ) ;
#24697 = CARTESIAN_POINT ( 'NONE',  ( 99.99999999999998579, 123.2000000000000028, -2.499999999999997780 ) ) ;
#24698 = CARTESIAN_POINT ( 'NONE',  ( 120.7049497278729575, 36.48554687608393721, -9.295050272127046043 ) ) ;
#24699 = CARTESIAN_POINT ( 'NONE',  ( 2.414731522848535132E-15, 37.77539062608393294, 13.14518615778179544 ) ) ;
#24700 = CARTESIAN_POINT ( 'NONE',  ( -5.444914386472297529, 34.05468750108393294, -13.14518615778179900 ) ) ;
#24701 = CARTESIAN_POINT ( 'NONE',  ( 95.54126587500000767, 93.06249999863440792, -7.484931351350258973E-15 ) ) ;
#24702 = CARTESIAN_POINT ( 'NONE',  ( -13.57481594606304398, 36.38632812716788578, 5.622872871577880183 ) ) ;
#24703 = CARTESIAN_POINT ( 'NONE',  ( 108.0825317500000153, 110.0000000000000000, -50.37500000273119127 ) ) ;
#24704 = AXIS2_PLACEMENT_3D ( 'NONE', #24633, #22352, #16355 ) ;
#24705 = CARTESIAN_POINT ( 'NONE',  ( 68.30411859782175554, 35.99999999999998579, 12.77244747738262731 ) ) ;
#24706 = CARTESIAN_POINT ( 'NONE',  ( 13.14518615778179900, 34.74921875108395142, 5.444914386472293977 ) ) ;
#24707 = CARTESIAN_POINT ( 'NONE',  ( 95.54126587499996504, 1.387778780781445676E-14, 8.687500001365592084 ) ) ;
#24708 =( BOUNDED_CURVE ( )  B_SPLINE_CURVE ( 2, ( #12340, #5044, #13708, #2477, #486, #22428, #12883 ),
 .UNSPECIFIED., .F., .F. ) 
 B_SPLINE_CURVE_WITH_KNOTS ( ( 3, 2, 2, 3 ),
 ( 0.4166666666666666297, 0.4583333333333332593, 0.5000000000000000000, 0.5416666676520737189 ),
 .UNSPECIFIED. ) 
 CURVE ( )  GEOMETRIC_REPRESENTATION_ITEM ( )  RATIONAL_B_SPLINE_CURVE ( ( 1.000000000000000000, 0.9238795325112866275, 1.000000000000000000, 0.9238795325112867385, 1.000000000000000000, 0.9238795325112867385, 1.000000000000000000 ) ) 
 REPRESENTATION_ITEM ( '' )  );
#24709 = CARTESIAN_POINT ( 'NONE',  ( 59.55508561352770158, 37.22968750108394431, -13.14518615778179722 ) ) ;
#24710 = PRODUCT_DEFINITION_SHAPE ( 'NONE', 'NONE',  #24593 ) ;
#24711 = EDGE_CURVE ( 'NONE', #12289, #4613, #4546, .T. ) ;
#24712 = CARTESIAN_POINT ( 'NONE',  ( 2.816687638038913930E-15, 21.95886589889650509, 23.00000000000001421 ) ) ;
#24713 = CARTESIAN_POINT ( 'NONE',  ( 185.7049497278729575, 36.48554687608393721, -9.295050272127046043 ) ) ;
#24714 = CARTESIAN_POINT ( 'NONE',  ( -5.444914386472297529, 33.45937500108394147, -13.14518615778179722 ) ) ;
#24715 = CARTESIAN_POINT ( 'NONE',  ( 99.99999999999998579, 124.3500000010924822, -2.066987299999998751 ) ) ;
#24716 = CARTESIAN_POINT ( 'NONE',  ( -13.57481594606304398, 36.28710937499999289, 5.622872871577880183 ) ) ;
#24717 = CARTESIAN_POINT ( 'NONE',  ( 189.5550856135277229, 39.31328125108392868, 13.14518615778179722 ) ) ;
#24718 = CARTESIAN_POINT ( 'NONE',  ( 104.9952793366501709, 103.1245878333314323, -51.17499999726881299 ) ) ;
#24719 = ORIENTED_EDGE ( 'NONE', *, *, #13648, .F. ) ;
#24720 = CARTESIAN_POINT ( 'NONE',  ( -5.622872871577873077, 32.41757812499999858, 13.57481594606304753 ) ) ;
#24721 = CARTESIAN_POINT ( 'NONE',  ( 2.414731522848535132E-15, 32.81445312608393294, 13.14518615778179544 ) ) ;
#24722 = VERTEX_POINT ( 'NONE', #13353 ) ;
#24723 = CARTESIAN_POINT ( 'NONE',  ( 135.4449143864723055, 33.36015625108393579, -13.14518615778179900 ) ) ;
#24724 = CARTESIAN_POINT ( 'NONE',  ( 195.0000000000000000, 36.93203125216787441, -13.57481594606304576 ) ) ;
#24725 = CARTESIAN_POINT ( 'NONE',  ( 195.0000000000000000, 34.99726562608393721, -13.14518615778179544 ) ) ;
#24726 = ORIENTED_EDGE ( 'NONE', *, *, #22826, .T. ) ;
#24727 = CARTESIAN_POINT ( 'NONE',  ( 104.9999999999999716, 1.449011120738813565E-14, 13.50000000000000000 ) ) ;
#24728 = CARTESIAN_POINT ( 'NONE',  ( 104.9999999999999716, 1.449011120738813565E-14, 8.625000002731185944 ) ) ;
#24729 = CARTESIAN_POINT ( 'NONE',  ( 94.99999999999995737, 1.387778780781445676E-14, 1.125000002731184390 ) ) ;
#24730 = CARTESIAN_POINT ( 'NONE',  ( 116.4251840539369596, 36.33671875216787583, 0.000000000000000000 ) ) ;
#24731 = CARTESIAN_POINT ( 'NONE',  ( 95.00472066334981491, 103.1245878333314465, -44.82500000273118701 ) ) ;
#24732 = DIRECTION ( 'NONE',  ( 0.000000000000000000, -1.000000000000000000, 0.000000000000000000 ) ) ;
#24733 = CARTESIAN_POINT ( 'NONE',  ( 13.57481594606304931, 36.58476562499999574, 5.622872871577868636 ) ) ;
#24734 = CARTESIAN_POINT ( 'NONE',  ( 195.0000000000000000, 40.15664062608393436, 13.14518615778179544 ) ) ;
#24735 = FILL_AREA_STYLE_COLOUR ( '', #10413 ) ;
#24736 = CARTESIAN_POINT ( 'NONE',  ( 99.99999999999995737, -4.458734124999988779, 5.687500001365591196 ) ) ;
#24737 = ORIENTED_EDGE ( 'NONE', *, *, #14397, .F. ) ;
#24738 = CARTESIAN_POINT ( 'NONE',  ( 3.089260913797906571, 36.00000000000000000, -13.21136010216355672 ) ) ;
#24739 = CARTESIAN_POINT ( 'NONE',  ( 98.15313185440925281, -4.458734124999987891, 8.625000001365593860 ) ) ;
#24740 = CARTESIAN_POINT ( 'NONE',  ( 133.0446094569239506, 53.89089363584123760, 14.99999999999996447 ) ) ;
#24741 = CARTESIAN_POINT ( 'NONE',  ( -9.115657261794684274, 36.00000000000000000, 9.510219181138523936 ) ) ;
#24742 = CARTESIAN_POINT ( 'NONE',  ( 65.00000000000000000, 33.40976562608393863, -13.14518615778179544 ) ) ;
#24743 = AXIS2_PLACEMENT_3D ( 'NONE', #2406, #21930, #11066 ) ;
#24744 = CARTESIAN_POINT ( 'NONE',  ( 103.5355339059327093, -3.535533905932726206, 5.375000000000000000 ) ) ;
#24745 = CARTESIAN_POINT ( 'NONE',  ( 106.5389055433251002, 114.7507929638356785, -47.92500000273120264 ) ) ;
#24746 = CARTESIAN_POINT ( 'NONE',  ( -13.57481594606304753, 38.56914062499999574, -5.622872871577872189 ) ) ;
#24747 = CARTESIAN_POINT ( 'NONE',  ( 13.57481594606304931, 35.09648437716787583, 5.622872871577868636 ) ) ;
#24748 = CARTESIAN_POINT ( 'NONE',  ( 0.3286002765677282222, 53.49358765998907472, 14.99999999999999645 ) ) ;
#24749 = CARTESIAN_POINT ( 'NONE',  ( 130.0000000000000000, 35.24531249999999716, -13.57481594606304576 ) ) ;
#24750 = ORIENTED_EDGE ( 'NONE', *, *, #22413, .F. ) ;
#24751 = DIRECTION ( 'NONE',  ( -0.000000000000000000, 1.000000000000000000, -0.000000000000000000 ) ) ;
#24752 = CARTESIAN_POINT ( 'NONE',  ( 13.14518615778179544, 33.21132812608393436, -1.609821015232357215E-15 ) ) ;
#24753 = CARTESIAN_POINT ( 'NONE',  ( 5.622872871577871301, 33.70742187716787441, -13.57481594606304753 ) ) ;
#24754 = CARTESIAN_POINT ( 'NONE',  ( 94.99999999999995737, -2.071067811865466624, 11.18750000273118594 ) ) ;
#24755 = CARTESIAN_POINT ( 'NONE',  ( 116.8548138422182063, 32.66562500108393863, 5.444914386472304635 ) ) ;
#24756 = CARTESIAN_POINT ( 'NONE',  ( 65.00000000000000000, 40.35507812608393152, -13.14518615778179544 ) ) ;
#24757 = ADVANCED_FACE ( 'NONE', ( #24213 ), #19790, .T. ) ;
#24758 =( BOUNDED_CURVE ( )  B_SPLINE_CURVE ( 2, ( #23507, #8530, #15785, #20213, #4687, #125, #18067, #13639, #9372, #8951, #15645 ),
 .UNSPECIFIED., .F., .F. ) 
 B_SPLINE_CURVE_WITH_KNOTS ( ( 3, 2, 2, 2, 2, 3 ),
 ( 0.000000000000000000, 0.02000000000000000042, 0.04000000000000000083, 0.05999999999999999778, 0.08000000000000000167, 0.1000000000000000194 ),
 .UNSPECIFIED. ) 
 CURVE ( )  GEOMETRIC_REPRESENTATION_ITEM ( )  RATIONAL_B_SPLINE_CURVE ( ( 1.000000000000000000, 0.9510565162951535312, 1.000000000000000000, 0.9510565162951535312, 1.000000000000000000, 0.9510565162951535312, 1.000000000000000000, 0.9510565162951535312, 1.000000000000000000, 0.9510565162951535312, 1.000000000000000000 ) ) 
 REPRESENTATION_ITEM ( '' )  );
#24759 = CARTESIAN_POINT ( 'NONE',  ( 130.0000000000000000, -7.395377635281828788, -1.503427012513233026E-14 ) ) ;
#24760 = CARTESIAN_POINT ( 'NONE',  ( -5.444914386472297529, 38.81718750108393579, -13.14518615778179900 ) ) ;
#24761 = CARTESIAN_POINT ( 'NONE',  ( -13.14518615778179544, 32.81445312608393294, 0.000000000000000000 ) ) ;
#24762 = CARTESIAN_POINT ( 'NONE',  ( -15.00000000000000000, 55.00000000000000000, 10.00000000000000000 ) ) ;
#24763 = CARTESIAN_POINT ( 'NONE',  ( 91.91746824999998466, 110.0000000000000000, -55.87499999726882294 ) ) ;
#24764 = CARTESIAN_POINT ( 'NONE',  ( -5.622872871577873077, 38.56914062716788294, -13.57481594606304753 ) ) ;
#24765 = CARTESIAN_POINT ( 'NONE',  ( 189.5550856135277229, 32.46718750108393436, -13.14518615778179900 ) ) ;
#24766 = CARTESIAN_POINT ( 'NONE',  ( 94.99999999999995737, 2.071067811865491493, 6.062500002731184168 ) ) ;
#24767 = CARTESIAN_POINT ( 'NONE',  ( 98.23223304703363112, 124.1069999999781572, -1.767766952966370209 ) ) ;
#24768 = CARTESIAN_POINT ( 'NONE',  ( 100.8561741729129153, 123.5000000010924737, -2.066987299999999195 ) ) ;
#24769 = CARTESIAN_POINT ( 'NONE',  ( 195.0000000000000000, 39.61093749999999147, 13.57481594606304576 ) ) ;
#24770 = DIRECTION ( 'NONE',  ( -1.000000000000000000, 0.000000000000000000, 0.000000000000000000 ) ) ;
#24771 = CARTESIAN_POINT ( 'NONE',  ( 87.00000000000000000, 118.0000000000000000, -15.00000000000000533 ) ) ;
#24772 = CARTESIAN_POINT ( 'NONE',  ( 2.493653234604083739E-15, 34.05468749999999289, 13.57481594606304576 ) ) ;
#24773 = DIRECTION ( 'NONE',  ( -0.000000000000000000, -1.000000000000000000, -0.000000000000000000 ) ) ;
#24774 = CARTESIAN_POINT ( 'NONE',  ( 9.295050272127047819, 33.11210937608393579, 9.295050272127046043 ) ) ;
#24775 = CARTESIAN_POINT ( 'NONE',  ( -9.295050272127044266, 34.30273437608393294, 9.295050272127047819 ) ) ;
#24776 = CARTESIAN_POINT ( 'NONE',  ( 0.5696516875510663214, 35.99464330212366292, 13.14518615778179544 ) ) ;
#24777 = CARTESIAN_POINT ( 'NONE',  ( 5.622872871577871301, 37.67617187716787441, -13.57481594606304753 ) ) ;
#24778 = CARTESIAN_POINT ( 'NONE',  ( -9.598844408820458085, 37.82500000216787583, -9.598844408820458085 ) ) ;
#24779 = CARTESIAN_POINT ( 'NONE',  ( 104.4587341249999781, 83.00000000136559208, -1.846868145590750299 ) ) ;
#24780 = CARTESIAN_POINT ( 'NONE',  ( 65.00000000000000000, 33.21132812608393436, -13.14518615778179544 ) ) ;
#24781 = DIRECTION ( 'NONE',  ( 0.000000000000000000, 0.000000000000000000, -1.000000000000000000 ) ) ;
#24782 = DIRECTION ( 'NONE',  ( 0.000000000000000000, 0.000000000000000000, 1.000000000000000000 ) ) ;
#24783 = CARTESIAN_POINT ( 'NONE',  ( 116.4251840539369596, 37.87460937716787868, -5.622872871577872189 ) ) ;
#24784 = CARTESIAN_POINT ( 'NONE',  ( -8.312177448680279460E-16, 34.45156249999999432, -13.57481594606304576 ) ) ;
#24785 = CARTESIAN_POINT ( 'NONE',  ( 143.1451861577818079, 34.74921875108395142, 5.444914386472293977 ) ) ;
#24786 = VERTEX_POINT ( 'NONE', #17367 ) ;
#24787 = CARTESIAN_POINT ( 'NONE',  ( 94.99999999999998579, 110.0000000000000000, -45.00000000000000711 ) ) ;
#24788 = CARTESIAN_POINT ( 'NONE',  ( 95.00000000000000000, 94.43750000000001421, -2.071067811865479058 ) ) ;
#24789 = CARTESIAN_POINT ( 'NONE',  ( 99.99999999999995737, 79.87500000273119838, -5.000000000000018652 ) ) ;
#24790 = CARTESIAN_POINT ( 'NONE',  ( 97.92893218813452449, 91.68749999999998579, 4.999999999999983125 ) ) ;
#24791 = CARTESIAN_POINT ( 'NONE',  ( 70.62287287157786864, 40.05742187716786873, -13.57481594606304753 ) ) ;
#24792 = CARTESIAN_POINT ( 'NONE',  ( 97.83688103937537051, 103.3426043859339103, -54.60000000000000853 ) ) ;
#24793 = CARTESIAN_POINT ( 'NONE',  ( 65.00000000000000000, 40.80156249999999574, -13.57481594606304576 ) ) ;
#24794 = CARTESIAN_POINT ( 'NONE',  ( -5.622872871577873077, 38.56914062716788294, -13.57481594606304753 ) ) ;
#24795 = VERTEX_POINT ( 'NONE', #6532 ) ;
#24796 =( BOUNDED_CURVE ( )  B_SPLINE_CURVE ( 2, ( #5540, #3113, #2691, #2961, #26637, #20504, #1544, #14751, #21336 ),
 .UNSPECIFIED., .F., .F. ) 
 B_SPLINE_CURVE_WITH_KNOTS ( ( 3, 2, 2, 2, 3 ),
 ( 0.1428571428571428492, 0.1517857142857142738, 0.1607142857142857539, 0.1696428571428571785, 0.1785714285714286031 ),
 .UNSPECIFIED. ) 
 CURVE ( )  GEOMETRIC_REPRESENTATION_ITEM ( )  RATIONAL_B_SPLINE_CURVE ( ( 1.000000000000000000, 0.9238795325112867385, 1.000000000000000000, 0.9238795325112867385, 1.000000000000000000, 0.9238795325112867385, 1.000000000000000000, 0.9238795325112865164, 1.000000000000000222 ) ) 
 REPRESENTATION_ITEM ( '' )  );
#24797 = CARTESIAN_POINT ( 'NONE',  ( 65.00000000000000000, 36.43593749999999432, 13.57481594606304576 ) ) ;
#24798 = CARTESIAN_POINT ( 'NONE',  ( 97.92893218813451028, 5.000000000000018652, 13.81250000000000000 ) ) ;
#24799 = EDGE_CURVE ( 'NONE', #19746, #2116, #17284, .T. ) ;
#24800 = EDGE_LOOP ( 'NONE', ( #2394, #10446 ) ) ;
#24801 = CARTESIAN_POINT ( 'NONE',  ( 13.14518615778179900, 34.84843750108393579, -5.444914386472297529 ) ) ;
#24802 = CARTESIAN_POINT ( 'NONE',  ( 185.7049497278729575, 39.66054687608393436, -9.295050272127046043 ) ) ;
#24803 = CARTESIAN_POINT ( 'NONE',  ( -13.14518615778179189, 34.25312500108393721, 5.444914386472304635 ) ) ;
#24804 = CARTESIAN_POINT ( 'NONE',  ( 102.0710678118654329, -4.999999999999989342, 13.43750000273118772 ) ) ;
#24805 = CARTESIAN_POINT ( 'NONE',  ( 99.99999999999995737, -4.999999999999990230, 3.249999999999999556 ) ) ;
#24806 = CARTESIAN_POINT ( 'NONE',  ( -5.444914386472297529, 32.66562500108393863, -13.14518615778179900 ) ) ;
#24807 = CARTESIAN_POINT ( 'NONE',  ( 143.1451861577818079, 32.26875000108393721, -5.444914386472297529 ) ) ;
#24808 = CARTESIAN_POINT ( 'NONE',  ( 99.99999999999998579, 91.56249999863440792, -4.458734124999994997 ) ) ;
#24809 = CARTESIAN_POINT ( 'NONE',  ( 99.99999999999998579, 123.7500000010924737, -2.066987299999998751 ) ) ;
#24810 = LINE ( 'NONE', #13678, #1382 ) ;
#24811 = CARTESIAN_POINT ( 'NONE',  ( 103.1528011352953342, -3.152801135295355106, 6.062500001365592084 ) ) ;
#24812 = CARTESIAN_POINT ( 'NONE',  ( 99.99999999999998579, 123.6000000000000085, 2.499999999999978684 ) ) ;
#24813 = AXIS2_PLACEMENT_3D ( 'NONE', #12739, #17310, #8483 ) ;
#24814 = CARTESIAN_POINT ( 'NONE',  ( 99.99999999999995737, 4.458734125000016313, 11.18750000136559208 ) ) ;
#24815 = CARTESIAN_POINT ( 'NONE',  ( 91.91746824999998466, 112.6261737610028320, -45.22500000273119980 ) ) ;
#24816 = CARTESIAN_POINT ( 'NONE',  ( 104.4587341249999923, 92.62499999863439371, -1.846868145590737198 ) ) ;
#24817 = DIRECTION ( 'NONE',  ( 0.000000000000000000, 1.000000000000000000, 0.000000000000000000 ) ) ;
#24818 = CARTESIAN_POINT ( 'NONE',  ( 102.2113248666666436, 122.4666666681233096, -9.811788309856265935E-15 ) ) ;
#24819 = CARTESIAN_POINT ( 'NONE',  ( 3.755638155860017591, 31.78804748261757140, -13.14518615778179367 ) ) ;
#24820 = ORIENTED_EDGE ( 'NONE', *, *, #4627, .T. ) ;
#24821 = CARTESIAN_POINT ( 'NONE',  ( 99.99999999999998579, 138.0000000000000000, 10.50000000000001066 ) ) ;
#24822 = ADVANCED_FACE ( 'NONE', ( #24349 ), #8816, .F. ) ;
#24823 = DIRECTION ( 'NONE',  ( 0.000000000000000000, 0.000000000000000000, 1.000000000000000000 ) ) ;
#24824 = CARTESIAN_POINT ( 'NONE',  ( 98.96446609406724804, 123.6500000021849672, 2.499999999999969802 ) ) ;
#24825 = CARTESIAN_POINT ( 'NONE',  ( 195.0000000000000000, 35.59257812608393579, -13.14518615778179544 ) ) ;
#24826 = VERTEX_POINT ( 'NONE', #20084 ) ;
#24827 = EDGE_CURVE ( 'NONE', #24826, #15121, #18218, .T. ) ;
#24828 = CARTESIAN_POINT ( 'NONE',  ( 193.1856446454109459, 51.46618445022109256, -15.00000000000000000 ) ) ;
#24829 = CARTESIAN_POINT ( 'NONE',  ( 104.4587341249999781, 1.846868145590750299, 12.25000000136559208 ) ) ;
#24830 = EDGE_CURVE ( 'NONE', #10007, #24596, #7468, .T. ) ;
#24831 = VERTEX_POINT ( 'NONE', #26355 ) ;
#24832 = CARTESIAN_POINT ( 'NONE',  ( 108.0825317500000153, 110.0000000000000000, -52.37500000273119838 ) ) ;
#24833 = CIRCLE ( 'NONE', #28005, 4.999999999999997335 ) ;
#24834 = CARTESIAN_POINT ( 'NONE',  ( 13.14518615778179900, 35.34453125108392868, 5.444914386472293977 ) ) ;
#24835 = LINE ( 'NONE', #25114, #7684 ) ;
#24836 = CARTESIAN_POINT ( 'NONE',  ( 9.180175813647991845, 50.00000000000000000, -9.999999999999998224 ) ) ;
#24837 = EDGE_CURVE ( 'NONE', #6267, #3669, #15109, .T. ) ;
#24838 = CARTESIAN_POINT ( 'NONE',  ( 143.1451861577818079, 38.61875000108393152, -5.444914386472297529 ) ) ;
#24839 = CARTESIAN_POINT ( 'NONE',  ( -13.14518615778179544, 36.78320312608393294, 0.000000000000000000 ) ) ;
#24840 = CARTESIAN_POINT ( 'NONE',  ( -9.295050272127046043, 34.89804687608393152, -9.295050272127046043 ) ) ;
#24842 = AXIS2_PLACEMENT_3D ( 'NONE', #25977, #26116, #6448 ) ;
#24841 = CARTESIAN_POINT ( 'NONE',  ( 98.15313185440925281, 92.87499999863440792, -4.458734124999994997 ) ) ;
#24843 = VECTOR ( 'NONE', #8258, 1000.000000000000000 ) ;
#24844 = CARTESIAN_POINT ( 'NONE',  ( 71.11775994554184877, 54.65941425414899157, -15.00000000000000000 ) ) ;
#24845 = CARTESIAN_POINT ( 'NONE',  ( 106.5389055433251002, 114.7507929638356785, -52.17500000273119554 ) ) ;
#24846 = EDGE_CURVE ( 'NONE', #20844, #9430, #13501, .T. ) ;
#24847 = VERTEX_POINT ( 'NONE', #12924 ) ;
#24848 = DIRECTION ( 'NONE',  ( -5.782411586589357392E-17, 0.000000000000000000, -1.000000000000000000 ) ) ;
#24849 = CARTESIAN_POINT ( 'NONE',  ( 5.444914386472297529, 34.94765625108394147, -13.14518615778179900 ) ) ;
#24850 = CARTESIAN_POINT ( 'NONE',  ( 99.99999999999995737, 4.458734125000016313, 7.437500001365592084 ) ) ;
#24851 = CARTESIAN_POINT ( 'NONE',  ( 74.29505027212704249, 38.66835937608393436, -9.295050272127046043 ) ) ;
#24852 = CARTESIAN_POINT ( 'NONE',  ( 106.9999999999999716, 1.473504056721760595E-14, 15.00000000000000000 ) ) ;
#24853 = CARTESIAN_POINT ( 'NONE',  ( 104.9999999999999574, -2.071067811865468844, 14.43749999999999645 ) ) ;
#24854 = CARTESIAN_POINT ( 'NONE',  ( -13.14518615778179722, 34.35234375108393579, -5.444914386472297529 ) ) ;
#24855 = CARTESIAN_POINT ( 'NONE',  ( 102.4999999999999716, 123.1500000021849672, -1.035533905932742638 ) ) ;
#24856 = CARTESIAN_POINT ( 'NONE',  ( 97.50000000000000000, 125.0000000000000000, -9.540979117872439019E-15 ) ) ;
#24857 = CARTESIAN_POINT ( 'NONE',  ( 181.8548138422182205, 39.11484375108393863, -5.444914386472297529 ) ) ;
#24858 = CARTESIAN_POINT ( 'NONE',  ( 99.99999999999997158, 118.4984768113314004, -52.37499999726880873 ) ) ;
#24859 = CARTESIAN_POINT ( 'NONE',  ( 5.622872871577878406, 34.89804687499999147, 13.57481594606304576 ) ) ;
#24860 = CARTESIAN_POINT ( 'NONE',  ( 5.444914386472297529, 35.54296875108393294, -13.14518615778179900 ) ) ;
#24861 = VECTOR ( 'NONE', #23624, 1000.000000000000000 ) ;
#24862 = ORIENTED_EDGE ( 'NONE', *, *, #1482, .T. ) ;
#24863 = CARTESIAN_POINT ( 'NONE',  ( 135.4449143864723055, 33.85625000108393579, 13.14518615778179189 ) ) ;
#24864 = CARTESIAN_POINT ( 'NONE',  ( 51.85481384221821344, 40.00781250108393294, 5.444914386472304635 ) ) ;
#24865 = DIRECTION ( 'NONE',  ( -0.000000000000000000, -0.000000000000000000, -1.000000000000000000 ) ) ;
#24866 = CARTESIAN_POINT ( 'NONE',  ( 208.1451861577817795, 33.95546875108393436, 5.444914386472293977 ) ) ;
#24867 = ORIENTED_EDGE ( 'NONE', *, *, #16054, .T. ) ;
#24868 = CARTESIAN_POINT ( 'NONE',  ( 102.0669872999999797, 124.1500000010924794, -9.794112055954760458E-15 ) ) ;
#24869 = DIRECTION ( 'NONE',  ( -0.000000000000000000, 1.000000000000000000, -0.000000000000000000 ) ) ;
#24870 = EDGE_CURVE ( 'NONE', #25247, #11161, #21656, .T. ) ;
#24871 = CARTESIAN_POINT ( 'NONE',  ( 124.3771271284221314, 37.77539062716788010, -13.57481594606304753 ) ) ;
#24872 = CARTESIAN_POINT ( 'NONE',  ( 102.4976396683250925, 102.3130555110000159, -48.52500000273119696 ) ) ;
#24873 =( BOUNDED_CURVE ( )  B_SPLINE_CURVE ( 2, ( #607, #24824, #3165, #22408, #13970, #751, #3020, #22271, #4885 ),
 .UNSPECIFIED., .F., .T. ) 
 B_SPLINE_CURVE_WITH_KNOTS ( ( 3, 2, 2, 2, 3 ),
 ( 0.2500000000000004441, 0.2916666666666670182, 0.3333333333333334814, 0.3750000000000000555, 0.4166666666666666297 ),
 .UNSPECIFIED. ) 
 CURVE ( )  GEOMETRIC_REPRESENTATION_ITEM ( )  RATIONAL_B_SPLINE_CURVE ( ( 0.9999999999999992228, 0.9238795325112875156, 1.000000000000000000, 0.9238795325112867385, 1.000000000000000000, 0.9238795325112867385, 1.000000000000000000, 0.9238795325112868495, 0.9999999999999998890 ) ) 
 REPRESENTATION_ITEM ( '' )  );
#24874 = AXIS2_PLACEMENT_3D ( 'NONE', #16423, #9729, #11854 ) ;
#24875 = CARTESIAN_POINT ( 'NONE',  ( 102.0710678118654471, 90.18749999999997158, -5.000000000000000000 ) ) ;
#24876 = CARTESIAN_POINT ( 'NONE',  ( 104.9999999999999716, 1.449011120738813565E-14, 34.79898987322334136 ) ) ;
#24877 = CARTESIAN_POINT ( 'NONE',  ( 74.18017581364802027, 49.99999999999999289, 14.99999999999997513 ) ) ;
#24878 = ORIENTED_EDGE ( 'NONE', *, *, #12640, .F. ) ;
#24879 = ORIENTED_EDGE ( 'NONE', *, *, #470, .F. ) ;
#24880 = CARTESIAN_POINT ( 'NONE',  ( 103.1528011352953342, 3.152801135295383084, 5.062500001365592972 ) ) ;
#24881 = EDGE_LOOP ( 'NONE', ( #22559, #3509 ) ) ;
#24882 = CARTESIAN_POINT ( 'NONE',  ( -13.57481594606304398, 35.59257812716789715, 5.622872871577880183 ) ) ;
#24883 = CARTESIAN_POINT ( 'NONE',  ( 96.84719886470459471, 3.152801135295383084, 8.312500001365592084 ) ) ;
#24884 = CARTESIAN_POINT ( 'NONE',  ( 136.1198436276953032, 51.28708186915216771, 14.99999999999926992 ) ) ;
#24885 = CARTESIAN_POINT ( 'NONE',  ( -13.09590655363597733, 36.00000000000000000, 1.137167824541468031 ) ) ;
#24886 = CARTESIAN_POINT ( 'NONE',  ( 65.00000000000000000, 37.72578125216787726, -13.57481594606304576 ) ) ;
#24887 = CARTESIAN_POINT ( 'NONE',  ( 104.9999999999999716, 1.449011120738813565E-14, 5.500000000000000000 ) ) ;
#24888 = CARTESIAN_POINT ( 'NONE',  ( 93.46109445667491400, 105.2492070361643215, -46.92500000273119554 ) ) ;
#24889 = CARTESIAN_POINT ( 'NONE',  ( 96.46446609406721961, 81.12500000000000000, 3.535533905932727539 ) ) ;
#24890 = CARTESIAN_POINT ( 'NONE',  ( 114.9999999999999858, 120.0000000000000000, -45.00000000000000711 ) ) ;
#24891 = CARTESIAN_POINT ( 'NONE',  ( 3.803054373245578823, 54.09082899096177499, 14.99999999999999645 ) ) ;
#24892 = DIRECTION ( 'NONE',  ( -0.000000000000000000, 1.000000000000000000, -0.000000000000000000 ) ) ;
#24893 = CARTESIAN_POINT ( 'NONE',  ( 135.6228728715778686, 34.40195312499999858, -13.57481594606304753 ) ) ;
#24894 = ORIENTED_EDGE ( 'NONE', *, *, #25008, .T. ) ;
#24895 = DIRECTION ( 'NONE',  ( 1.156482317317871478E-16, 0.000000000000000000, 1.000000000000000000 ) ) ;
#24896 = CARTESIAN_POINT ( 'NONE',  ( -9.295050272127044266, 33.70742187608393436, 9.295050272127047819 ) ) ;
#24897 = CARTESIAN_POINT ( 'NONE',  ( -5.622872871577873077, 34.10429687716786873, 13.57481594606304753 ) ) ;
#24898 = AXIS2_PLACEMENT_3D ( 'NONE', #8324, #23309, #10306 ) ;
#24899 = CARTESIAN_POINT ( 'NONE',  ( 99.99999999999995737, -4.999999999999990230, 6.375000002731185944 ) ) ;
#24900 = CARTESIAN_POINT ( 'NONE',  ( 139.2950502721270425, 32.11992187608393579, 9.295050272127046043 ) ) ;
#24901 = CARTESIAN_POINT ( 'NONE',  ( 65.00000000000000000, 39.16445312608392726, 13.14518615778179544 ) ) ;
#24902 = CARTESIAN_POINT ( 'NONE',  ( -8.312177448680279460E-16, 32.07031249999999289, -13.57481594606304576 ) ) ;
#24903 = CARTESIAN_POINT ( 'NONE',  ( 5.444914386472302859, 40.00781250108393294, 13.14518615778179189 ) ) ;
#24904 = CARTESIAN_POINT ( 'NONE',  ( 94.99999999999995737, 1.387778780781445676E-14, 11.00000000000000000 ) ) ;
#24905 = CARTESIAN_POINT ( 'NONE',  ( 7.171391216998964424, 31.99955315621561525, -11.52591757658528948 ) ) ;
#24906 = DIRECTION ( 'NONE',  ( 0.000000000000000000, 0.000000000000000000, -1.000000000000000000 ) ) ;
#24907 = CARTESIAN_POINT ( 'NONE',  ( 2.493653234604083739E-15, 38.12265625216787157, 13.57481594606304576 ) ) ;
#24908 = DIRECTION ( 'NONE',  ( 0.000000000000000000, 0.000000000000000000, 1.000000000000000000 ) ) ;
#24909 = CARTESIAN_POINT ( 'NONE',  ( -8.312177448680279460E-16, 32.96328125216787441, -13.57481594606304576 ) ) ;
#24910 = CARTESIAN_POINT ( 'NONE',  ( 99.14382582708707048, 123.1000000010924822, 2.066987299999979211 ) ) ;
#24911 = CARTESIAN_POINT ( 'NONE',  ( 123.5294363033336822, 36.00000000000001421, -11.78199955157030487 ) ) ;
#24912 = DIRECTION ( 'NONE',  ( -1.000000000000000000, 0.000000000000000000, 0.000000000000000000 ) ) ;
#24913 = LINE ( 'NONE', #5252, #5136 ) ;
#24914 = CARTESIAN_POINT ( 'NONE',  ( 13.57481594606304753, 34.30273437500000000, -5.622872871577873077 ) ) ;
#24915 = CARTESIAN_POINT ( 'NONE',  ( -5.444914386472299306, 34.55078125108393294, 13.14518615778179722 ) ) ;
#24916 = CARTESIAN_POINT ( 'NONE',  ( -9.295050272127044266, 31.92148437608393508, 9.295050272127047819 ) ) ;
#24917 = CARTESIAN_POINT ( 'NONE',  ( 195.0000000000000000, 32.46718749999999432, 13.57481594606304576 ) ) ;
#24918 = CARTESIAN_POINT ( 'NONE',  ( 13.57481594606304753, 37.57695312716787583, -5.622872871577873077 ) ) ;
#24919 = CARTESIAN_POINT ( 'NONE',  ( 9.598844408820459861, 37.42812500216787441, 9.598844408820456309 ) ) ;
#24920 = CARTESIAN_POINT ( 'NONE',  ( -5.622872871578057818, 35.59257812499998863, 13.57481594606286457 ) ) ;
#24921 = CARTESIAN_POINT ( 'NONE',  ( 78.14518615778179367, 33.06250000108393294, -5.444914386472297529 ) ) ;
#24922 = DIRECTION ( 'NONE',  ( -0.000000000000000000, -1.000000000000000000, -0.000000000000000000 ) ) ;
#24923 = LINE ( 'NONE', #14077, #471 ) ;
#24924 = CARTESIAN_POINT ( 'NONE',  ( 100.8561741729129295, 124.0000000010925021, 2.066987299999979211 ) ) ;
#24925 = FACE_OUTER_BOUND ( 'NONE', #533, .T. ) ;
#24926 = CARTESIAN_POINT ( 'NONE',  ( 99.99999999999997158, 118.4984768113314004, -52.37499999726880873 ) ) ;
#24927 = CARTESIAN_POINT ( 'NONE',  ( 143.1451861577818079, 34.84843750108393579, -5.444914386472297529 ) ) ;
#24928 = ORIENTED_EDGE ( 'NONE', *, *, #850, .T. ) ;
#24929 = CARTESIAN_POINT ( 'NONE',  ( 102.0710678118654329, 80.31250000000000000, 4.999999999999989342 ) ) ;
#24930 = CARTESIAN_POINT ( 'NONE',  ( 99.99999999999998579, 92.75000000000000000, 4.999999999999984013 ) ) ;
#24931 = CARTESIAN_POINT ( 'NONE',  ( 99.99999999999995737, 82.18750000136559208, -4.458734125000016313 ) ) ;
#24932 = CARTESIAN_POINT ( 'NONE',  ( 95.00000000000000000, 93.43750000000001421, -2.071067811865479058 ) ) ;
#24933 = CARTESIAN_POINT ( 'NONE',  ( 65.00000000000000000, 36.00000000000000000, 11.57481594606303688 ) ) ;
#24934 = CARTESIAN_POINT ( 'NONE',  ( 105.6631189606246153, 114.1144967660473242, -53.80000000000001137 ) ) ;
#24935 = CARTESIAN_POINT ( 'NONE',  ( 181.8548138422182205, 40.75195312608393294, 0.000000000000000000 ) ) ;
#24936 = CARTESIAN_POINT ( 'NONE',  ( -9.598844408820458085, 38.61875000216787157, -9.598844408820458085 ) ) ;
#24937 = EDGE_LOOP ( 'NONE', ( #24217, #9029, #6136, #11695 ) ) ;
#24938 = VECTOR ( 'NONE', #4642, 1000.000000000000000 ) ;
#24939 = CARTESIAN_POINT ( 'NONE',  ( 96.46446609406721961, -3.535533905932727539, 8.125000000000000000 ) ) ;
#24940 = ORIENTED_EDGE ( 'NONE', *, *, #6691, .T. ) ;
#24941 = CARTESIAN_POINT ( 'NONE',  ( -9.295050272127044266, 37.67617187608393436, 9.295050272127047819 ) ) ;
#24942 = CARTESIAN_POINT ( 'NONE',  ( 181.8548138422181921, 39.71015625108393010, -5.444914386472297529 ) ) ;
#24943 = CARTESIAN_POINT ( 'NONE',  ( 9.295050272127047819, 34.50117187608393010, 9.295050272127046043 ) ) ;
#24944 = CARTESIAN_POINT ( 'NONE',  ( 99.99999999999995737, -4.999999999999990230, 12.37500000273118594 ) ) ;
#24945 = CARTESIAN_POINT ( 'NONE',  ( 130.0000000000000000, 39.95820312608393010, 13.14518615778179544 ) ) ;
#24946 = CARTESIAN_POINT ( 'NONE',  ( -9.295050272127044266, 32.91367187608393152, 9.295050272127047819 ) ) ;
#24947 = CARTESIAN_POINT ( 'NONE',  ( 94.33688103937537051, 105.8855032339526758, -50.30000000546237970 ) ) ;
#24948 = CARTESIAN_POINT ( 'NONE',  ( 101.8468681455907330, 90.49999999863440792, -4.458734124999994997 ) ) ;
#24949 = CARTESIAN_POINT ( 'NONE',  ( 101.0355339059327378, 123.9500000000000028, -2.499999999999997780 ) ) ;
#24950 = PRODUCT_RELATED_PRODUCT_CATEGORY ( 'part', '', ( #12815 ) ) ;
#24951 = CARTESIAN_POINT ( 'NONE',  ( 195.0000000000000000, 50.00000000000000000, 13.57481594606302266 ) ) ;
#24952 = CARTESIAN_POINT ( 'NONE',  ( 103.1528011352953342, -3.152801135295355106, 8.062500001365592084 ) ) ;
#24953 = CARTESIAN_POINT ( 'NONE',  ( 97.93301270000000613, 124.5500000010924850, -9.540979117872439019E-15 ) ) ;
#24954 = EDGE_CURVE ( 'NONE', #26438, #25848, #19510, .T. ) ;
#24955 = CARTESIAN_POINT ( 'NONE',  ( 98.15313185440923860, 4.458734125000016313, 9.250000001365592084 ) ) ;
#24956 = CARTESIAN_POINT ( 'NONE',  ( 107.0000000000000142, 110.0000000000000000, -49.50000000546238255 ) ) ;
#24957 = CARTESIAN_POINT ( 'NONE',  ( 101.8468681455907330, 91.37499999863439371, 4.458734124999979898 ) ) ;
#24958 = CARTESIAN_POINT ( 'NONE',  ( 9.598844408820456309, 39.90859374999999432, -9.598844408820458085 ) ) ;
#24959 = LINE ( 'NONE', #5445, #14800 ) ;
#24960 = CARTESIAN_POINT ( 'NONE',  ( -13.14518615778179544, 32.81445312608393294, 0.000000000000000000 ) ) ;
#24961 = CIRCLE ( 'NONE', #11749, 13.57481594606304398 ) ;
#24962 = ORIENTED_EDGE ( 'NONE', *, *, #19448, .T. ) ;
#24963 = DIRECTION ( 'NONE',  ( 0.000000000000000000, 0.000000000000000000, 1.000000000000000000 ) ) ;
#24964 =( BOUNDED_CURVE ( )  B_SPLINE_CURVE ( 2, ( #2781, #7613, #791, #935, #15731, #5202, #4922, #13867, #13585, #27015, #22306, #22593, #27161, #7462, #16157, #24864, #22734, #3200, #11871, #1076, #12424, #1490, #3480, #23289, #25559, #1629, #20869, #18996, #1353, #5627, #3625, #21430, #6039, #27567, #25275, #12705, #14433, #23149, #5764, #1767, #16991, #25690, #12286, #21142, #19141, #8302, #7888, #21010, #23009, #10433, #10018, #21285, #16725, #5906, #3897, #10289, #27846, #27296, #18591, #6174, #14841, #27705, #12559, #18857, #8169, #23423, #3763, #8027, #23563, #14705, #10145, #4041, #14572, #9883, #16860, #18727, #25422, #7753, #12145, #16440, #25137, #14293, #27425, #16583, #15262, #17416, #2328, #23981, #8724, #17557, #5133, #8865, #28119, #13799, #21852, #1910, #6721 ),
 .UNSPECIFIED., .F., .F. ) 
 B_SPLINE_CURVE_WITH_KNOTS ( ( 3, 2, 2, 2, 2, 2, 2, 2, 2, 2, 2, 2, 2, 2, 2, 2, 2, 2, 2, 2, 2, 2, 2, 2, 2, 2, 2, 2, 2, 2, 2, 2, 2, 2, 2, 2, 2, 2, 2, 2, 2, 2, 2, 2, 2, 2, 2, 2, 3 ),
 ( 0.000000000000000000, 0.01041666666666666609, 0.02083333333333333218, 0.03125000000000000000, 0.04166666666666666435, 0.05208333333333333565, 0.06250000000000000000, 0.07291666666666667129, 0.08333333333333332871, 0.09374999999999998612, 0.1041666666666666713, 0.1145833333333333287, 0.1250000000000000000, 0.1354166666666666574, 0.1458333333333333426, 0.1562500000000000000, 0.1666666666666666574, 0.1770833333333333426, 0.1874999999999999722, 0.1979166666666666574, 0.2083333333333333426, 0.2187500000000000000, 0.2291666666666666574, 0.2395833333333333426, 0.2500000000000000000, 0.2604166666666666852, 0.2708333333333333148, 0.2812500000000000000, 0.2916666666666666852, 0.3020833333333333148, 0.3125000000000000000, 0.3229166666666666852, 0.3333333333333333148, 0.3437500000000000000, 0.3541666666666666852, 0.3645833333333333148, 0.3749999999999999445, 0.3854166666666666852, 0.3958333333333333148, 0.4062500000000000000, 0.4166666666666666852, 0.4270833333333333148, 0.4375000000000000000, 0.4479166666666666852, 0.4583333333333333148, 0.4687500000000000000, 0.4791666666666666852, 0.4895833333333333148, 0.4988304892921909817 ),
 .UNSPECIFIED. ) 
 CURVE ( )  GEOMETRIC_REPRESENTATION_ITEM ( )  RATIONAL_B_SPLINE_CURVE ( ( 1.000000000000000000, 0.9238795325112867385, 1.000000000000000000, 0.9238795325112867385, 1.000000000000000000, 0.9238795325112867385, 1.000000000000000000, 0.9238795325112867385, 1.000000000000000000, 0.9238795325112867385, 1.000000000000000000, 0.9238795325112867385, 1.000000000000000000, 0.9238795325112867385, 1.000000000000000000, 0.9238795325112867385, 1.000000000000000000, 0.9238795325112867385, 1.000000000000000000, 0.9238795325112867385, 1.000000000000000000, 0.9238795325112867385, 1.000000000000000000, 0.9238795325112867385, 1.000000000000000000, 0.9238795325112867385, 1.000000000000000000, 0.9238795325112867385, 1.000000000000000000, 0.9238795325112867385, 1.000000000000000000, 0.9238795325112867385, 1.000000000000000000, 0.9238795325112867385, 1.000000000000000000, 0.9238795325112867385, 1.000000000000000000, 0.9238795325112867385, 1.000000000000000000, 0.9238795325112867385, 1.000000000000000000, 0.9238795325112867385, 1.000000000000000000, 0.9238795325112867385, 1.000000000000000000, 0.9238795325112867385, 1.000000000000000000, 0.9238795325112867385, 1.000000000000000000, 0.9238795325112867385, 1.000000000000000000, 0.9238795325112867385, 1.000000000000000000, 0.9238795325112867385, 1.000000000000000000, 0.9238795325112867385, 1.000000000000000000, 0.9238795325112867385, 1.000000000000000000, 0.9238795325112867385, 1.000000000000000000, 0.9238795325112867385, 1.000000000000000000, 0.9238795325112867385, 1.000000000000000000, 0.9238795325112867385, 1.000000000000000000, 0.9238795325112867385, 1.000000000000000000, 0.9238795325112867385, 1.000000000000000000, 0.9238795325112867385, 1.000000000000000000, 0.9238795325112867385, 1.000000000000000000, 0.9238795325112867385, 1.000000000000000000, 0.9238795325112867385, 1.000000000000000000, 0.9238795325112867385, 1.000000000000000000, 0.9238795325112867385, 1.000000000000000000, 0.9238795325112867385, 1.000000000000000000, 0.9238795325112867385, 1.000000000000000000, 0.9238795325112867385, 1.000000000000000000, 0.9238795325112867385, 1.000000000000000000, 0.9238795325112867385, 1.000000000000000000, 0.9238795325112867385, 1.000000000000000000, 0.9324258078851886955, 0.9848264816800353927 ) ) 
 REPRESENTATION_ITEM ( '' )  );
#24965 = CARTESIAN_POINT ( 'NONE',  ( 104.9999999999999716, 1.449011120738813565E-14, 2.499999999999998668 ) ) ;
#24966 = CARTESIAN_POINT ( 'NONE',  ( 204.2950502721270425, 33.11210937608393579, -9.295050272127046043 ) ) ;
#24967 = VERTEX_POINT ( 'NONE', #20513 ) ;
#24968 = CARTESIAN_POINT ( 'NONE',  ( 187.9105827276678156, 49.99999999943695173, -11.59823041029156165 ) ) ;
#24969 = CARTESIAN_POINT ( 'NONE',  ( 96.84719886470459471, -3.152801135295355994, 12.81250000136559208 ) ) ;
#24970 = ORIENTED_EDGE ( 'NONE', *, *, #1505, .T. ) ;
#24971 = CARTESIAN_POINT ( 'NONE',  ( 91.91746824999998466, 112.6261737610028320, -45.47500000273119980 ) ) ;
#24972 = CARTESIAN_POINT ( 'NONE',  ( 13.14518615778179544, 36.18789062608393436, -1.609821015232357215E-15 ) ) ;
#24973 = DIRECTION ( 'NONE',  ( -0.000000000000000000, 1.000000000000000000, -0.000000000000000000 ) ) ;
#24974 = CARTESIAN_POINT ( 'NONE',  ( 5.622872871577912157, 38.86679687500001279, 13.57481594606301023 ) ) ;
#24975 = VECTOR ( 'NONE', #17474, 1000.000000000000000 ) ;
#24976 = AXIS2_PLACEMENT_3D ( 'NONE', #15557, #9292, #17989 ) ;
#24977 = CARTESIAN_POINT ( 'NONE',  ( 130.0000000000000000, 38.76757812608393294, -13.14518615778179544 ) ) ;
#24978 = CARTESIAN_POINT ( 'NONE',  ( -13.14518615778179189, 37.62656250108393152, 5.444914386472304635 ) ) ;
#24979 = CARTESIAN_POINT ( 'NONE',  ( 2.414731522848535132E-15, 32.81445312608393294, 13.14518615778179544 ) ) ;
#24980 = EDGE_CURVE ( 'NONE', #4858, #8561, #2407, .T. ) ;
#24981 = CIRCLE ( 'NONE', #404, 11.57481594606304398 ) ;
#24982 = CARTESIAN_POINT ( 'NONE',  ( 104.4587341249999923, 92.62499999863439371, -1.846868145590737198 ) ) ;
#24983 = DIRECTION ( 'NONE',  ( -2.674902700537828060E-32, 1.000000000000000000, -4.625929269271485914E-16 ) ) ;
#24984 = CARTESIAN_POINT ( 'NONE',  ( 91.91746824999998466, 107.3738262389971680, -49.27500000273118985 ) ) ;
#24985 = CARTESIAN_POINT ( 'NONE',  ( 13.57481594606304753, 38.37070312716787157, -5.622872871577873966 ) ) ;
#24986 = CARTESIAN_POINT ( 'NONE',  ( -9.295050272127046043, 32.71523437608393436, -9.295050272127046043 ) ) ;
#24987 = CARTESIAN_POINT ( 'NONE',  ( 95.54126587499996504, -1.846868145590724986, 6.750000001365592084 ) ) ;
#24988 = EDGE_CURVE ( 'NONE', #21956, #34, #8550, .T. ) ;
#24989 = CARTESIAN_POINT ( 'NONE',  ( 99.99999999999995737, 83.43750000136560629, -4.458734125000016313 ) ) ;
#24990 = CARTESIAN_POINT ( 'NONE',  ( -9.598844408820458085, 38.61875000216787157, -9.598844408820458085 ) ) ;
#24991 = DIRECTION ( 'NONE',  ( -1.000000000000000000, 0.000000000000000000, 0.000000000000000000 ) ) ;
#24992 = CARTESIAN_POINT ( 'NONE',  ( 208.1451861577818079, 37.03125000108393294, -5.444914386472297529 ) ) ;
#24993 = EDGE_LOOP ( 'NONE', ( #23672, #8398, #14996, #23351 ) ) ;
#24994 = EDGE_CURVE ( 'NONE', #4636, #25739, #1136, .T. ) ;
#24995 = CARTESIAN_POINT ( 'NONE',  ( -9.295050272127044266, 36.08867187608393579, 9.295050272127047819 ) ) ;
#24996 = CARTESIAN_POINT ( 'NONE',  ( 100.8561741729129295, 124.0000000010925021, 2.066987299999979211 ) ) ;
#24997 = DIRECTION ( 'NONE',  ( -0.000000000000000000, -1.000000000000000000, -0.000000000000000000 ) ) ;
#24998 = DIRECTION ( 'NONE',  ( -0.000000000000000000, 1.000000000000000000, -0.000000000000000000 ) ) ;
#24999 = CARTESIAN_POINT ( 'NONE',  ( 97.50236033167490746, 117.6869444889999841, -48.27499999726882152 ) ) ;
#25000 = CARTESIAN_POINT ( 'NONE',  ( 13.57481594606304931, 32.61601562499999574, 5.622872871577869525 ) ) ;
#25001 = CARTESIAN_POINT ( 'NONE',  ( 5.444914386472302859, 34.45156250108393436, 13.14518615778179189 ) ) ;
#25002 = ORIENTED_EDGE ( 'NONE', *, *, #19217, .F. ) ;
#25003 = PLANE ( 'NONE',  #18428 ) ;
#25004 = CARTESIAN_POINT ( 'NONE',  ( 68.75563826565991121, 31.58960998161716560, -13.14518615778179900 ) ) ;
#25005 = PRESENTATION_LAYER_ASSIGNMENT (  '', '', ( #1354 ) ) ;
#25006 = ORIENTED_EDGE ( 'NONE', *, *, #8987, .F. ) ;
#25007 = CARTESIAN_POINT ( 'NONE',  ( 9.598844408820456309, 32.86406250216787583, -9.598844408820458085 ) ) ;
#25008 = EDGE_CURVE ( 'NONE', #9430, #7349, #22652, .T. ) ;
#25009 = CARTESIAN_POINT ( 'NONE',  ( 204.2950502721270425, 34.10429687608393579, -9.295050272127046043 ) ) ;
#25010 =( BOUNDED_CURVE ( )  B_SPLINE_CURVE ( 2, ( #9053, #2920, #24440, #4781, #9190, #26881, #3068, #22168, #2646 ),
 .UNSPECIFIED., .F., .T. ) 
 B_SPLINE_CURVE_WITH_KNOTS ( ( 3, 2, 2, 2, 3 ),
 ( 0.08333333333333307891, 0.1249999999999999167, 0.1666666666666667407, 0.2083333333333335924, 0.2500000000000004441 ),
 .UNSPECIFIED. ) 
 CURVE ( )  GEOMETRIC_REPRESENTATION_ITEM ( )  RATIONAL_B_SPLINE_CURVE ( ( 1.000000000000000444, 0.9238795325112862944, 1.000000000000000000, 0.9238795325112867385, 1.000000000000000000, 0.9238795325112867385, 1.000000000000000000, 0.9238795325112859613, 1.000000000000000888 ) ) 
 REPRESENTATION_ITEM ( '' )  );
#25011 = ORIENTED_EDGE ( 'NONE', *, *, #4466, .F. ) ;
#25012 = CARTESIAN_POINT ( 'NONE',  ( 96.46446609406721961, 3.535533905932755072, 2.000000002731185056 ) ) ;
#25013 = CARTESIAN_POINT ( 'NONE',  ( 96.46446609406726225, 91.24999999726880162, -3.535533905932738197 ) ) ;
#25014 = CARTESIAN_POINT ( 'NONE',  ( 95.27063293749995410, 79.84375000068280315, -1.387778780781445676E-14 ) ) ;
#25015 = CARTESIAN_POINT ( 'NONE',  ( 116.4251840539369596, 37.13046875216787868, 0.000000000000000000 ) ) ;
#25016 = DIRECTION ( 'NONE',  ( 0.000000000000000000, 0.000000000000000000, 1.000000000000000000 ) ) ;
#25017 = CARTESIAN_POINT ( 'NONE',  ( 97.83688103937535629, 116.6573956140660897, -46.89999999453763735 ) ) ;
#25018 = CARTESIAN_POINT ( 'NONE',  ( 195.0000000000000000, 38.17226562608394147, -13.14518615778179544 ) ) ;
#25019 = ADVANCED_FACE ( 'NONE', ( #20368 ), #15273, .T. ) ;
#25020 = ORIENTED_EDGE ( 'NONE', *, *, #27599, .F. ) ;
#25021 = CARTESIAN_POINT ( 'NONE',  ( 104.4587341249999639, 1.442382525525748735E-14, 13.18750000136559208 ) ) ;
#25022 = CARTESIAN_POINT ( 'NONE',  ( 120.8198241863519939, 55.00000000000000000, -15.00000000000000000 ) ) ;
#25023 = DIRECTION ( 'NONE',  ( 0.000000000000000000, 0.000000000000000000, 1.000000000000000000 ) ) ;
#25024 = CARTESIAN_POINT ( 'NONE',  ( -1.021803718759902280, 36.00000000000000711, 13.11239906893438878 ) ) ;
#25025 = CARTESIAN_POINT ( 'NONE',  ( 70.44491438647230552, 33.36015625108393579, -13.14518615778179900 ) ) ;
#25026 = FILL_AREA_STYLE ('',( #25156 ) ) ;
#25027 = CARTESIAN_POINT ( 'NONE',  ( -13.14518615778179189, 39.21406250108392300, 5.444914386472304635 ) ) ;
#25028 = DIRECTION ( 'NONE',  ( 0.000000000000000000, 0.000000000000000000, 1.000000000000000000 ) ) ;
#25029 = CARTESIAN_POINT ( 'NONE',  ( 1.662435489736055498E-15, -7.395377635281828788, -13.57481594606304398 ) ) ;
#25030 = CARTESIAN_POINT ( 'NONE',  ( 0.7238719380229381439, 53.51529642094862993, 14.99999999999999645 ) ) ;
#25031 = CARTESIAN_POINT ( 'NONE',  ( 124.3771271284221314, 33.70742187500000142, -13.57481594606304753 ) ) ;
#25032 = ADVANCED_FACE ( 'NONE', ( #4656 ), #22043, .F. ) ;
#25033 = AXIS2_PLACEMENT_3D ( 'NONE', #21280, #12279, #22866 ) ;
#25034 = EDGE_LOOP ( 'NONE', ( #11000, #24393, #24862, #9143, #16484, #17272, #20809, #1146, #21625, #374, #8147, #23701, #7986, #3538, #26084, #21774, #21338, #15511, #27538, #10312, #15383, #10065, #9688, #4628, #433, #21321, #20737, #3304, #26454, #11305, #18659 ) ) ;
#25035 = CARTESIAN_POINT ( 'NONE',  ( 107.0000000000000000, 110.0000000000000000, -145.0000000000000284 ) ) ;
#25036 = CARTESIAN_POINT ( 'NONE',  ( 5.444914386472302859, 32.26875000108393721, 13.14518615778179189 ) ) ;
#25037 = CARTESIAN_POINT ( 'NONE',  ( -9.598844408820458085, 35.44375000216787441, -9.598844408820458085 ) ) ;
#25038 = CARTESIAN_POINT ( 'NONE',  ( 103.5355339059327093, 3.535533905932755072, 4.750000002731185944 ) ) ;
#25039 = CARTESIAN_POINT ( 'NONE',  ( 124.5550856135277087, 31.67343750108393863, -13.14518615778179900 ) ) ;
#25040 = CARTESIAN_POINT ( 'NONE',  ( 55.40115559117954547, 32.26875000216787726, -9.598844408820458085 ) ) ;
#25041 = CARTESIAN_POINT ( 'NONE',  ( 59.37712712842213136, 36.98164062716787015, -13.57481594606304753 ) ) ;
#25042 = CARTESIAN_POINT ( 'NONE',  ( -13.14518615778179544, 37.37851562608393863, 0.000000000000000000 ) ) ;
#25043 = CARTESIAN_POINT ( 'NONE',  ( -5.444914386472299306, 33.75703125108393721, 13.14518615778179722 ) ) ;
#25044 = CARTESIAN_POINT ( 'NONE',  ( 84.99999999999998579, 0.000000000000000000, 8.673617379884035472E-16 ) ) ;
#25045 = CARTESIAN_POINT ( 'NONE',  ( 102.4976396683250783, 102.3130555110000159, -55.27499999726882152 ) ) ;
#25046 = AXIS2_PLACEMENT_3D ( 'NONE', #7662, #6535, #6128 ) ;
#25047 = FILL_AREA_STYLE_COLOUR ( '', #6611 ) ;
#25048 = CARTESIAN_POINT ( 'NONE',  ( 181.8548138422181921, 31.87187500108393223, 5.444914386472304635 ) ) ;
#25049 = CARTESIAN_POINT ( 'NONE',  ( 98.23223304703363112, 124.2999999999999972, 1.767766952966351557 ) ) ;
#25050 = CARTESIAN_POINT ( 'NONE',  ( 98.96446609406727646, 124.8569999999781714, -2.499999999999997780 ) ) ;
#25051 = CARTESIAN_POINT ( 'NONE',  ( 102.0669872999999939, 123.4000000010924936, -0.8561741729129507261 ) ) ;
#25052 = CARTESIAN_POINT ( 'NONE',  ( 95.67376207875072680, 115.9545556584642867, -50.79999999453763593 ) ) ;
#25053 = LINE ( 'NONE', #27345, #16330 ) ;
#25054 = LINE ( 'NONE', #2827, #4680 ) ;
#25055 = CARTESIAN_POINT ( 'NONE',  ( -8.312177448680279460E-16, 34.45156249999999432, -13.57481594606304576 ) ) ;
#25056 = ORIENTED_EDGE ( 'NONE', *, *, #20365, .F. ) ;
#25057 = CARTESIAN_POINT ( 'NONE',  ( -9.839381608887936892, 36.00000000000000711, -9.004033604613056241 ) ) ;
#25058 = CARTESIAN_POINT ( 'NONE',  ( 2.493653234604083739E-15, 39.61093749999999147, 13.57481594606304576 ) ) ;
#25059 = CARTESIAN_POINT ( 'NONE',  ( 9.295050272127047819, 34.50117187608393010, 9.295050272127046043 ) ) ;
#25060 = CARTESIAN_POINT ( 'NONE',  ( -9.295050272127046043, 34.10429687608393579, -9.295050272127046043 ) ) ;
#25061 = EDGE_CURVE ( 'NONE', #20470, #12415, #4514, .T. ) ;
#25062 = CARTESIAN_POINT ( 'NONE',  ( -13.57481594606304753, 33.90585937716787868, -5.622872871577873077 ) ) ;
#25063 = DIRECTION ( 'NONE',  ( 1.000000000000000000, 0.000000000000000000, -5.782411586589357392E-17 ) ) ;
#25064 = CARTESIAN_POINT ( 'NONE',  ( -9.598844408820454532, 35.54296874999999289, 9.598844408820459861 ) ) ;
#25065 = CARTESIAN_POINT ( 'NONE',  ( 71.94442639331153089, 31.55306875057403104, -11.16113171639042356 ) ) ;
#25066 = CARTESIAN_POINT ( 'NONE',  ( 91.91746824999998466, 107.3738262389971538, -53.27500000273119696 ) ) ;
#25067 = CARTESIAN_POINT ( 'NONE',  ( 97.93301269999999192, 123.8000000010924850, 0.8561741729129329626 ) ) ;
#25068 = CARTESIAN_POINT ( 'NONE',  ( 13.57481594606304576, 33.45937499999999432, -1.662435489736055892E-15 ) ) ;
#25069 = CARTESIAN_POINT ( 'NONE',  ( 91.91746824999997045, 107.3738262389971538, -53.77499999726881441 ) ) ;
#25070 = CARTESIAN_POINT ( 'NONE',  ( 130.0000000000000000, 35.39414062608393863, 13.14518615778179544 ) ) ;
#25071 = ORIENTED_EDGE ( 'NONE', *, *, #14212, .F. ) ;
#25072 = CARTESIAN_POINT ( 'NONE',  ( 114.9999999999999858, 120.0000000000000000, -45.00000000000000711 ) ) ;
#25073 = LINE ( 'NONE', #5561, #22154 ) ;
#25074 = CARTESIAN_POINT ( 'NONE',  ( 104.4587341249999639, 83.93750000136560629, -1.442382525525748735E-14 ) ) ;
#25075 = CARTESIAN_POINT ( 'NONE',  ( 95.00000000000000000, 91.56249999999998579, 2.071067811865463959 ) ) ;
#25076 = STYLED_ITEM ( 'NONE', ( #11491 ), #17619 ) ;
#25077 = CARTESIAN_POINT ( 'NONE',  ( 105.6631189606246295, 105.8855032339526758, -54.20000000000000995 ) ) ;
#25078 = CARTESIAN_POINT ( 'NONE',  ( 195.0000000000000000, 32.41757812608393863, -13.14518615778179544 ) ) ;
#25079 = CARTESIAN_POINT ( 'NONE',  ( -5.622872871577873077, 39.36289062716787157, -13.57481594606304753 ) ) ;
#25080 = ORIENTED_EDGE ( 'NONE', *, *, #5487, .F. ) ;
#25081 = CARTESIAN_POINT ( 'NONE',  ( 102.0710678118654329, -4.999999999999989342, 9.312499999999998224 ) ) ;
#25082 = ORIENTED_EDGE ( 'NONE', *, *, #6344, .F. ) ;
#25083 = CARTESIAN_POINT ( 'NONE',  ( 5.444914386472297529, 34.15390625108393863, -13.14518615778179900 ) ) ;
#25084 = CARTESIAN_POINT ( 'NONE',  ( 181.4251840539369596, 32.41757812716787157, 5.622872871577880183 ) ) ;
#25085 = CARTESIAN_POINT ( 'NONE',  ( 9.598844408820456309, 36.83281250216787583, -9.598844408820458085 ) ) ;
#25086 = CARTESIAN_POINT ( 'NONE',  ( 94.99999999999995737, 1.387778780781445676E-14, 14.12500000273118594 ) ) ;
#25087 = CIRCLE ( 'NONE', #4148, 11.57481594606304398 ) ;
#25088 = LINE ( 'NONE', #22678, #9348 ) ;
#25089 = CARTESIAN_POINT ( 'NONE',  ( 94.99999999999995737, 80.18750000273119838, 2.071067811865466624 ) ) ;
#25090 = CARTESIAN_POINT ( 'NONE',  ( 91.91746824999998466, 110.0000000000000000, -45.87499999726882294 ) ) ;
#25091 = CARTESIAN_POINT ( 'NONE',  ( 104.4587341249999781, 90.31249999863440792, -6.938893903907228378E-15 ) ) ;
#25092 = CARTESIAN_POINT ( 'NONE',  ( 98.23223304703363112, 124.1000000000000085, -1.767766952966370209 ) ) ;
#25093 = CARTESIAN_POINT ( 'NONE',  ( 204.5988444088204403, 39.90859374999999432, -9.598844408820458085 ) ) ;
#25094 = CONTEXT_DEPENDENT_SHAPE_REPRESENTATION ( #7496, #27001 ) ;
#25095 = CARTESIAN_POINT ( 'NONE',  ( 13.57481594606304931, 35.89023437716787868, 5.622872871577868636 ) ) ;
#25096 = CARTESIAN_POINT ( 'NONE',  ( 101.8468681455906903, 4.458734125000016313, 8.375000001365592084 ) ) ;
#25097 = DIRECTION ( 'NONE',  ( -0.000000000000000000, 1.000000000000000000, -0.000000000000000000 ) ) ;
#25098 = AXIS2_PLACEMENT_3D ( 'NONE', #7658, #24629, #7081 ) ;
#25099 = CARTESIAN_POINT ( 'NONE',  ( 95.54126587499996504, 1.846868145590750077, 9.375000001365593860 ) ) ;
#25100 = CARTESIAN_POINT ( 'NONE',  ( 105.6631189606246295, 105.8855032339526758, -51.70000000546237828 ) ) ;
#25101 = CARTESIAN_POINT ( 'NONE',  ( 95.54126587499999346, 94.99999999863439371, -1.846868145590737864 ) ) ;
#25102 = CARTESIAN_POINT ( 'NONE',  ( 102.4976396683250783, 102.3130555110000159, -55.02499999726882152 ) ) ;
#25103 = CARTESIAN_POINT ( 'NONE',  ( -13.14518615778179189, 32.86406250108393579, 5.444914386472304635 ) ) ;
#25104 = ORIENTED_EDGE ( 'NONE', *, *, #10185, .T. ) ;
#25105 = CARTESIAN_POINT ( 'NONE',  ( 2.493653234604083739E-15, 38.02343749999999289, 13.57481594606304576 ) ) ;
#25106 = CARTESIAN_POINT ( 'NONE',  ( 181.8548138422182205, 34.20351562608393436, 0.000000000000000000 ) ) ;
#25107 = ORIENTED_EDGE ( 'NONE', *, *, #18158, .F. ) ;
#25108 = CARTESIAN_POINT ( 'NONE',  ( 198.1146977455429692, 53.90847045361284984, -15.00000000000000000 ) ) ;
#25109 = CARTESIAN_POINT ( 'NONE',  ( 103.1528011352953342, -3.152801135295355106, 8.062500001365592084 ) ) ;
#25110 = ADVANCED_FACE ( 'NONE', ( #18036 ), #7054, .T. ) ;
#25111 = ORIENTED_EDGE ( 'NONE', *, *, #1653, .F. ) ;
#25112 = CARTESIAN_POINT ( 'NONE',  ( 97.50236033167492167, 102.3130555110000159, -44.97500000273119980 ) ) ;
#25113 = CARTESIAN_POINT ( 'NONE',  ( -8.049105076161786076E-16, 33.21132812608393436, -13.14518615778179544 ) ) ;
#25114 = CARTESIAN_POINT ( 'NONE',  ( 93.00000000000000000, 110.0000000000000000, -55.00000000000000711 ) ) ;
#25115 = CARTESIAN_POINT ( 'NONE',  ( 5.444914386472297529, 37.92421875108393436, -13.14518615778179722 ) ) ;
#25116 = CARTESIAN_POINT ( 'NONE',  ( 13.14518615778179544, 38.76757812608393294, -1.609821015232357215E-15 ) ) ;
#25117 = CARTESIAN_POINT ( 'NONE',  ( 5.444914386472297529, 40.50390625108394005, -13.14518615778179900 ) ) ;
#25118 = CARTESIAN_POINT ( 'NONE',  ( 101.8468681455907330, 91.74999999863439371, -4.458734124999994997 ) ) ;
#25119 = CARTESIAN_POINT ( 'NONE',  ( -9.598844408820458085, 36.23750000216787726, -9.598844408820458085 ) ) ;
#25120 = CARTESIAN_POINT ( 'NONE',  ( -8.312177448680279460E-16, 36.93203125216787441, -13.57481594606304576 ) ) ;
#25121 = CARTESIAN_POINT ( 'NONE',  ( 2.414731522848535132E-15, 33.01289062608393721, 13.14518615778179544 ) ) ;
#25122 = CARTESIAN_POINT ( 'NONE',  ( 95.54126587499996504, -1.846868145590724986, 3.750000001365591640 ) ) ;
#25123 =( BOUNDED_CURVE ( )  B_SPLINE_CURVE ( 2, ( #24300, #15738, #4641 ),
 .UNSPECIFIED., .F., .T. ) 
 B_SPLINE_CURVE_WITH_KNOTS ( ( 3, 3 ),
 ( 0.5208333333333332593, 0.5249747582430949189 ),
 .UNSPECIFIED. ) 
 CURVE ( )  GEOMETRIC_REPRESENTATION_ITEM ( )  RATIONAL_B_SPLINE_CURVE ( ( 1.000000000000000888, 0.9697362687807569159, 0.9635368518655843539 ) ) 
 REPRESENTATION_ITEM ( '' )  );
#25124 = CARTESIAN_POINT ( 'NONE',  ( 95.54126587499996504, 81.68750000136559208, -1.387778780781445676E-14 ) ) ;
#25125 = CARTESIAN_POINT ( 'NONE',  ( 2.414731522848535132E-15, 36.78320312608393294, 13.14518615778179544 ) ) ;
#25126 = CARTESIAN_POINT ( 'NONE',  ( 78.57481594606305464, 39.11484375216787157, -1.662435489736055892E-15 ) ) ;
#25127 = DIRECTION ( 'NONE',  ( -5.782411586589357392E-17, 0.000000000000000000, -1.000000000000000000 ) ) ;
#25128 = ORIENTED_EDGE ( 'NONE', *, *, #27941, .F. ) ;
#25129 = CARTESIAN_POINT ( 'NONE',  ( -9.295050272127046043, 34.30273437608393294, -9.295050272127046043 ) ) ;
#25130 = CARTESIAN_POINT ( 'NONE',  ( 99.14382582708707048, 124.4000000010924794, -2.066987299999999195 ) ) ;
#25131 = CARTESIAN_POINT ( 'NONE',  ( 104.4587341249999923, 95.49999999863440792, 1.846868145590726318 ) ) ;
#25132 = CARTESIAN_POINT ( 'NONE',  ( 93.46109445667489979, 105.2492070361643215, -49.67499999726882010 ) ) ;
#25133 = CARTESIAN_POINT ( 'NONE',  ( 116.4251840539369738, 39.56132812716787583, 5.622872871577880183 ) ) ;
#25134 = CARTESIAN_POINT ( 'NONE',  ( 2.414731522848535132E-15, 32.02070312608393010, 13.14518615778179544 ) ) ;
#25135 = ORIENTED_EDGE ( 'NONE', *, *, #4796, .F. ) ;
#25136 = CARTESIAN_POINT ( 'NONE',  ( 93.00000000000000000, 112.2744378736303332, -45.10000000000001563 ) ) ;
#25137 = CARTESIAN_POINT ( 'NONE',  ( 51.85481384221820633, 36.78320312608393294, 0.000000000000000000 ) ) ;
#25138 = DIRECTION ( 'NONE',  ( 0.000000000000000000, 0.000000000000000000, 1.000000000000000000 ) ) ;
#25139 = CARTESIAN_POINT ( 'NONE',  ( 195.0000000000000000, 31.82226562608393650, -13.14518615778179544 ) ) ;
#25140 = EDGE_LOOP ( 'NONE', ( #11298, #24578, #21866, #7185 ) ) ;
#25141 = CARTESIAN_POINT ( 'NONE',  ( 95.00000000000000000, 92.56249999999998579, 2.071067811865463959 ) ) ;
#25142 = CARTESIAN_POINT ( 'NONE',  ( 0.8389268692830608165, 53.50081894914648473, -14.99999999999999822 ) ) ;
#25143 = CARTESIAN_POINT ( 'NONE',  ( 65.00000000000000000, 36.03906250000000000, -13.57481594606304576 ) ) ;
#25144 = AXIS2_PLACEMENT_3D ( 'NONE', #28201, #28062, #17498 ) ;
#25145 = CARTESIAN_POINT ( 'NONE',  ( 135.6228728715778686, 39.26367187716787299, -13.57481594606304753 ) ) ;
#25146 = EDGE_CURVE ( 'NONE', #4009, #923, #4395, .T. ) ;
#25147 = CARTESIAN_POINT ( 'NONE',  ( 0.000000000000000000, 36.00000000000000000, 0.000000000000000000 ) ) ;
#25148 = CARTESIAN_POINT ( 'NONE',  ( 208.1451861577817795, 38.71796875108393721, 5.444914386472293977 ) ) ;
#25149 = ORIENTED_EDGE ( 'NONE', *, *, #9674, .F. ) ;
#25150 = ORIENTED_EDGE ( 'NONE', *, *, #23587, .F. ) ;
#25151 = CARTESIAN_POINT ( 'NONE',  ( 99.99999999999995737, -4.458734124999988779, 0.6875000013655923059 ) ) ;
#25152 = CARTESIAN_POINT ( 'NONE',  ( 195.0000000000000000, 50.00000000000000000, -2.255140518769849538E-14 ) ) ;
#25153 = CARTESIAN_POINT ( 'NONE',  ( 9.598844408820456309, 38.32109374999999574, -9.598844408820458085 ) ) ;
#25154 = CARTESIAN_POINT ( 'NONE',  ( 101.8468681455907046, 83.75000000136560629, 4.458734124999987891 ) ) ;
#25155 = CARTESIAN_POINT ( 'NONE',  ( 74.59884440882045453, 40.00781250216787299, -9.598844408820458085 ) ) ;
#25156 = FILL_AREA_STYLE_COLOUR ( '', #1792 ) ;
#25157 = CARTESIAN_POINT ( 'NONE',  ( 5.444914386472297529, 40.50390625108394005, -13.14518615778179900 ) ) ;
#25158 = CARTESIAN_POINT ( 'NONE',  ( -5.622872871577964560, 38.46992187499999005, -13.57481594606295339 ) ) ;
#25159 = SPHERICAL_SURFACE ( 'NONE', #27588, 5.000000000000000000 ) ;
#25160 = CARTESIAN_POINT ( 'NONE',  ( 65.00000000000000000, 40.80156249999999574, -13.57481594606304576 ) ) ;
#25161 = CARTESIAN_POINT ( 'NONE',  ( 120.4011555911795455, 33.75703124999999005, -9.598844408820458085 ) ) ;
#25162 = ORIENTED_EDGE ( 'NONE', *, *, #20148, .T. ) ;
#25163 = CIRCLE ( 'NONE', #21082, 10.50000000000001599 ) ;
#25164 = EDGE_LOOP ( 'NONE', ( #24467, #9180, #23984 ) ) ;
#25165 = UNCERTAINTY_MEASURE_WITH_UNIT (LENGTH_MEASURE( 1.000000000000000082E-05 ), #10302, 'distance_accuracy_value', 'NONE');
#25166 =( BOUNDED_SURFACE ( )  B_SPLINE_SURFACE ( 1, 2, ( 
 ( #19425, #8871, #1916, #17563, #10581, #14991, #6181, #26267, #14848, #6727, #10718, #28126, #17422, #23846, #23431, #3905, #2191, #49, #19147, #12565, #27990, #21717, #23569, #8451, #27852, #4184, #26121, #21291, #17139, #12845, #21574, #17280, #25983, #6453, #15124, #4323, #15414, #9158, #332, #9433, #4893 ),
 ( #13408, #13261, #22280, #20137, #2886, #15704, #18132, #24406, #21993, #7008, #18282, #2470, #24266, #5174, #24129, #17711, #20274, #9578, #616, #13837, #13556, #11275, #2613, #2755, #22417, #11131, #19846, #760, #26988, #11418, #22135, #26845, #9018, #4748, #17850, #19996, #3030, #475, #4602, #26413, #26553 ) ),
 .UNSPECIFIED., .F., .F., .T. ) 
 B_SPLINE_SURFACE_WITH_KNOTS ( ( 2, 2 ),
 ( 3, 2, 2, 2, 2, 2, 2, 2, 2, 2, 2, 2, 2, 2, 2, 2, 2, 2, 2, 2, 3 ),
 ( 0.000000000000000000, 1.000000000000000000 ),
 ( 0.000000000000000000, 0.04166666666666666435, 0.08333333333333332871, 0.1250000000000000000, 0.1666666666666666574, 0.2083333333333333426, 0.2500000000000000000, 0.2916666666666666852, 0.3333333333333333148, 0.3750000000000000000, 0.4166666666666666852, 0.4583333333333333148, 0.5000000000000000000, 0.5416666666666666297, 0.5833333333333333703, 0.6250000000000000000, 0.6666666666666666297, 0.7083333333333333703, 0.7500000000000000000, 0.7916666666666666297, 0.8333333333333333703 ),
 .UNSPECIFIED. ) 
 GEOMETRIC_REPRESENTATION_ITEM ( )  RATIONAL_B_SPLINE_SURFACE ( (
 ( 1.000000000000000000, 0.9238795325112867385, 1.000000000000000000, 0.9238795325112867385, 1.000000000000000000, 0.9238795325112867385, 1.000000000000000000, 0.9238795325112867385, 1.000000000000000000, 0.9238795325112867385, 1.000000000000000000, 0.9238795325112867385, 1.000000000000000000, 0.9238795325112867385, 1.000000000000000000, 0.9238795325112867385, 1.000000000000000000, 0.9238795325112867385, 1.000000000000000000, 0.9238795325112867385, 1.000000000000000000, 0.9238795325112867385, 1.000000000000000000, 0.9238795325112867385, 1.000000000000000000, 0.9238795325112867385, 1.000000000000000000, 0.9238795325112867385, 1.000000000000000000, 0.9238795325112867385, 1.000000000000000000, 0.9238795325112867385, 1.000000000000000000, 0.9238795325112867385, 1.000000000000000000, 0.9238795325112867385, 1.000000000000000000, 0.9238795325112867385, 1.000000000000000000, 0.9238795325112867385, 1.000000000000000000),
 ( 1.000000000000000000, 0.9238795325112867385, 1.000000000000000000, 0.9238795325112867385, 1.000000000000000000, 0.9238795325112867385, 1.000000000000000000, 0.9238795325112867385, 1.000000000000000000, 0.9238795325112867385, 1.000000000000000000, 0.9238795325112867385, 1.000000000000000000, 0.9238795325112867385, 1.000000000000000000, 0.9238795325112867385, 1.000000000000000000, 0.9238795325112867385, 1.000000000000000000, 0.9238795325112867385, 1.000000000000000000, 0.9238795325112867385, 1.000000000000000000, 0.9238795325112867385, 1.000000000000000000, 0.9238795325112867385, 1.000000000000000000, 0.9238795325112867385, 1.000000000000000000, 0.9238795325112867385, 1.000000000000000000, 0.9238795325112867385, 1.000000000000000000, 0.9238795325112867385, 1.000000000000000000, 0.9238795325112867385, 1.000000000000000000, 0.9238795325112867385, 1.000000000000000000, 0.9238795325112867385, 1.000000000000000000) ) ) 
 REPRESENTATION_ITEM ( '' )  SURFACE ( )  );
#25167 = CARTESIAN_POINT ( 'NONE',  ( 9.598844408820456309, 40.70234374999999716, -9.598844408820458085 ) ) ;
#25168 = CARTESIAN_POINT ( 'NONE',  ( -13.14518615778179900, 38.91640625108393436, -5.444914386472297529 ) ) ;
#25169 = CARTESIAN_POINT ( 'NONE',  ( 103.5355339059327093, -3.535533905932726206, 7.500000002731185944 ) ) ;
#25170 = CARTESIAN_POINT ( 'NONE',  ( 120.7049497278729575, 39.06523437608392868, -9.295050272127046043 ) ) ;
#25171 = CARTESIAN_POINT ( 'NONE',  ( 78.14518615778179367, 39.31328125108392868, 5.444914386472293977 ) ) ;
#25172 = ORIENTED_EDGE ( 'NONE', *, *, #7608, .T. ) ;
#25173 = ORIENTED_EDGE ( 'NONE', *, *, #22101, .T. ) ;
#25174 = CARTESIAN_POINT ( 'NONE',  ( 61.86382637865181522, 36.00000000000000711, 12.79489613812742910 ) ) ;
#25175 = CARTESIAN_POINT ( 'NONE',  ( 13.14518615778179544, 40.15664062608393436, -1.609821015232357215E-15 ) ) ;
#25176 = EDGE_CURVE ( 'NONE', #12047, #25968, #20326, .T. ) ;
#25177 = CARTESIAN_POINT ( 'NONE',  ( 98.96446609406727646, 123.6500000021849530, 2.499999999999977796 ) ) ;
#25178 = CARTESIAN_POINT ( 'NONE',  ( 183.7351811978183207, 35.99999999999997158, 6.828991891054760011 ) ) ;
#25179 = CARTESIAN_POINT ( 'NONE',  ( 95.00472066334981491, 116.8754121666685393, -52.17499999726882010 ) ) ;
#25180 = DIRECTION ( 'NONE',  ( 0.000000000000000000, -0.000000000000000000, 1.000000000000000000 ) ) ;
#25181 = LINE ( 'NONE', #5669, #2681 ) ;
#25182 = CARTESIAN_POINT ( 'NONE',  ( 0.000000000000000000, -7.395377635281828788, 0.000000000000000000 ) ) ;
#25183 = CARTESIAN_POINT ( 'NONE',  ( 98.23223304703363112, 124.2999999999999972, 1.767766952966351557 ) ) ;
#25184 = EDGE_CURVE ( 'NONE', #18668, #11161, #22978, .T. ) ;
#25185 = CARTESIAN_POINT ( 'NONE',  ( 102.0669872999999797, 122.5500000010924850, -9.794112055954760458E-15 ) ) ;
#25186 = CARTESIAN_POINT ( 'NONE',  ( 91.91746824999998466, 110.0000000000000000, -55.74999999726882294 ) ) ;
#25187 = DIRECTION ( 'NONE',  ( -0.000000000000000000, 1.000000000000000000, -0.000000000000000000 ) ) ;
#25188 = CARTESIAN_POINT ( 'NONE',  ( 98.15313185440925281, -4.458734124999987891, 13.62500000136559208 ) ) ;
#25189 = CARTESIAN_POINT ( 'NONE',  ( 107.0000000000000142, 110.0000000000000000, -47.50000000546238255 ) ) ;
#25190 =( REPRESENTATION_RELATIONSHIP ('NONE','NONE', #2411, #17883 ) REPRESENTATION_RELATIONSHIP_WITH_TRANSFORMATION ( #15353 )SHAPE_REPRESENTATION_RELATIONSHIP( ) );
#25191 = EDGE_LOOP ( 'NONE', ( #18671, #14544, #6473, #28098 ) ) ;
#25192 = CARTESIAN_POINT ( 'NONE',  ( -4.459473413638155748, 36.00000000000000711, -12.68347323196786114 ) ) ;
#25193 = CARTESIAN_POINT ( 'NONE',  ( 9.598844408820459861, 40.50390624999999289, 9.598844408820456309 ) ) ;
#25194 = CARTESIAN_POINT ( 'NONE',  ( 13.14518615778179900, 33.85625000108393579, -5.444914386472297529 ) ) ;
#25195 = CARTESIAN_POINT ( 'NONE',  ( 9.295050272127046043, 33.11210937608393579, -9.295050272127046043 ) ) ;
#25196 = ADVANCED_FACE ( 'NONE', ( #13605 ), #668, .F. ) ;
#25197 = CARTESIAN_POINT ( 'NONE',  ( 9.598844408820459861, 32.66562500216787157, 9.598844408820456309 ) ) ;
#25198 = CYLINDRICAL_SURFACE ( 'NONE', #15368, 4.999999999999989342 ) ;
#25199 = CARTESIAN_POINT ( 'NONE',  ( 99.99999999999995737, 83.43750000136560629, -4.458734125000016313 ) ) ;
#25200 = CARTESIAN_POINT ( 'NONE',  ( 78.14518615778179367, 40.30546875108393579, 5.444914386472293977 ) ) ;
#25201 = CARTESIAN_POINT ( 'NONE',  ( 93.46109445667491400, 114.7507929638356785, -51.57500000273120122 ) ) ;
#25202 = CARTESIAN_POINT ( 'NONE',  ( 65.00000000000000000, -7.395377635281828788, -7.517135062566165128E-15 ) ) ;
#25203 = CARTESIAN_POINT ( 'NONE',  ( 102.0669872999999797, 122.5500000010924850, -9.794112055954760458E-15 ) ) ;
#25204 = CARTESIAN_POINT ( 'NONE',  ( 102.4999999999999858, 122.9999999999999858, 0.3272492347489319164 ) ) ;
#25205 = CARTESIAN_POINT ( 'NONE',  ( 104.3262379212492448, 104.0454443415356991, -47.79999999453763593 ) ) ;
#25206 = CARTESIAN_POINT ( 'NONE',  ( 130.0000000000000000, 35.79101562608394005, -13.14518615778179544 ) ) ;
#25207 = ORIENTED_EDGE ( 'NONE', *, *, #7608, .F. ) ;
#25208 = CARTESIAN_POINT ( 'NONE',  ( 95.67376207875072680, 104.0454443415356991, -52.19999999453764161 ) ) ;
#25209 = CARTESIAN_POINT ( 'NONE',  ( 96.84719886470459471, 81.56250000136559208, 3.152801135295355994 ) ) ;
#25210 = CARTESIAN_POINT ( 'NONE',  ( 103.5355339059327235, 94.87500000000000000, 3.535533905932724874 ) ) ;
#25211 = CARTESIAN_POINT ( 'NONE',  ( 51.42518405393695957, 40.30546875216787583, 0.000000000000000000 ) ) ;
#25212 = CIRCLE ( 'NONE', #22949, 13.57481594606304576 ) ;
#25213 = CARTESIAN_POINT ( 'NONE',  ( 99.99999999999997158, 118.4984768113314004, -52.12499999726880873 ) ) ;
#25214 = CARTESIAN_POINT ( 'NONE',  ( -13.57481594606304576, 39.56132812716787583, 5.622872871577880183 ) ) ;
#25215 = ORIENTED_EDGE ( 'NONE', *, *, #6469, .T. ) ;
#25216 = CARTESIAN_POINT ( 'NONE',  ( 99.99999999999995737, 5.000000000000018652, 7.749999999999999112 ) ) ;
#25217 = ORIENTED_EDGE ( 'NONE', *, *, #21122, .F. ) ;
#25218 = CARTESIAN_POINT ( 'NONE',  ( 13.14518615778179544, 34.00507812608393721, -1.609821015232357215E-15 ) ) ;
#25219 = CARTESIAN_POINT ( 'NONE',  ( 200.4449143864723055, 39.21406250108392300, 13.14518615778179189 ) ) ;
#25220 = CARTESIAN_POINT ( 'NONE',  ( 7.171390501253594785, 31.30502191632583830, -11.52591802191987114 ) ) ;
#25221 = ADVANCED_FACE ( 'NONE', ( #7482 ), #16029, .T. ) ;
#25222 = CARTESIAN_POINT ( 'NONE',  ( 102.0710678118654329, 5.000000000000018652, 13.81250000273118594 ) ) ;
#25223 = CARTESIAN_POINT ( 'NONE',  ( 130.0000000000000000, 36.78320312608393294, 13.14518615778179544 ) ) ;
#25224 = CARTESIAN_POINT ( 'NONE',  ( 99.99999999999995737, 1.387778780781445676E-14, 34.79898987322334136 ) ) ;
#25225 = CARTESIAN_POINT ( 'NONE',  ( 139.5988444088204403, 37.52734375000000000, -9.598844408820458085 ) ) ;
#25226 = LINE ( 'NONE', #10789, #21062 ) ;
#25227 = CARTESIAN_POINT ( 'NONE',  ( 97.50000000000000000, 123.4500000000000028, 1.035533905932725096 ) ) ;
#25228 = CARTESIAN_POINT ( 'NONE',  ( 189.5550856135277229, 32.16953125108393152, 13.14518615778179722 ) ) ;
#25229 = DIRECTION ( 'NONE',  ( 0.000000000000000000, 0.000000000000000000, -1.000000000000000000 ) ) ;
#25230 = CARTESIAN_POINT ( 'NONE',  ( 98.15313185440925281, 4.458734125000016313, 5.500000001365592972 ) ) ;
#25231 = CARTESIAN_POINT ( 'NONE',  ( 95.67376207875072680, 115.9545556584642867, -52.80000000546237260 ) ) ;
#25232 = CARTESIAN_POINT ( 'NONE',  ( 104.4587341249999781, 1.846868145590750521, 6.000000001365592084 ) ) ;
#25233 = CARTESIAN_POINT ( 'NONE',  ( 104.3262379212492590, 115.9545556584642867, -47.20000000546238539 ) ) ;
#25234 = CARTESIAN_POINT ( 'NONE',  ( 99.99999999999998579, 95.31249999863440792, 4.458734124999981674 ) ) ;
#25235 = CARTESIAN_POINT ( 'NONE',  ( 99.99999999999998579, 128.0000000000000000, -0.5000000000000138778 ) ) ;
#25236 = CARTESIAN_POINT ( 'NONE',  ( 91.91746824999997045, 107.3738262389971680, -55.52499999726881441 ) ) ;
#25237 = CARTESIAN_POINT ( 'NONE',  ( 13.14518615778179900, 34.84843750108393579, -5.444914386472297529 ) ) ;
#25238 = ORIENTED_EDGE ( 'NONE', *, *, #9714, .F. ) ;
#25239 = CARTESIAN_POINT ( 'NONE',  ( 99.99999999999995737, 85.00000000000000000, 4.999999999999990230 ) ) ;
#25240 = AXIS2_PLACEMENT_3D ( 'NONE', #17840, #20127, #7424 ) ;
#25241 = CARTESIAN_POINT ( 'NONE',  ( 98.15313185440925281, 90.99999999863439371, 4.458734124999979898 ) ) ;
#25242 = VERTEX_POINT ( 'NONE', #15753 ) ;
#25243 = CARTESIAN_POINT ( 'NONE',  ( 200.4449143864723055, 33.65781250108393152, 13.14518615778179189 ) ) ;
#25244 = ORIENTED_EDGE ( 'NONE', *, *, #733, .T. ) ;
#25245 = CARTESIAN_POINT ( 'NONE',  ( 201.4508793426651039, 50.00000000106953735, -11.97362904075546197 ) ) ;
#25246 = CARTESIAN_POINT ( 'NONE',  ( 104.4587341249999781, -1.846868145590721655, 6.125000001365591196 ) ) ;
#25247 = VERTEX_POINT ( 'NONE', #22327 ) ;
#25248 = CARTESIAN_POINT ( 'NONE',  ( 106.5389055433251002, 105.2492070361643215, -50.57500000273120122 ) ) ;
#25249 = CARTESIAN_POINT ( 'NONE',  ( -8.049105076161786076E-16, 34.00507812608393721, -13.14518615778179544 ) ) ;
#25250 = FACE_OUTER_BOUND ( 'NONE', #22548, .T. ) ;
#25251 = CARTESIAN_POINT ( 'NONE',  ( 5.444914386472302859, 38.42031250108393436, 13.14518615778179189 ) ) ;
#25252 = CARTESIAN_POINT ( 'NONE',  ( -9.295050272127046043, 36.68398437608393436, -9.295050272127046043 ) ) ;
#25253 = CARTESIAN_POINT ( 'NONE',  ( -5.444914386472297529, 32.46718750108393436, -13.14518615778179900 ) ) ;
#25254 = AXIS2_PLACEMENT_3D ( 'NONE', #16344, #24092, #4567 ) ;
#25255 = CARTESIAN_POINT ( 'NONE',  ( 98.15313185440925281, 93.87499999863439371, -4.458734124999994997 ) ) ;
#25256 = CARTESIAN_POINT ( 'NONE',  ( 0.000000000000000000, 30.99999999999999645, 0.000000000000000000 ) ) ;
#25257 = CARTESIAN_POINT ( 'NONE',  ( 78.57481594606305464, 38.22187499999999716, -1.662435489736055892E-15 ) ) ;
#25258 = CARTESIAN_POINT ( 'NONE',  ( -13.14518615778179900, 33.55859375108393294, -5.444914386472297529 ) ) ;
#25259 = CARTESIAN_POINT ( 'NONE',  ( 95.54126587499996504, 1.846868145590750077, 1.625000001365593416 ) ) ;
#25260 = CARTESIAN_POINT ( 'NONE',  ( 95.54126587499996504, 81.75000000136560629, 1.846868145590724986 ) ) ;
#25261 = CARTESIAN_POINT ( 'NONE',  ( -9.295050272127046043, 35.69179687608393436, -9.295050272127046043 ) ) ;
#25262 = CARTESIAN_POINT ( 'NONE',  ( 13.57481594606304576, 32.66562499999999858, -1.662435489736055892E-15 ) ) ;
#25263 = CYLINDRICAL_SURFACE ( 'NONE', #1078, 5.000000000000004441 ) ;
#25264 = ORIENTED_EDGE ( 'NONE', *, *, #9306, .F. ) ;
#25265 = CARTESIAN_POINT ( 'NONE',  ( 2.414731522848535132E-15, 33.01289062608393721, 13.14518615778179544 ) ) ;
#25266 = EDGE_CURVE ( 'NONE', #2842, #4709, #2130, .T. ) ;
#25267 = CARTESIAN_POINT ( 'NONE',  ( 102.0669873000000081, 124.1000000010924822, 0.8561741729129311862 ) ) ;
#25268 = CARTESIAN_POINT ( 'NONE',  ( 96.84719886470463734, 93.18749999863440792, 3.152801135295351997 ) ) ;
#25269 = CARTESIAN_POINT ( 'NONE',  ( 107.0000000000000000, 110.0000000000000000, -49.49999999453764588 ) ) ;
#25270 = CARTESIAN_POINT ( 'NONE',  ( 91.91746824999998466, 110.0000000000000000, -55.87499999726882294 ) ) ;
#25271 = AXIS2_PLACEMENT_3D ( 'NONE', #4402, #13057, #6664 ) ;
#25272 = CYLINDRICAL_SURFACE ( 'NONE', #21242, 5.000000000000004441 ) ;
#25273 = CARTESIAN_POINT ( 'NONE',  ( -5.444914386472297529, 31.67343750108393863, -13.14518615778179900 ) ) ;
#25274 = EDGE_LOOP ( 'NONE', ( #14856, #282, #20807, #5595, #9041, #8685 ) ) ;
#25275 = CARTESIAN_POINT ( 'NONE',  ( 55.70494972787295751, 39.06523437608392868, -9.295050272127046043 ) ) ;
#25276 = ORIENTED_EDGE ( 'NONE', *, *, #15137, .T. ) ;
#25277 = DIRECTION ( 'NONE',  ( 0.000000000000000000, 0.000000000000000000, -1.000000000000000000 ) ) ;
#25278 = CARTESIAN_POINT ( 'NONE',  ( 185.7049497278729575, 31.92148437608393508, -9.295050272127046043 ) ) ;
#25279 = EDGE_LOOP ( 'NONE', ( #14134, #26075, #106, #21111, #17939, #3552, #14152, #22414, #9251, #18995, #25707, #19713, #24575 ) ) ;
#25280 = CARTESIAN_POINT ( 'NONE',  ( 94.99999999999995737, 1.387778780781445676E-14, 2.125000002731185056 ) ) ;
#25281 = CARTESIAN_POINT ( 'NONE',  ( 65.00000000000000000, 40.40468749999999432, 13.57481594606304576 ) ) ;
#25282 = AXIS2_PLACEMENT_3D ( 'NONE', #20245, #11818, #14099 ) ;
#25283 = VECTOR ( 'NONE', #7131, 1000.000000000000000 ) ;
#25284 = CARTESIAN_POINT ( 'NONE',  ( 135.6228728715779539, 36.58476562716786873, 13.57481594606297115 ) ) ;
#25285 = CARTESIAN_POINT ( 'NONE',  ( 116.4251840539369454, 33.90585937716787868, -5.622872871577873077 ) ) ;
#25286 =( BOUNDED_CURVE ( )  B_SPLINE_CURVE ( 2, ( #16528, #9828, #25085, #21087, #18938, #10228, #1434, #5710, #3285 ),
 .UNSPECIFIED., .F., .F. ) 
 B_SPLINE_CURVE_WITH_KNOTS ( ( 3, 2, 2, 2, 3 ),
 ( 0.3541666666666666852, 0.3645833333333332593, 0.3749999999999998890, 0.3854166666666665741, 0.3958333333333331483 ),
 .UNSPECIFIED. ) 
 CURVE ( )  GEOMETRIC_REPRESENTATION_ITEM ( )  RATIONAL_B_SPLINE_CURVE ( ( 1.000000000000000000, 0.9238795325112867385, 1.000000000000000000, 0.9238795325112867385, 1.000000000000000000, 0.9238795325112867385, 1.000000000000000000, 0.9238795325112879597, 0.9999999999999987788 ) ) 
 REPRESENTATION_ITEM ( '' )  );
#25287 = CARTESIAN_POINT ( 'NONE',  ( 94.33688103937537051, 105.8855032339526758, -44.30000000546237970 ) ) ;
#25288 = CARTESIAN_POINT ( 'NONE',  ( 105.6631189606246153, 114.1144967660473242, -47.29999999453764303 ) ) ;
#25289 = CARTESIAN_POINT ( 'NONE',  ( 195.0000000000000000, 39.36289062608393152, 13.14518615778179544 ) ) ;
#25290 = ORIENTED_EDGE ( 'NONE', *, *, #24275, .F. ) ;
#25291 = CARTESIAN_POINT ( 'NONE',  ( 101.8468681455906903, 4.458734125000016313, 14.37500000136559386 ) ) ;
#25292 = CARTESIAN_POINT ( 'NONE',  ( 96.84719886470459471, -3.152801135295355994, 13.81250000136559208 ) ) ;
#25293 = DIRECTION ( 'NONE',  ( -0.000000000000000000, -1.000000000000000000, -0.000000000000000000 ) ) ;
#25294 = CARTESIAN_POINT ( 'NONE',  ( 99.99999999999995737, 83.18750000136560629, -4.458734125000016313 ) ) ;
#25295 = FACE_BOUND ( 'NONE', #26299, .T. ) ;
#25296 = CARTESIAN_POINT ( 'NONE',  ( 99.99999999999998579, 91.62499999726880162, 4.999999999999984013 ) ) ;
#25297 = EDGE_CURVE ( 'NONE', #370, #20441, #21130, .T. ) ;
#25298 = CARTESIAN_POINT ( 'NONE',  ( -13.14518615778179900, 39.90859375108394147, -5.444914386472297529 ) ) ;
#25299 = CARTESIAN_POINT ( 'NONE',  ( 96.46446609406721961, 80.87500000000000000, -3.535533905932755072 ) ) ;
#25300 = CIRCLE ( 'NONE', #13450, 22.40192378864669109 ) ;
#25301 = DIRECTION ( 'NONE',  ( 0.000000000000000000, -1.000000000000000000, 0.000000000000000000 ) ) ;
#25302 = CARTESIAN_POINT ( 'NONE',  ( 99.99999999999998579, 90.00000000000000000, -6.938893903907228378E-15 ) ) ;
#25303 = CARTESIAN_POINT ( 'NONE',  ( 102.4976396683250783, 102.3130555110000159, -49.02499999726882152 ) ) ;
#25304 = VERTEX_POINT ( 'NONE', #10305 ) ;
#25305 = ORIENTED_EDGE ( 'NONE', *, *, #3443, .F. ) ;
#25306 = CARTESIAN_POINT ( 'NONE',  ( 99.99999999999995737, 84.75000000000000000, -5.000000000000018652 ) ) ;
#25307 = CARTESIAN_POINT ( 'NONE',  ( 13.57481594606304576, 39.80937499999999574, -1.662435489736055892E-15 ) ) ;
#25308 = CARTESIAN_POINT ( 'NONE',  ( 13.57481594606304931, 31.92148437716787512, 5.622872871577869525 ) ) ;
#25309 = CARTESIAN_POINT ( 'NONE',  ( 94.99999999999995737, 2.071067811865491048, 5.062500002731185944 ) ) ;
#25310 = CARTESIAN_POINT ( 'NONE',  ( 130.0000000000000000, 31.62382812608393579, -13.14518615778179544 ) ) ;
#25311 = CARTESIAN_POINT ( 'NONE',  ( 51.85481384221820633, 35.79101562608393294, 0.000000000000000000 ) ) ;
#25312 = CARTESIAN_POINT ( 'NONE',  ( 52.26160984214450878, 36.00000000000000000, 3.273369733618432864 ) ) ;
#25313 = CARTESIAN_POINT ( 'NONE',  ( 13.14518615778179900, 36.13828125108393863, 5.444914386472293977 ) ) ;
#25314 = CARTESIAN_POINT ( 'NONE',  ( -14.99999999999999822, 80.00000000000000000, 15.00000000000000000 ) ) ;
#25315 = CARTESIAN_POINT ( 'NONE',  ( 102.4999999999999716, 123.9500000021849502, -1.035533905932742638 ) ) ;
#25316 = CARTESIAN_POINT ( 'NONE',  ( 0.000000000000000000, 36.00000000000000000, -11.57481594606304576 ) ) ;
#25317 = CARTESIAN_POINT ( 'NONE',  ( 116.4251840539369596, 40.20624999999999005, 0.000000000000000000 ) ) ;
#25318 = FILL_AREA_STYLE ('',( #25047 ) ) ;
#25319 = CARTESIAN_POINT ( 'NONE',  ( -13.14518615778179189, 37.42812500108393436, 5.444914386472304635 ) ) ;
#25320 = VECTOR ( 'NONE', #16052, 1000.000000000000000 ) ;
#25321 = LINE ( 'NONE', #10189, #6988 ) ;
#25322 = CARTESIAN_POINT ( 'NONE',  ( 102.4999999999999716, 123.8500000000000085, -1.035533905932742638 ) ) ;
#25323 = CARTESIAN_POINT ( 'NONE',  ( 99.14382582708707048, 123.0000000010925021, -2.066987299999999195 ) ) ;
#25324 = CYLINDRICAL_SURFACE ( 'NONE', #2787, 3.000000000000004441 ) ;
#25325 = ADVANCED_FACE ( 'NONE', ( #27725 ), #7871, .F. ) ;
#25326 = LINE ( 'NONE', #16768, #27746 ) ;
#25327 = CARTESIAN_POINT ( 'NONE',  ( 101.8468681455906903, -4.458734124999987891, 13.75000000136559208 ) ) ;
#25328 = CARTESIAN_POINT ( 'NONE',  ( -9.598844408820458085, 32.26875000216787726, -9.598844408820458085 ) ) ;
#25329 = ORIENTED_EDGE ( 'NONE', *, *, #3035, .F. ) ;
#25330 = CARTESIAN_POINT ( 'NONE',  ( 97.50000000000000000, 124.3000000021849587, -9.540979117872439019E-15 ) ) ;
#25331 = CARTESIAN_POINT ( 'NONE',  ( 2.493653234604083739E-15, 40.40468749999999432, 13.57481594606304576 ) ) ;
#25332 = CARTESIAN_POINT ( 'NONE',  ( -9.295050272127044266, 32.71523437608393436, 9.295050272127047819 ) ) ;
#25333 = CARTESIAN_POINT ( 'NONE',  ( 2.493653234604083739E-15, 34.15390625216787157, 13.57481594606304576 ) ) ;
#25334 = DIRECTION ( 'NONE',  ( -1.000000000000000000, 0.000000000000000000, 0.000000000000000000 ) ) ;
#25335 = CARTESIAN_POINT ( 'NONE',  ( 103.1528011352953342, 79.81250000136559208, 3.152801135295355106 ) ) ;
#25336 = CARTESIAN_POINT ( 'NONE',  ( 65.00000000000000000, 39.75976562608394005, -13.14518615778179544 ) ) ;
#25337 =( BOUNDED_CURVE ( )  B_SPLINE_CURVE ( 2, ( #26242, #12540, #166, #19680, #6700, #17110, #27829, #19542, #23544 ),
 .UNSPECIFIED., .F., .F. ) 
 B_SPLINE_CURVE_WITH_KNOTS ( ( 3, 2, 2, 2, 3 ),
 ( 0.1875000000000001388, 0.1979166666666667407, 0.2083333333333333703, 0.2187499999999999722, 0.2291666666666665741 ),
 .UNSPECIFIED. ) 
 CURVE ( )  GEOMETRIC_REPRESENTATION_ITEM ( )  RATIONAL_B_SPLINE_CURVE ( ( 0.9999999999999990008, 0.9238795325112877377, 1.000000000000000000, 0.9238795325112867385, 1.000000000000000000, 0.9238795325112867385, 1.000000000000000000, 0.9238795325112872936, 0.9999999999999994449 ) ) 
 REPRESENTATION_ITEM ( '' )  );
#25338 = CARTESIAN_POINT ( 'NONE',  ( 104.9952793366501851, 116.8754121666685393, -50.07500000273120122 ) ) ;
#25339 = LINE ( 'NONE', #5825, #24594 ) ;
#25340 = VECTOR ( 'NONE', #7805, 1000.000000000000000 ) ;
#25341 = ADVANCED_FACE ( 'NONE', ( #20891 ), #10034, .T. ) ;
#25342 = DIRECTION ( 'NONE',  ( 0.000000000000000000, -1.000000000000000000, -0.000000000000000000 ) ) ;
#25343 = CARTESIAN_POINT ( 'NONE',  ( -8.312177448680279460E-16, 33.65781249999999147, -13.57481594606304576 ) ) ;
#25344 = CARTESIAN_POINT ( 'NONE',  ( 94.33688103937534208, 114.1144967660473242, -50.69999999453764161 ) ) ;
#25345 = CARTESIAN_POINT ( 'NONE',  ( 124.5550856135277087, 31.87187500108393223, -13.14518615778179900 ) ) ;
#25346 = ORIENTED_EDGE ( 'NONE', *, *, #19063, .F. ) ;
#25347 = CARTESIAN_POINT ( 'NONE',  ( 104.9999999999999716, 2.071067811865491937, 7.562499999999999112 ) ) ;
#25348 = EDGE_CURVE ( 'NONE', #16116, #19665, #12438, .T. ) ;
#25349 = CARTESIAN_POINT ( 'NONE',  ( 13.14518615778179900, 40.30546875108393579, 5.444914386472293977 ) ) ;
#25350 = CARTESIAN_POINT ( 'NONE',  ( 101.8468681455906903, 80.12500000136560629, -4.458734125000016313 ) ) ;
#25351 = AXIS2_PLACEMENT_3D ( 'NONE', #16668, #27648, #23230 ) ;
#25352 = CARTESIAN_POINT ( 'NONE',  ( 116.8548138422182063, 39.80937500108392868, 5.444914386472304635 ) ) ;
#25353 = CARTESIAN_POINT ( 'NONE',  ( 55.40115559117954547, 38.02343750216788010, 9.598844408820459861 ) ) ;
#25354 = ADVANCED_FACE ( 'NONE', ( #19011, #8044 ), #7772, .T. ) ;
#25355 = AXIS2_PLACEMENT_3D ( 'NONE', #9623, #18328, #11886 ) ;
#25356 = CARTESIAN_POINT ( 'NONE',  ( 104.9952793366501709, 116.8754121666685393, -50.32499999726882578 ) ) ;
#25357 = CARTESIAN_POINT ( 'NONE',  ( 13.57481594606304576, 39.90859375216787441, -1.662435489736055892E-15 ) ) ;
#25358 = ORIENTED_EDGE ( 'NONE', *, *, #5693, .T. ) ;
#25359 = CARTESIAN_POINT ( 'NONE',  ( 94.99999999999995737, -2.071067811865466624, 9.062499999999998224 ) ) ;
#25360 = EDGE_CURVE ( 'NONE', #9281, #4419, #22048, .T. ) ;
#25361 = CARTESIAN_POINT ( 'NONE',  ( 93.00000000000000000, 110.0000000000000000, -52.00000000000000711 ) ) ;
#25362 = CARTESIAN_POINT ( 'NONE',  ( 13.14518615778179900, 34.74921875108395142, 5.444914386472293977 ) ) ;
#25363 = CARTESIAN_POINT ( 'NONE',  ( 202.1713913950166273, 31.30502190640808990, -11.52591746582321974 ) ) ;
#25364 = CIRCLE ( 'NONE', #3963, 5.000000000000004441 ) ;
#25365 = CARTESIAN_POINT ( 'NONE',  ( 92.99999999999998579, 110.0000000000000000, -145.0000000000000284 ) ) ;
#25366 = CARTESIAN_POINT ( 'NONE',  ( 120.7049497278729575, 39.06523437608392868, 9.295050272127047819 ) ) ;
#25367 = CARTESIAN_POINT ( 'NONE',  ( 13.14518615778179900, 32.36796875108393579, 5.444914386472293977 ) ) ;
#25368 = CARTESIAN_POINT ( 'NONE',  ( 92.99999999999998579, 110.0000000000000000, -50.49999999453763877 ) ) ;
#25369 = DIRECTION ( 'NONE',  ( 0.000000000000000000, 0.000000000000000000, -1.000000000000000000 ) ) ;
#25370 = CARTESIAN_POINT ( 'NONE',  ( 99.14382582708707048, 124.1000000010924964, 2.066987299999979211 ) ) ;
#25371 = CARTESIAN_POINT ( 'NONE',  ( 208.5748159460630688, 38.22187499999999716, -1.662435489736055892E-15 ) ) ;
#25372 = EDGE_CURVE ( 'NONE', #2214, #24582, #23869, .T. ) ;
#25373 = PRODUCT_CONTEXT ( 'NONE', #10768, 'mechanical' ) ;
#25374 = CARTESIAN_POINT ( 'NONE',  ( 99.99999999999998579, 93.25000000000000000, -4.999999999999997335 ) ) ;
#25375 = CARTESIAN_POINT ( 'NONE',  ( 103.1528011352953342, 3.152801135295383084, 2.312500001365592084 ) ) ;
#25376 = CARTESIAN_POINT ( 'NONE',  ( 78.14518615778179367, 38.51953125108393294, 5.444914386472293977 ) ) ;
#25377 = CARTESIAN_POINT ( 'NONE',  ( 98.15313185440923860, 4.458734125000016313, 7.250000001365592084 ) ) ;
#25378 = CARTESIAN_POINT ( 'NONE',  ( 107.0000000000000142, 107.7255621263696526, -51.60000000546238397 ) ) ;
#25379 = CARTESIAN_POINT ( 'NONE',  ( 95.54126587500000767, 94.06249999863440792, -7.484931351350258973E-15 ) ) ;
#25380 =( BOUNDED_CURVE ( )  B_SPLINE_CURVE ( 2, ( #26340, #24198, #13049, #20066, #17919 ),
 .UNSPECIFIED., .F., .F. ) 
 B_SPLINE_CURVE_WITH_KNOTS ( ( 3, 2, 3 ),
 ( 0.000000000000000000, 0.02500000000000002220, 0.05000000000000004441 ),
 .UNSPECIFIED. ) 
 CURVE ( )  GEOMETRIC_REPRESENTATION_ITEM ( )  RATIONAL_B_SPLINE_CURVE ( ( 1.000000000000000000, 0.9238795325112867385, 1.000000000000000000, 0.9238795325112866275, 1.000000000000000222 ) ) 
 REPRESENTATION_ITEM ( '' )  );
#25381 = CARTESIAN_POINT ( 'NONE',  ( 200.6228728715777549, 39.66054687500000142, 13.57481594606318076 ) ) ;
#25382 = LINE ( 'NONE', #17084, #17994 ) ;
#25383 = CARTESIAN_POINT ( 'NONE',  ( -8.312177448680279460E-16, 40.00781250000000000, -13.57481594606304576 ) ) ;
#25384 = VERTEX_POINT ( 'NONE', #25995 ) ;
#25385 = CARTESIAN_POINT ( 'NONE',  ( 103.1528011352953342, 84.06250000136560629, 3.152801135295355106 ) ) ;
#25386 = EDGE_CURVE ( 'NONE', #27020, #15564, #3488, .T. ) ;
#25387 = VECTOR ( 'NONE', #21451, 1000.000000000000000 ) ;
#25388 = ORIENTED_EDGE ( 'NONE', *, *, #1321, .F. ) ;
#25389 = EDGE_CURVE ( 'NONE', #4172, #25694, #11974, .T. ) ;
#25390 = VERTEX_POINT ( 'NONE', #22722 ) ;
#25391 = CARTESIAN_POINT ( 'NONE',  ( 190.1415007095349381, 49.99999999891522151, -12.70434618648777381 ) ) ;
#25392 = CARTESIAN_POINT ( 'NONE',  ( 103.1528011352953342, -3.152801135295355106, 5.062500001365592972 ) ) ;
#25393 = ORIENTED_EDGE ( 'NONE', *, *, #26948, .T. ) ;
#25394 = CARTESIAN_POINT ( 'NONE',  ( 108.0825317500000011, 107.3738262389971538, -48.47500000273118559 ) ) ;
#25395 = CARTESIAN_POINT ( 'NONE',  ( 13.14518615778179544, 32.21914062608393436, -1.609821015232357215E-15 ) ) ;
#25396 = CARTESIAN_POINT ( 'NONE',  ( 189.3771271284219608, 38.86679687716787868, 13.57481594606290720 ) ) ;
#25397 = ADVANCED_FACE ( 'NONE', ( #2769 ), #22293, .T. ) ;
#25398 = CARTESIAN_POINT ( 'NONE',  ( 13.14518615778179722, 40.20625000108393010, -5.444914386472297529 ) ) ;
#25399 = CARTESIAN_POINT ( 'NONE',  ( 97.50236033167492167, 102.3130555110000159, -46.72500000273119269 ) ) ;
#25400 = CARTESIAN_POINT ( 'NONE',  ( 135.4449143864723339, 39.71015625108393010, -13.14518615778179722 ) ) ;
#25401 = CARTESIAN_POINT ( 'NONE',  ( -13.14518615778179544, 39.95820312608393010, 0.000000000000000000 ) ) ;
#25402 = ORIENTED_EDGE ( 'NONE', *, *, #7577, .T. ) ;
#25403 = CARTESIAN_POINT ( 'NONE',  ( 74.59884440882045453, 37.52734375000000000, -9.598844408820458085 ) ) ;
#25404 = DIRECTION ( 'NONE',  ( 0.000000000000000000, 1.000000000000000000, 0.000000000000000000 ) ) ;
#25405 = CARTESIAN_POINT ( 'NONE',  ( 2.493653234604083739E-15, 37.32890625216786873, 13.57481594606304576 ) ) ;
#25406 = CARTESIAN_POINT ( 'NONE',  ( 103.1528011352953342, 3.152801135295383084, 5.062500001365592972 ) ) ;
#25407 = CARTESIAN_POINT ( 'NONE',  ( 9.295050272127047819, 33.90585937608393863, 9.295050272127046043 ) ) ;
#25408 = CARTESIAN_POINT ( 'NONE',  ( 104.4587341249999639, 1.442382525525748735E-14, 1.187500001365592750 ) ) ;
#25409 = CARTESIAN_POINT ( 'NONE',  ( 101.8468681455907046, 81.37500000136563472, -4.458734125000016313 ) ) ;
#25410 = CARTESIAN_POINT ( 'NONE',  ( -8.049105076161786076E-16, 34.00507812608393721, -13.14518615778179544 ) ) ;
#25411 = CARTESIAN_POINT ( 'NONE',  ( -9.295050272127046043, 39.85898437608393152, -9.295050272127046043 ) ) ;
#25412 = EDGE_CURVE ( 'NONE', #1080, #3022, #9449, .T. ) ;
#25413 = CARTESIAN_POINT ( 'NONE',  ( 58.88343976028321691, 54.66944451632674173, 14.99999999999998224 ) ) ;
#25414 = EDGE_LOOP ( 'NONE', ( #213, #12516, #4768, #13286 ) ) ;
#25415 = FILL_AREA_STYLE_COLOUR ( '', #15887 ) ;
#25416 = DIRECTION ( 'NONE',  ( 0.000000000000000000, -1.000000000000000000, 0.000000000000000000 ) ) ;
#25417 = CARTESIAN_POINT ( 'NONE',  ( 96.84719886470463734, 95.18749999863440792, 3.152801135295351997 ) ) ;
#25418 = CARTESIAN_POINT ( 'NONE',  ( 2.493653234604083739E-15, 31.77265625216787370, 13.57481594606304576 ) ) ;
#25419 = LINE ( 'NONE', #21007, #19429 ) ;
#25420 = CARTESIAN_POINT ( 'NONE',  ( 219.9999999999999716, 75.00000000000000000, -10.00000000000000000 ) ) ;
#25421 = EDGE_LOOP ( 'NONE', ( #26878, #2343 ) ) ;
#25422 = CARTESIAN_POINT ( 'NONE',  ( 65.00000000000000000, 36.98164062608393721, 13.14518615778179544 ) ) ;
#25423 = CARTESIAN_POINT ( 'NONE',  ( 94.99999999999995737, 79.56250000136559208, -1.387778780781445676E-14 ) ) ;
#25424 = AXIS2_PLACEMENT_3D ( 'NONE', #1958, #28035, #2242 ) ;
#25425 = FACE_OUTER_BOUND ( 'NONE', #3562, .T. ) ;
#25426 = ORIENTED_EDGE ( 'NONE', *, *, #20253, .F. ) ;
#25427 = CARTESIAN_POINT ( 'NONE',  ( 92.99999999999995737, 1.387778780781445676E-14, 34.79898987322334136 ) ) ;
#25428 = CARTESIAN_POINT ( 'NONE',  ( 100.0000000000000000, 110.0000000000000000, -55.00000000000000711 ) ) ;
#25429 = DIRECTION ( 'NONE',  ( 0.000000000000000000, -1.000000000000000000, -0.000000000000000000 ) ) ;
#25430 = CARTESIAN_POINT ( 'NONE',  ( -9.598844408820454532, 33.95546874999999432, 9.598844408820459861 ) ) ;
#25431 = CARTESIAN_POINT ( 'NONE',  ( 124.3771271284221314, 33.31054687716787299, 13.57481594606304753 ) ) ;
#25432 = CARTESIAN_POINT ( 'NONE',  ( 99.99999988184244160, 117.0000000000000000, -45.00000000000000711 ) ) ;
#25433 = FACE_BOUND ( 'NONE', #14672, .T. ) ;
#25434 = CARTESIAN_POINT ( 'NONE',  ( 181.8548138422182205, 37.57695312608393579, 0.000000000000000000 ) ) ;
#25435 = VERTEX_POINT ( 'NONE', #15995 ) ;
#25436 = VERTEX_POINT ( 'NONE', #24852 ) ;
#25437 = CARTESIAN_POINT ( 'NONE',  ( 87.00000000000000000, 123.0000000000000000, 12.99999999999999112 ) ) ;
#25438 = CARTESIAN_POINT ( 'NONE',  ( -13.57481594606304576, 40.20624999999999005, 0.000000000000000000 ) ) ;
#25439 = VECTOR ( 'NONE', #23530, 1000.000000000000000 ) ;
#25440 = CARTESIAN_POINT ( 'NONE',  ( 94.99999999999997158, 2.071067811865503483, 13.93749999999999467 ) ) ;
#25441 = CARTESIAN_POINT ( 'NONE',  ( 99.99999999999998579, 123.6000000000000085, 2.499999999999978684 ) ) ;
#25442 = CARTESIAN_POINT ( 'NONE',  ( 13.14518615778179544, 39.56132812608393579, -1.609821015232357215E-15 ) ) ;
#25443 = CYLINDRICAL_SURFACE ( 'NONE', #10341, 2.499999999999995115 ) ;
#25444 = VECTOR ( 'NONE', #2412, 999.9999999999998863 ) ;
#25445 = CARTESIAN_POINT ( 'NONE',  ( 7.065634988760085555, 36.00000000000000000, 11.21307450592249033 ) ) ;
#25446 = CARTESIAN_POINT ( 'NONE',  ( 195.0000000000000000, 50.00000000000000000, -2.255140518769849538E-14 ) ) ;
#25447 = CARTESIAN_POINT ( 'NONE',  ( 93.46109445667489979, 105.2492070361643215, -49.42499999726882010 ) ) ;
#25448 = ORIENTED_EDGE ( 'NONE', *, *, #25372, .F. ) ;
#25449 = UNCERTAINTY_MEASURE_WITH_UNIT (LENGTH_MEASURE( 1.000000000000000082E-05 ), #27860, 'distance_accuracy_value', 'NONE');
#25450 = CARTESIAN_POINT ( 'NONE',  ( -5.444914386472297529, 31.87187500108393223, -13.14518615778179900 ) ) ;
#25451 = CARTESIAN_POINT ( 'NONE',  ( -9.598844408820458085, 32.26875000216787726, -9.598844408820458085 ) ) ;
#25452 = CARTESIAN_POINT ( 'NONE',  ( 96.46446609406721961, 3.535533905932755072, 6.000000002731185056 ) ) ;
#25453 = CARTESIAN_POINT ( 'NONE',  ( 130.0000000000000000, 39.75976562608394005, -13.14518615778179544 ) ) ;
#25454 = CARTESIAN_POINT ( 'NONE',  ( 55.70494972787295751, 37.27929687608393294, -9.295050272127046043 ) ) ;
#25455 = DIRECTION ( 'NONE',  ( 0.8660254037844418162, -0.4999999999999947264, -0.000000000000000000 ) ) ;
#25456 = CARTESIAN_POINT ( 'NONE',  ( 9.295050272127046043, 34.69960937608393436, -9.295050272127046043 ) ) ;
#25457 = CARTESIAN_POINT ( 'NONE',  ( 181.8975291782780914, 36.00000000000001421, -1.608626461598034130 ) ) ;
#25458 =( BOUNDED_CURVE ( )  B_SPLINE_CURVE ( 2, ( #9106, #13068, #15508, #12929, #6406, #15075, #19515, #26212, #17800 ),
 .UNSPECIFIED., .F., .F. ) 
 B_SPLINE_CURVE_WITH_KNOTS ( ( 3, 2, 2, 2, 3 ),
 ( 0.4500000000000003997, 0.4750000000000003664, 0.5000000000000004441, 0.5250000000000004663, 0.5500000000000004885 ),
 .UNSPECIFIED. ) 
 CURVE ( )  GEOMETRIC_REPRESENTATION_ITEM ( )  RATIONAL_B_SPLINE_CURVE ( ( 0.9999999999999987788, 0.9238795325112879597, 1.000000000000000000, 0.9238795325112867385, 1.000000000000000000, 0.9238795325112867385, 1.000000000000000000, 0.9238795325112854062, 1.000000000000001332 ) ) 
 REPRESENTATION_ITEM ( '' )  );
#25459 = CARTESIAN_POINT ( 'NONE',  ( 55.40115559117954547, 37.72578124999999005, -9.598844408820458085 ) ) ;
#25460 = LINE ( 'NONE', #3799, #11705 ) ;
#25461 = EDGE_CURVE ( 'NONE', #778, #22877, #11451, .T. ) ;
#25462 = CARTESIAN_POINT ( 'NONE',  ( -20.00000000000000355, 75.00000000000000000, -14.99999999999999822 ) ) ;
#25463 = MECHANICAL_DESIGN_GEOMETRIC_PRESENTATION_REPRESENTATION (  '', ( #2261 ), #24551 ) ;
#25464 = CARTESIAN_POINT ( 'NONE',  ( 9.295050272127046043, 38.66835937608393436, -9.295050272127046043 ) ) ;
#25465 = CARTESIAN_POINT ( 'NONE',  ( 143.4541126562309046, 35.99999999999999289, 0.6772748633552372333 ) ) ;
#25466 = CARTESIAN_POINT ( 'NONE',  ( 102.4999999999999858, 123.7999999999999972, -9.847140817659276890E-15 ) ) ;
#25467 = FACE_OUTER_BOUND ( 'NONE', #26435, .T. ) ;
#25468 = CARTESIAN_POINT ( 'NONE',  ( 98.53841926354351699, 123.8500000010924680, -1.461580736456474794 ) ) ;
#25469 = FACE_OUTER_BOUND ( 'NONE', #875, .T. ) ;
#25470 = CARTESIAN_POINT ( 'NONE',  ( 96.84719886470459471, -3.152801135295355994, 11.56250000136559208 ) ) ;
#25471 = CARTESIAN_POINT ( 'NONE',  ( -8.312177448680279460E-16, 32.07031249999999289, -13.57481594606304576 ) ) ;
#25472 = VERTEX_POINT ( 'NONE', #24712 ) ;
#25473 = CARTESIAN_POINT ( 'NONE',  ( 99.99999999999998579, 102.6397644303321215, -53.50000000000000711 ) ) ;
#25474 = CARTESIAN_POINT ( 'NONE',  ( -8.312177448680279460E-16, 40.80156249999999574, -13.57481594606304576 ) ) ;
#25475 = CARTESIAN_POINT ( 'NONE',  ( 13.14518615778179722, 33.75703125108393010, 5.444914386472293977 ) ) ;
#25476 = CARTESIAN_POINT ( 'NONE',  ( 13.57481594606304931, 33.50898437716787015, 5.622872871577869525 ) ) ;
#25477 = CARTESIAN_POINT ( 'NONE',  ( 112.9999999999999858, 97.00000000000000000, -13.00000000000000711 ) ) ;
#25478 = CARTESIAN_POINT ( 'NONE',  ( 95.54126587499996504, 81.43750000136559208, -1.387778780781445676E-14 ) ) ;
#25479 = CARTESIAN_POINT ( 'NONE',  ( 59.55508561352770158, 36.93203125108394147, 13.14518615778179722 ) ) ;
#25480 = CARTESIAN_POINT ( 'NONE',  ( 93.46109445667491400, 114.7507929638356785, -47.57500000273119412 ) ) ;
#25481 = CARTESIAN_POINT ( 'NONE',  ( 104.9999999999999574, 2.071067811865501263, 11.56249999999999822 ) ) ;
#25482 = CARTESIAN_POINT ( 'NONE',  ( 98.53841926354351699, 123.0500000010924850, -1.461580736456474794 ) ) ;
#25483 = CARTESIAN_POINT ( 'NONE',  ( -13.57481594606304576, 40.99999999999999289, 0.000000000000000000 ) ) ;
#25484 = CARTESIAN_POINT ( 'NONE',  ( 104.3262379212492448, 115.9545556584642867, -51.19999999453763451 ) ) ;
#25485 = CARTESIAN_POINT ( 'NONE',  ( 120.7049497278729575, 32.91367187608393152, 9.295050272127047819 ) ) ;
#25486 = ORIENTED_EDGE ( 'NONE', *, *, #20539, .F. ) ;
#25487 = CARTESIAN_POINT ( 'NONE',  ( 1.417506129906585004E-15, 36.00000000000000000, -11.57481594606304398 ) ) ;
#25488 = CARTESIAN_POINT ( 'NONE',  ( -13.14518615778179900, 39.90859375108394147, -5.444914386472297529 ) ) ;
#25489 = CARTESIAN_POINT ( 'NONE',  ( 9.598844408820456309, 40.00781250216787299, -9.598844408820458085 ) ) ;
#25490 = CARTESIAN_POINT ( 'NONE',  ( 99.99999999999998579, 94.75000000000000000, 4.999999999999984013 ) ) ;
#25491 = CARTESIAN_POINT ( 'NONE',  ( 51.42518405393695957, 36.38632812716788578, 5.622872871577880183 ) ) ;
#25492 = CARTESIAN_POINT ( 'NONE',  ( 102.4976396683250783, 102.3130555110000159, -53.02499999726882862 ) ) ;
#25493 = CARTESIAN_POINT ( 'NONE',  ( -8.312177448680279460E-16, 34.55078125216787299, -13.57481594606304576 ) ) ;
#25494 = VERTEX_POINT ( 'NONE', #9173 ) ;
#25495 = CARTESIAN_POINT ( 'NONE',  ( 102.0710678118654329, 5.000000000000018652, 9.687499999999998224 ) ) ;
#25496 = CARTESIAN_POINT ( 'NONE',  ( 102.1631189606246295, 116.6573956140660897, -47.10000000546237686 ) ) ;
#25497 = CARTESIAN_POINT ( 'NONE',  ( 3.755639919285892248, 31.78804746655075419, -13.14518615778179544 ) ) ;
#25498 = CARTESIAN_POINT ( 'NONE',  ( 200.4449143864723055, 38.42031250108393436, 13.14518615778179189 ) ) ;
#25499 = EDGE_CURVE ( 'NONE', #13519, #5360, #7308, .T. ) ;
#25500 = DIRECTION ( 'NONE',  ( -0.000000000000000000, -1.000000000000000000, -0.000000000000000000 ) ) ;
#25501 = CARTESIAN_POINT ( 'NONE',  ( 116.8548138422182205, 38.22187500108393721, 5.444914386472304635 ) ) ;
#25502 = EDGE_CURVE ( 'NONE', #756, #12986, #26570, .T. ) ;
#25503 =( BOUNDED_CURVE ( )  B_SPLINE_CURVE ( 2, ( #11534, #18259, #14105, #22395, #26967, #16106, #5013, #3295, #9836 ),
 .UNSPECIFIED., .F., .F. ) 
 B_SPLINE_CURVE_WITH_KNOTS ( ( 3, 2, 2, 2, 3 ),
 ( 0.3541666666666666852, 0.3645833333333332593, 0.3749999999999998890, 0.3854166666666665741, 0.3958333333333331483 ),
 .UNSPECIFIED. ) 
 CURVE ( )  GEOMETRIC_REPRESENTATION_ITEM ( )  RATIONAL_B_SPLINE_CURVE ( ( 1.000000000000000000, 0.9238795325112867385, 1.000000000000000000, 0.9238795325112867385, 1.000000000000000000, 0.9238795325112867385, 1.000000000000000000, 0.9238795325112879597, 0.9999999999999987788 ) ) 
 REPRESENTATION_ITEM ( '' )  );
#25504 = CARTESIAN_POINT ( 'NONE',  ( 6.944426393311537993, 31.75150625057403175, -11.16113171639042356 ) ) ;
#25505 = CARTESIAN_POINT ( 'NONE',  ( 101.8468681455907330, 95.12499999863439371, 4.458734124999980786 ) ) ;
#25506 = DIRECTION ( 'NONE',  ( -0.000000000000000000, 1.000000000000000000, -0.000000000000000000 ) ) ;
#25507 = CARTESIAN_POINT ( 'NONE',  ( 13.14518615778179900, 40.10703125108393152, 5.444914386472293977 ) ) ;
#25508 = CARTESIAN_POINT ( 'NONE',  ( 195.0000000000000000, 37.22968749999999716, 13.57481594606304576 ) ) ;
#25509 = LINE ( 'NONE', #8118, #5530 ) ;
#25510 = CARTESIAN_POINT ( 'NONE',  ( 95.54126587499995082, 1.846868145590750077, 2.625000001365592084 ) ) ;
#25511 = CARTESIAN_POINT ( 'NONE',  ( 70.44491438647230552, 40.00781250108393294, 13.14518615778179189 ) ) ;
#25512 = AXIS2_PLACEMENT_3D ( 'NONE', #18108, #13677, #5150 ) ;
#25513 = CARTESIAN_POINT ( 'NONE',  ( 101.8468681455907046, -4.458734124999987891, 7.750000001365592084 ) ) ;
#25514 = CARTESIAN_POINT ( 'NONE',  ( 93.00000000000001421, 107.7255621263696668, -48.40000000546238113 ) ) ;
#25515 = CARTESIAN_POINT ( 'NONE',  ( 96.84719886470463734, 90.93749999863440792, 3.152801135295351997 ) ) ;
#25516 = CARTESIAN_POINT ( 'NONE',  ( 104.4587341249999781, 90.43749999863440792, -6.938893903907228378E-15 ) ) ;
#25517 = CARTESIAN_POINT ( 'NONE',  ( 13.57481594606304931, 39.75976562499999289, 5.622872871577869525 ) ) ;
#25518 = CARTESIAN_POINT ( 'NONE',  ( 143.1451861577818079, 40.35507812608393863, -1.609821015232357215E-15 ) ) ;
#25519 = ADVANCED_FACE ( 'NONE', ( #7022 ), #15717, .F. ) ;
#25520 = ORIENTED_EDGE ( 'NONE', *, *, #23099, .F. ) ;
#25521 = CARTESIAN_POINT ( 'NONE',  ( 104.4587341249999781, 82.12500000136560629, 1.846868145590721655 ) ) ;
#25522 = DIRECTION ( 'NONE',  ( -0.000000000000000000, 1.000000000000000000, -0.000000000000000000 ) ) ;
#25523 = ORIENTED_EDGE ( 'NONE', *, *, #17696, .T. ) ;
#25524 = APPLICATION_CONTEXT ( 'automotive_design' ) ;
#25525 = VERTEX_POINT ( 'NONE', #27148 ) ;
#25526 = CARTESIAN_POINT ( 'NONE',  ( 126.2025481310420076, 54.08938259242987101, -15.00000000000000178 ) ) ;
#25527 = CARTESIAN_POINT ( 'NONE',  ( 96.84719886470459471, 3.152801135295383084, 5.562500001365592972 ) ) ;
#25528 = VERTEX_POINT ( 'NONE', #24567 ) ;
#25529 = CARTESIAN_POINT ( 'NONE',  ( 95.00472066334982912, 116.8754121666685393, -49.67500000273118843 ) ) ;
#25530 = CARTESIAN_POINT ( 'NONE',  ( -9.295050272127044266, 32.71523437608393436, 9.295050272127047819 ) ) ;
#25531 = CARTESIAN_POINT ( 'NONE',  ( 189.3771271284221314, 37.27929687716787299, 13.57481594606304753 ) ) ;
#25532 = EDGE_CURVE ( 'NONE', #11020, #10899, #749, .T. ) ;
#25533 = CARTESIAN_POINT ( 'NONE',  ( -9.295050272127046043, 40.45429687608393721, -9.295050272127046043 ) ) ;
#25534 = LINE ( 'NONE', #8276, #2584 ) ;
#25535 = CARTESIAN_POINT ( 'NONE',  ( 195.3286002765670446, 53.49358765999039633, 14.99999999999994671 ) ) ;
#25536 = CARTESIAN_POINT ( 'NONE',  ( 139.2950502721270425, 38.07304687608393579, -9.295050272127046043 ) ) ;
#25537 = CARTESIAN_POINT ( 'NONE',  ( 13.14518615778179544, 33.01289062608393010, -1.609821015232357215E-15 ) ) ;
#25538 = ORIENTED_EDGE ( 'NONE', *, *, #324, .T. ) ;
#25539 = CARTESIAN_POINT ( 'NONE',  ( 55.40115559117954547, 37.72578124999999005, -9.598844408820458085 ) ) ;
#25540 = CARTESIAN_POINT ( 'NONE',  ( 84.99999999999998579, 125.0000000000000000, -15.00000000000000888 ) ) ;
#25541 = EDGE_CURVE ( 'NONE', #28082, #26002, #13714, .T. ) ;
#25542 = DIRECTION ( 'NONE',  ( -0.000000000000000000, 1.000000000000000000, -0.000000000000000000 ) ) ;
#25543 = CARTESIAN_POINT ( 'NONE',  ( 104.4587341249999781, 1.846868145590750299, 3.000000001365592528 ) ) ;
#25544 = CARTESIAN_POINT ( 'NONE',  ( 13.14518615778179544, 33.21132812608393436, -1.609821015232357215E-15 ) ) ;
#25545 = CARTESIAN_POINT ( 'NONE',  ( 103.1528011352953342, -3.152801135295355106, 4.062500001365592084 ) ) ;
#25546 = CARTESIAN_POINT ( 'NONE',  ( 98.15313185440923860, 83.50000000136560629, -4.458734125000016313 ) ) ;
#25547 = CARTESIAN_POINT ( 'NONE',  ( -13.14518615778179189, 31.87187500108393223, 5.444914386472304635 ) ) ;
#25548 = CARTESIAN_POINT ( 'NONE',  ( 9.295050272127047819, 38.66835937608393436, 9.295050272127046043 ) ) ;
#25549 = EDGE_CURVE ( 'NONE', #24847, #1889, #11290, .T. ) ;
#25550 = CARTESIAN_POINT ( 'NONE',  ( 61.13458562458681200, 54.10683252460148651, 14.99999999999998046 ) ) ;
#25551 = ORIENTED_EDGE ( 'NONE', *, *, #6983, .F. ) ;
#25552 = CARTESIAN_POINT ( 'NONE',  ( -5.444914386472297529, 32.66562500108393863, -13.14518615778179722 ) ) ;
#25553 = CARTESIAN_POINT ( 'NONE',  ( 100.8561741729129295, 123.5000000010924879, -2.066987299999998751 ) ) ;
#25554 = CARTESIAN_POINT ( 'NONE',  ( 84.99999999999998579, 123.0000000000000000, 12.99999999999999112 ) ) ;
#25555 = CARTESIAN_POINT ( 'NONE',  ( 208.1451861577818079, 36.38632812608393863, -1.609821015232357215E-15 ) ) ;
#25556 = CARTESIAN_POINT ( 'NONE',  ( 101.9373566580610628, 122.9999999999999858, -1.366919386427927874 ) ) ;
#25557 = CARTESIAN_POINT ( 'NONE',  ( -8.312177448680279460E-16, 32.07031249999999289, -13.57481594606304576 ) ) ;
#25558 = ORIENTED_EDGE ( 'NONE', *, *, #16966, .T. ) ;
#25559 = CARTESIAN_POINT ( 'NONE',  ( 78.14518615778179367, 39.56132812608393579, -1.609821015232357215E-15 ) ) ;
#25560 = CARTESIAN_POINT ( 'NONE',  ( 71.11656023971681861, 54.66944451632674884, -15.00000000000000000 ) ) ;
#25561 = ORIENTED_EDGE ( 'NONE', *, *, #12726, .T. ) ;
#25562 = CARTESIAN_POINT ( 'NONE',  ( 97.92893218813451028, 5.000000000000018652, 1.937500002731185500 ) ) ;
#25563 = CARTESIAN_POINT ( 'NONE',  ( 116.4251840539369596, 37.82499999999999574, 0.000000000000000000 ) ) ;
#25564 = CARTESIAN_POINT ( 'NONE',  ( 196.8875287258763649, 53.66306546785488507, 14.99999999999994671 ) ) ;
#25565 = CARTESIAN_POINT ( 'NONE',  ( 143.5748159460630404, 35.09648437716787583, 5.622872871577869525 ) ) ;
#25566 = CARTESIAN_POINT ( 'NONE',  ( 130.0000000000000000, 36.00000000000000000, -1.503427012513233026E-14 ) ) ;
#25567 = CARTESIAN_POINT ( 'NONE',  ( -8.312177448680279460E-16, 32.16953125216787157, -13.57481594606304576 ) ) ;
#25568 = EDGE_CURVE ( 'NONE', #27080, #11152, #27714, .T. ) ;
#25569 = CARTESIAN_POINT ( 'NONE',  ( 208.1451861577818079, 38.76757812608393294, -1.609821015232357215E-15 ) ) ;
#25570 = EDGE_LOOP ( 'NONE', ( #3309, #24324 ) ) ;
#25571 = ORIENTED_EDGE ( 'NONE', *, *, #16104, .T. ) ;
#25572 = FILL_AREA_STYLE ('',( #6462 ) ) ;
#25573 = CARTESIAN_POINT ( 'NONE',  ( 0.000000000000000000, 50.00000000000000000, 0.000000000000000000 ) ) ;
#25574 = CARTESIAN_POINT ( 'NONE',  ( 5.622872871577780707, 33.70742187716788152, -13.57481594606313990 ) ) ;
#25575 = DIRECTION ( 'NONE',  ( -0.000000000000000000, 1.000000000000000000, -0.000000000000000000 ) ) ;
#25576 = CARTESIAN_POINT ( 'NONE',  ( 2.493653234604083739E-15, 34.15390625216787157, 13.57481594606304576 ) ) ;
#25577 = CARTESIAN_POINT ( 'NONE',  ( -9.295050272127044266, 40.05742187608393579, 9.295050272127047819 ) ) ;
#25578 = CYLINDRICAL_SURFACE ( 'NONE', #10921, 5.000000000000004441 ) ;
#25579 = LINE ( 'NONE', #14313, #16203 ) ;
#25580 = CARTESIAN_POINT ( 'NONE',  ( 96.46446609406721961, 82.87500000000000000, -3.535533905932755072 ) ) ;
#25581 = CARTESIAN_POINT ( 'NONE',  ( 133.8783852973911905, 32.03609435653363136, -13.57481594606304576 ) ) ;
#25582 = ORIENTED_EDGE ( 'NONE', *, *, #26376, .F. ) ;
#25583 = CARTESIAN_POINT ( 'NONE',  ( 13.57481594606304576, 39.01562500000000000, -1.662435489736055892E-15 ) ) ;
#25584 = CARTESIAN_POINT ( 'NONE',  ( -5.444914386472299306, 39.11484375108394573, 13.14518615778179722 ) ) ;
#25585 = CARTESIAN_POINT ( 'NONE',  ( 104.9999999999999574, -2.071067811865462627, 0.5625000027311858330 ) ) ;
#25586 = CARTESIAN_POINT ( 'NONE',  ( 133.7556399192858976, 31.58960996655074993, -13.14518615778179544 ) ) ;
#25587 = CARTESIAN_POINT ( 'NONE',  ( 65.00000000000000000, 37.97382812608393721, -13.14518615778179544 ) ) ;
#25588 = CARTESIAN_POINT ( 'NONE',  ( 208.1451861577818079, 32.21914062608393436, -1.609821015232357215E-15 ) ) ;
#25589 = CYLINDRICAL_SURFACE ( 'NONE', #20254, 7.000000000000006217 ) ;
#25590 = CARTESIAN_POINT ( 'NONE',  ( -9.295050272127044266, 36.68398437608392726, 9.295050272127047819 ) ) ;
#25591 = CARTESIAN_POINT ( 'NONE',  ( 94.99999999999994316, -2.071067811865456409, 9.187500002731182391 ) ) ;
#25592 = CARTESIAN_POINT ( 'NONE',  ( 195.2703369776649254, 36.00000000000000000, 13.14949859323919412 ) ) ;
#25593 = CARTESIAN_POINT ( 'NONE',  ( 130.0000000000000000, 40.40468749999999432, 13.57481594606304576 ) ) ;
#25594 = CARTESIAN_POINT ( 'NONE',  ( 9.295050272127047819, 39.26367187608393294, 9.295050272127046043 ) ) ;
#25595 = CARTESIAN_POINT ( 'NONE',  ( 3.039397050802530753, 53.88964894337311762, 14.99999999999999645 ) ) ;
#25596 = CARTESIAN_POINT ( 'NONE',  ( 98.96446609406727646, 123.5499999999999972, 2.499999999999977796 ) ) ;
#25597 = CARTESIAN_POINT ( 'NONE',  ( 99.14382582708707048, 124.1000000010924964, 2.066987299999979211 ) ) ;
#25598 = CARTESIAN_POINT ( 'NONE',  ( 102.0669873000000081, 124.4000000010924651, -0.8561741729129508371 ) ) ;
#25599 = CARTESIAN_POINT ( 'NONE',  ( 96.84719886470459471, 3.152801135295383084, 14.31250000136559208 ) ) ;
#25600 = CARTESIAN_POINT ( 'NONE',  ( 102.0710678118654329, -4.999999999999989342, 13.43750000273118594 ) ) ;
#25601 = ORIENTED_EDGE ( 'NONE', *, *, #27805, .F. ) ;
#25602 = CARTESIAN_POINT ( 'NONE',  ( 102.1631189606246295, 103.3426043859339103, -53.40000000000001279 ) ) ;
#25603 = CARTESIAN_POINT ( 'NONE',  ( -5.444914386472297529, 31.87187500108393223, -13.14518615778179900 ) ) ;
#25604 = CARTESIAN_POINT ( 'NONE',  ( -5.444914386472299306, 31.97109375108393792, 13.14518615778179722 ) ) ;
#25605 = CIRCLE ( 'NONE', #25144, 13.57481594606304398 ) ;
#25606 = CARTESIAN_POINT ( 'NONE',  ( 9.598844408820456309, 33.65781250216787157, -9.598844408820458085 ) ) ;
#25607 = CARTESIAN_POINT ( 'NONE',  ( 103.5355339059327093, 3.535533905932755072, 2.624999999999998668 ) ) ;
#25608 = CARTESIAN_POINT ( 'NONE',  ( 98.15313185440925281, 81.62500000136560629, 4.458734124999987891 ) ) ;
#25609 = CARTESIAN_POINT ( 'NONE',  ( 51.85481384221820633, 38.42031250108393436, 5.444914386472304635 ) ) ;
#25610 = CARTESIAN_POINT ( 'NONE',  ( 93.46109445667491400, 105.2492070361643215, -51.17500000273119554 ) ) ;
#25611 = DIRECTION ( 'NONE',  ( 1.000000000000000000, 0.000000000000000000, 0.000000000000000000 ) ) ;
#25612 =( BOUNDED_CURVE ( )  B_SPLINE_CURVE ( 2, ( #2095, #19474, #10627, #26317, #10763, #4655, #98, #24034, #11179 ),
 .UNSPECIFIED., .F., .F. ) 
 B_SPLINE_CURVE_WITH_KNOTS ( ( 3, 2, 2, 2, 3 ),
 ( 0.1458333333333336757, 0.1562500000000002776, 0.1666666666666669072, 0.1770833333333335369, 0.1875000000000001388 ),
 .UNSPECIFIED. ) 
 CURVE ( )  GEOMETRIC_REPRESENTATION_ITEM ( )  RATIONAL_B_SPLINE_CURVE ( ( 0.9999999999999975575, 0.9238795325112891810, 1.000000000000000000, 0.9238795325112867385, 1.000000000000000000, 0.9238795325112867385, 1.000000000000000000, 0.9238795325112857393, 1.000000000000001110 ) ) 
 REPRESENTATION_ITEM ( '' )  );
#25613 = EDGE_LOOP ( 'NONE', ( #12387, #19833, #27547, #25217 ) ) ;
#25614 = CARTESIAN_POINT ( 'NONE',  ( 102.0669872999999797, 123.5500000010924708, -9.794112055954760458E-15 ) ) ;
#25615 = DIRECTION ( 'NONE',  ( 0.000000000000000000, 0.000000000000000000, 1.000000000000000000 ) ) ;
#25616 = CARTESIAN_POINT ( 'NONE',  ( 99.99999999999997158, 102.6397644303321215, -53.99999999453763877 ) ) ;
#25617 = CARTESIAN_POINT ( 'NONE',  ( 116.8548138422182205, 32.02070312608393010, 0.000000000000000000 ) ) ;
#25618 = ORIENTED_EDGE ( 'NONE', *, *, #11909, .F. ) ;
#25619 = CARTESIAN_POINT ( 'NONE',  ( 94.99999999999995737, 1.387778780781445676E-14, 8.000000000000000000 ) ) ;
#25620 = EDGE_CURVE ( 'NONE', #13072, #6002, #19704, .T. ) ;
#25621 = CARTESIAN_POINT ( 'NONE',  ( 9.295050272127047819, 38.66835937608393436, 9.295050272127046043 ) ) ;
#25622 = CARTESIAN_POINT ( 'NONE',  ( -5.622872871577873077, 40.15664062716787441, -13.57481594606304753 ) ) ;
#25623 = CARTESIAN_POINT ( 'NONE',  ( 120.7049497278729575, 40.45429687608393721, -9.295050272127046043 ) ) ;
#25624 = CARTESIAN_POINT ( 'NONE',  ( 51.42518405393695957, 38.66835937716786731, -5.622872871577873077 ) ) ;
#25625 = CARTESIAN_POINT ( 'NONE',  ( 97.50236033167490746, 117.6869444889999841, -54.02499999726882862 ) ) ;
#25626 = CARTESIAN_POINT ( 'NONE',  ( 13.57481594606304576, 35.93984375216787441, -1.662435489736055892E-15 ) ) ;
#25627 = ORIENTED_EDGE ( 'NONE', *, *, #1184, .T. ) ;
#25628 = VECTOR ( 'NONE', #9734, 1000.000000000000000 ) ;
#25629 = CARTESIAN_POINT ( 'NONE',  ( 104.9999999999999574, -2.071067811865462627, 3.437499999999999556 ) ) ;
#25630 = CARTESIAN_POINT ( 'NONE',  ( 102.1631189606246295, 116.6573956140660897, -52.60000000000000853 ) ) ;
#25631 = CARTESIAN_POINT ( 'NONE',  ( 181.8548138422181921, 38.91640625108393436, -5.444914386472297529 ) ) ;
#25632 = CARTESIAN_POINT ( 'NONE',  ( 124.5550856135277087, 38.02343750108394005, -13.14518615778179722 ) ) ;
#25633 = DIRECTION ( 'NONE',  ( 0.000000000000000000, 0.000000000000000000, 1.000000000000000000 ) ) ;
#25634 = CARTESIAN_POINT ( 'NONE',  ( 94.99999999999995737, 1.387778780781445676E-14, 11.00000000000000000 ) ) ;
#25635 = CARTESIAN_POINT ( 'NONE',  ( 101.8468681455907330, 93.49999999863440792, -4.458734124999994997 ) ) ;
#25636 = CARTESIAN_POINT ( 'NONE',  ( 107.0000000000000000, 110.0000000000000000, -48.00000000000001421 ) ) ;
#25637 = CARTESIAN_POINT ( 'NONE',  ( -5.444914386472299306, 38.32109375108394289, 13.14518615778179722 ) ) ;
#25638 = CARTESIAN_POINT ( 'NONE',  ( 200.6228728715778686, 37.57695312499998863, -13.57481594606304753 ) ) ;
#25639 = ITEM_DEFINED_TRANSFORMATION ( 'NONE', 'NONE', #21786,  #26844 ) ;
#25640 = CARTESIAN_POINT ( 'NONE',  ( 125.2199608011490284, 36.00000000000002842, 12.25280873422854278 ) ) ;
#25641 = CARTESIAN_POINT ( 'NONE',  ( 104.4587341249999639, 1.442382525525748735E-14, 2.187500001365592084 ) ) ;
#25642 = CARTESIAN_POINT ( 'NONE',  ( 51.85481384221820633, 39.80937500108392868, 5.444914386472304635 ) ) ;
#25643 = CARTESIAN_POINT ( 'NONE',  ( 96.84719886470459471, -3.152801135295355994, 4.562500001365592084 ) ) ;
#25644 = DIRECTION ( 'NONE',  ( 0.000000000000000000, 1.000000000000000000, 0.000000000000000000 ) ) ;
#25645 = CARTESIAN_POINT ( 'NONE',  ( 95.54126587499999346, 94.12499999863439371, 1.846868145590722543 ) ) ;
#25646 = CARTESIAN_POINT ( 'NONE',  ( 1.417506129906585201E-15, 36.00000000000000000, 11.57481594606304576 ) ) ;
#25647 = CARTESIAN_POINT ( 'NONE',  ( 13.57481594606304753, 40.65273437499998721, -5.622872871577873077 ) ) ;
#25648 = CARTESIAN_POINT ( 'NONE',  ( 139.2950502721270425, 39.66054687608393436, -9.295050272127046043 ) ) ;
#25649 = ORIENTED_EDGE ( 'NONE', *, *, #22584, .T. ) ;
#25650 = CARTESIAN_POINT ( 'NONE',  ( 95.54126587499996504, 84.68750000136560629, -1.387778780781445676E-14 ) ) ;
#25651 = AXIS2_PLACEMENT_3D ( 'NONE', #27475, #18499, #16628 ) ;
#25652 = CARTESIAN_POINT ( 'NONE',  ( 95.54126587499999346, 91.74999999863439371, -1.846868145590737864 ) ) ;
#25653 = ORIENTED_EDGE ( 'NONE', *, *, #16443, .F. ) ;
#25654 = EDGE_CURVE ( 'NONE', #5311, #138, #13442, .T. ) ;
#25655 = CYLINDRICAL_SURFACE ( 'NONE', #10193, 0.5000000000000086597 ) ;
#25656 = CARTESIAN_POINT ( 'NONE',  ( 65.00000000000000000, 34.99726562608393721, -13.14518615778179544 ) ) ;
#25657 = ORIENTED_EDGE ( 'NONE', *, *, #984, .F. ) ;
#25658 = LINE ( 'NONE', #14806, #25439 ) ;
#25659 = CARTESIAN_POINT ( 'NONE',  ( 95.54126587499995082, -1.846868145590724986, 7.750000001365592084 ) ) ;
#25660 = VERTEX_POINT ( 'NONE', #11997 ) ;
#25661 = CARTESIAN_POINT ( 'NONE',  ( 5.444914386472302859, 34.65000000108393863, 13.14518615778179189 ) ) ;
#25662 =( BOUNDED_CURVE ( )  B_SPLINE_CURVE ( 2, ( #14044, #11190, #7493, #9634, #18340, #11477, #20194, #679, #4809, #393, #20485 ),
 .UNSPECIFIED., .F., .F. ) 
 B_SPLINE_CURVE_WITH_KNOTS ( ( 3, 2, 2, 2, 2, 3 ),
 ( 0.5999999999999998668, 0.6199999999999998845, 0.6399999999999999023, 0.6599999999999999201, 0.6799999999999999378, 0.6999999999999998446 ),
 .UNSPECIFIED. ) 
 CURVE ( )  GEOMETRIC_REPRESENTATION_ITEM ( )  RATIONAL_B_SPLINE_CURVE ( ( 1.000000000000000222, 0.9510565162951533091, 1.000000000000000000, 0.9510565162951535312, 1.000000000000000000, 0.9510565162951535312, 1.000000000000000000, 0.9510565162951535312, 1.000000000000000000, 0.9510565162951537532, 0.9999999999999997780 ) ) 
 REPRESENTATION_ITEM ( '' )  );
#25663 = CARTESIAN_POINT ( 'NONE',  ( 5.444914386472297529, 32.36796875108393579, -13.14518615778179900 ) ) ;
#25664 = CARTESIAN_POINT ( 'NONE',  ( 181.4251840539369596, 37.92421875216787441, 0.000000000000000000 ) ) ;
#25665 = CARTESIAN_POINT ( 'NONE',  ( 13.14518615778179544, 39.36289062608393152, -1.609821015232357215E-15 ) ) ;
#25666 = CARTESIAN_POINT ( 'NONE',  ( 65.00000000000000000, 36.13828125216787157, -13.57481594606304576 ) ) ;
#25667 = CARTESIAN_POINT ( 'NONE',  ( 198.8030543732578224, 54.09082899096448926, 14.99999999999994671 ) ) ;
#25668 = CARTESIAN_POINT ( 'NONE',  ( 135.4449143864723339, 38.91640625108393436, -13.14518615778179722 ) ) ;
#25669 = CARTESIAN_POINT ( 'NONE',  ( 13.14518615778179900, 38.02343750108395426, -5.444914386472297529 ) ) ;
#25670 = EDGE_LOOP ( 'NONE', ( #27665, #24520, #7862, #4250, #12254, #19537 ) ) ;
#25671 = CARTESIAN_POINT ( 'NONE',  ( 65.00000000000000000, 38.42031249999999432, -13.57481594606304576 ) ) ;
#25672 = CARTESIAN_POINT ( 'NONE',  ( 92.99999999999998579, 110.0000000000000000, -55.74999999726883004 ) ) ;
#25673 = CARTESIAN_POINT ( 'NONE',  ( 100.0000000000000000, 110.0000000000000000, -55.00000000000000711 ) ) ;
#25674 = EDGE_CURVE ( 'NONE', #2105, #6018, #19292, .T. ) ;
#25675 = AXIS2_PLACEMENT_3D ( 'NONE', #14801, #12520, #12802 ) ;
#25676 = CARTESIAN_POINT ( 'NONE',  ( 96.84719886470459471, 3.152801135295383084, 5.312500001365592972 ) ) ;
#25677 = CARTESIAN_POINT ( 'NONE',  ( 104.4587341249999781, -1.846868145590721655, 2.125000001365591640 ) ) ;
#25678 = DIRECTION ( 'NONE',  ( 0.000000000000000000, 1.000000000000000000, 0.000000000000000000 ) ) ;
#25679 = CARTESIAN_POINT ( 'NONE',  ( 91.91746824999998466, 110.0000000000000000, -45.62499999726882294 ) ) ;
#25680 = CARTESIAN_POINT ( 'NONE',  ( 96.46446609406721961, 3.535533905932755072, 8.000000002731185944 ) ) ;
#25681 = DIRECTION ( 'NONE',  ( 0.000000000000000000, 0.000000000000000000, 1.000000000000000000 ) ) ;
#25682 = ORIENTED_EDGE ( 'NONE', *, *, #18560, .T. ) ;
#25684 = ADVANCED_FACE ( 'NONE', ( #14141 ), #25263, .F. ) ;
#25683 = DIRECTION ( 'NONE',  ( 0.000000000000000000, 0.000000000000000000, -1.000000000000000000 ) ) ;
#25685 = DIRECTION ( 'NONE',  ( 0.000000000000000000, 0.000000000000000000, -1.000000000000000000 ) ) ;
#25686 = CARTESIAN_POINT ( 'NONE',  ( 97.92893218813451028, 82.31250000273122680, 4.999999999999989342 ) ) ;
#25687 = CARTESIAN_POINT ( 'NONE',  ( 99.99999999999997158, 101.5015231886685854, -55.37499999726883004 ) ) ;
#25688 = EDGE_CURVE ( 'NONE', #14776, #25390, #7600, .T. ) ;
#25689 = VERTEX_POINT ( 'NONE', #18579 ) ;
#25690 = CARTESIAN_POINT ( 'NONE',  ( 78.14518615778180788, 38.71796875108393721, 5.444914386472293977 ) ) ;
#25691 = EDGE_CURVE ( 'NONE', #4294, #9852, #21134, .T. ) ;
#25692 = CARTESIAN_POINT ( 'NONE',  ( 94.99999999999995737, 83.18750000273119838, 2.071067811865466624 ) ) ;
#25693 = CARTESIAN_POINT ( 'NONE',  ( -13.57481594606304576, 39.41249999999999432, 0.000000000000000000 ) ) ;
#25694 = VERTEX_POINT ( 'NONE', #10423 ) ;
#25695 = CARTESIAN_POINT ( 'NONE',  ( 102.1631189606246295, 116.6573956140660897, -52.60000000000000853 ) ) ;
#25696 = AXIS2_PLACEMENT_3D ( 'NONE', #3372, #1662, #27740 ) ;
#25697 = CARTESIAN_POINT ( 'NONE',  ( -9.180175813648018490, 55.00000000000000000, -15.00000000000000000 ) ) ;
#25698 = CARTESIAN_POINT ( 'NONE',  ( 94.99999999999995737, 81.18750000273119838, 2.071067811865466624 ) ) ;
#25699 = EDGE_CURVE ( 'NONE', #24259, #11568, #14325, .T. ) ;
#25700 = CARTESIAN_POINT ( 'NONE',  ( 130.0000000000000000, 35.74140625216787015, 13.57481594606304576 ) ) ;
#25701 =( BOUNDED_CURVE ( )  B_SPLINE_CURVE ( 1, ( #27064, #15492 ),
 .UNSPECIFIED., .F., .F. ) 
 B_SPLINE_CURVE_WITH_KNOTS ( ( 2, 2 ),
 ( 0.000000000000000000, 1.000000000000000000 ),
 .UNSPECIFIED. ) 
 CURVE ( )  GEOMETRIC_REPRESENTATION_ITEM ( )  RATIONAL_B_SPLINE_CURVE ( ( 0.9684275698016389100, 0.9684275698016389100 ) ) 
 REPRESENTATION_ITEM ( '' )  );
#25702 = B_SPLINE_CURVE_WITH_KNOTS ( 'NONE', 3,
 ( #4705, #15804, #4851, #26074, #13221, #6543, #15223, #8972, #19661, #26222, #4422, #13515, #17519, #2715, #2572, #17660, #10950, #11375, #13076, #8829, #6681, #15367, #24083, #4559, #21953, #2431, #19803, #287, #26368, #16519, #20804 ),
 .UNSPECIFIED., .F., .F.,
 ( 4, 2, 2, 2, 2, 2, 2, 2, 2, 2, 1, 2, 2, 2, 2, 4 ),
 ( 0.000000000000000000, 0.001656255954913766690, 0.003312511909827533380, 0.004968767864741300069, 0.005796895842198182547, 0.006625023819655066759, 0.008281279774568852531, 0.009937535729482641772, 0.01325004763931021852, 0.01490630359422400603, 0.01656255954913779180, 0.01821881550405158104, 0.01987507145896536681, 0.02318758336879294182, 0.02484383932370672760, 0.02650009527862051337 ),
 .UNSPECIFIED. ) ;
#25703 = CARTESIAN_POINT ( 'NONE',  ( 78.14518615778179367, 40.30546875108393579, 5.444914386472293977 ) ) ;
#25704 = DIRECTION ( 'NONE',  ( -0.000000000000000000, 1.000000000000000000, -0.000000000000000000 ) ) ;
#25705 = CARTESIAN_POINT ( 'NONE',  ( 181.8548138422181921, 36.03906250108394005, 5.444914386472304635 ) ) ;
#25706 = ORIENTED_EDGE ( 'NONE', *, *, #6175, .F. ) ;
#25707 = ORIENTED_EDGE ( 'NONE', *, *, #16663, .T. ) ;
#25708 = ORIENTED_EDGE ( 'NONE', *, *, #7065, .F. ) ;
#25709 = CARTESIAN_POINT ( 'NONE',  ( -5.444914386472297529, 33.26093750108393721, -13.14518615778179900 ) ) ;
#25710 = DIRECTION ( 'NONE',  ( 0.000000000000000000, 1.000000000000000000, 3.469446951953611231E-16 ) ) ;
#25711 = EDGE_CURVE ( 'NONE', #14663, #19205, #21000, .T. ) ;
#25712 = CARTESIAN_POINT ( 'NONE',  ( 95.54126587499996504, 83.43750000136560629, -1.387778780781445676E-14 ) ) ;
#25713 = CYLINDRICAL_SURFACE ( 'NONE', #18068, 2.999999999999989786 ) ;
#25714 = DIRECTION ( 'NONE',  ( -1.000000000000000000, 0.000000000000000000, -0.000000000000000000 ) ) ;
#25715 = AXIS2_PLACEMENT_3D ( 'NONE', #14954, #1738, #17387 ) ;
#25716 = CARTESIAN_POINT ( 'NONE',  ( 11.20653150213496296, 36.00000000000000000, 7.323573988461853368 ) ) ;
#25717 = CARTESIAN_POINT ( 'NONE',  ( 93.46109445667489979, 105.2492070361643215, -47.42499999726882720 ) ) ;
#25718 = ORIENTED_EDGE ( 'NONE', *, *, #18399, .F. ) ;
#25719 = EDGE_CURVE ( 'NONE', #1494, #2719, #4706, .T. ) ;
#25720 = CARTESIAN_POINT ( 'NONE',  ( -13.57481594606304576, 39.41249999999999432, 0.000000000000000000 ) ) ;
#25721 = CARTESIAN_POINT ( 'NONE',  ( -13.14518615778179544, 39.75976562608393294, 0.000000000000000000 ) ) ;
#25722 = CARTESIAN_POINT ( 'NONE',  ( 102.0710678118654329, -4.999999999999989342, 1.437500002731185056 ) ) ;
#25723 = CARTESIAN_POINT ( 'NONE',  ( 143.1451861577818079, 35.54296875108394715, 5.444914386472293977 ) ) ;
#25724 = CARTESIAN_POINT ( 'NONE',  ( 55.70494972787295751, 36.68398437608392726, 9.295050272127047819 ) ) ;
#25725 = ADVANCED_FACE ( 'NONE', ( #3887 ), #21275, .T. ) ;
#25726 = CARTESIAN_POINT ( 'NONE',  ( 198.7556399192858976, 31.58960996655074993, -13.14518615778179544 ) ) ;
#25727 = CARTESIAN_POINT ( 'NONE',  ( 57.93163431200125757, 35.99999999999999289, 11.09140360074102993 ) ) ;
#25728 = CARTESIAN_POINT ( 'NONE',  ( -13.14518615778179900, 36.53515625108392584, -5.444914386472297529 ) ) ;
#25729 = CARTESIAN_POINT ( 'NONE',  ( 131.6025331306099986, 53.60343507247939954, -15.00000000000000000 ) ) ;
#25730 = DIRECTION ( 'NONE',  ( 0.000000000000000000, 0.000000000000000000, -1.000000000000000000 ) ) ;
#25731 = CARTESIAN_POINT ( 'NONE',  ( -18.00000000000000711, 52.00000000000000711, -12.99999999999999822 ) ) ;
#25732 = AXIS2_PLACEMENT_3D ( 'NONE', #4884, #21847, #26402 ) ;
#25733 = CARTESIAN_POINT ( 'NONE',  ( -5.444914386472297529, 37.22968750108393721, -13.14518615778179900 ) ) ;
#25734 = CARTESIAN_POINT ( 'NONE',  ( -13.57481594606304753, 34.60039062499999574, -5.622872871577872189 ) ) ;
#25735 = CARTESIAN_POINT ( 'NONE',  ( 97.50000000000000000, 123.3569999999781572, -1.035533905932742416 ) ) ;
#25736 = CARTESIAN_POINT ( 'NONE',  ( 99.14382582708707048, 122.8000000010924708, -2.066987299999999195 ) ) ;
#25737 = CARTESIAN_POINT ( 'NONE',  ( 97.93301270000000613, 124.7000000010924765, -0.8561741729129506151 ) ) ;
#25738 = SHAPE_REPRESENTATION_RELATIONSHIP ( 'NONE' , 'NONE' ,  #9145, #11047 ) ;
#25739 = VERTEX_POINT ( 'NONE', #8715 ) ;
#25740 = CARTESIAN_POINT ( 'NONE',  ( 103.1528011352953342, -3.152801135295355106, 12.81250000136559208 ) ) ;
#25741 = CARTESIAN_POINT ( 'NONE',  ( -13.57481594606304753, 32.21914062500000142, -5.622872871577873077 ) ) ;
#25742 = VECTOR ( 'NONE', #1035, 1000.000000000000000 ) ;
#25743 = ORIENTED_EDGE ( 'NONE', *, *, #26938, .F. ) ;
#25744 = DIRECTION ( 'NONE',  ( -0.000000000000000000, -1.000000000000000000, -0.000000000000000000 ) ) ;
#25745 = CARTESIAN_POINT ( 'NONE',  ( 99.99999999999995737, 4.458734125000016313, 12.18750000136559208 ) ) ;
#25746 = CARTESIAN_POINT ( 'NONE',  ( 5.444914386472302859, 33.65781250108393152, 13.14518615778179189 ) ) ;
#25747 = CARTESIAN_POINT ( 'NONE',  ( -5.444914386472297529, 40.40468750108393436, -13.14518615778179900 ) ) ;
#25748 = DIRECTION ( 'NONE',  ( 0.000000000000000000, -0.000000000000000000, 1.000000000000000000 ) ) ;
#25749 = CARTESIAN_POINT ( 'NONE',  ( 103.1528011352953342, 84.31250000136560629, -3.152801135295383084 ) ) ;
#25750 = CARTESIAN_POINT ( 'NONE',  ( 78.14518615778179367, 38.76757812608393294, -1.609821015232357215E-15 ) ) ;
#25751 = CARTESIAN_POINT ( 'NONE',  ( 97.50236033167492167, 117.6869444889999841, -49.77500000273119696 ) ) ;
#25752 = CARTESIAN_POINT ( 'NONE',  ( 5.444914386472297529, 40.30546875108393579, -13.14518615778179722 ) ) ;
#25753 = CARTESIAN_POINT ( 'NONE',  ( 97.93301269999999192, 124.7000000010924623, -0.8561741729129505041 ) ) ;
#25754 = FACE_OUTER_BOUND ( 'NONE', #7421, .T. ) ;
#25755 = CARTESIAN_POINT ( 'NONE',  ( 102.1631189606246295, 103.3426043859339103, -51.89999999453764445 ) ) ;
#25756 = CARTESIAN_POINT ( 'NONE',  ( 116.4251840539369596, 40.99999999999999289, 0.000000000000000000 ) ) ;
#25757 = ORIENTED_EDGE ( 'NONE', *, *, #11777, .T. ) ;
#25758 = CARTESIAN_POINT ( 'NONE',  ( 65.00000000000000000, 50.00000000000000000, -7.517135062566165128E-15 ) ) ;
#25759 = CARTESIAN_POINT ( 'NONE',  ( -13.14518615778179544, 39.16445312608393436, 0.000000000000000000 ) ) ;
#25760 = CARTESIAN_POINT ( 'NONE',  ( -9.598844408820454532, 39.61093750216787868, 9.598844408820459861 ) ) ;
#25761 = CARTESIAN_POINT ( 'NONE',  ( 130.0000000000000000, 35.98945312608393010, 13.14518615778179544 ) ) ;
#25762 = CARTESIAN_POINT ( 'NONE',  ( 78.57481594606304043, 36.68398437716788152, 5.622872871577869525 ) ) ;
#25763 = CARTESIAN_POINT ( 'NONE',  ( 106.5389055433250860, 105.2492070361643215, -50.82499999726882578 ) ) ;
#25764 = CARTESIAN_POINT ( 'NONE',  ( 9.598844408820459861, 34.25312500216787015, 9.598844408820456309 ) ) ;
#25765 = AXIS2_PLACEMENT_3D ( 'NONE', #10909, #8509, #10632 ) ;
#25766 = EDGE_LOOP ( 'NONE', ( #27118, #4920, #23176, #15261, #6373, #17131, #17868, #251, #326, #25238, #2492, #20019, #19342, #26093, #11551 ) ) ;
#25767 = CARTESIAN_POINT ( 'NONE',  ( 97.92893218813451028, -4.999999999999989342, 4.187499999999998224 ) ) ;
#25768 = ORIENTED_EDGE ( 'NONE', *, *, #26932, .F. ) ;
#25769 = CARTESIAN_POINT ( 'NONE',  ( 208.1451861577817795, 37.82500000108392868, -5.444914386472297529 ) ) ;
#25770 = CARTESIAN_POINT ( 'NONE',  ( -5.622872871577964560, 38.46992187499999005, -13.57481594606295339 ) ) ;
#25771 = CARTESIAN_POINT ( 'NONE',  ( 124.5550856135277087, 39.61093750108393152, -13.14518615778179722 ) ) ;
#25772 = CARTESIAN_POINT ( 'NONE',  ( 9.598844408820456309, 35.93984374999999432, -9.598844408820458085 ) ) ;
#25773 = LINE ( 'NONE', #26196, #7687 ) ;
#25774 = CARTESIAN_POINT ( 'NONE',  ( 104.4587341249999923, 94.37499999863440792, -1.846868145590737198 ) ) ;
#25775 =( BOUNDED_SURFACE ( )  B_SPLINE_SURFACE ( 1, 2, ( 
 ( #27295, #25136, #28084, #8547, #14292, #20592, #21250, #14803, #16302, #1075, #23526, #1732, #10396, #4004, #12670, #21395, #1873, #10537, #6970, #17380, #17810, #13222, #2433, #431, #6828, #26513, #15082, #13367, #11235, #2147, #4852, #19953, #12937, #26369, #9115, #17663, #17950, #24226, #17521, #19524, #21670, #10809, #4560, #5, #4280, #24364, #22096, #15226, #22238, #15518, #15665, #2717, #11378, #13517, #20099, #26078, #15369, #576, #8690, #24086, #21954, #6546, #9257, #6413, #23944, #2574, #23802, #4424, #13078, #21817, #6683, #2293, #10952, #19663, #4707, #146, #8831, #26224, #11093, #19805, #289, #8974, #24510, #20670, #13661, #13940, #14228, #1154, #24934, #16377, #3277, #9540, #25077, #20529, #24658, #2848, #24792, #18090, #7392, #4998, #18241 ),
 ( #26660, #718, #11946, #20805, #11806, #5565, #5274, #22521, #3412, #14090, #7252, #11517, #22376, #9819, #1285, #22666, #5421, #3138, #26949, #15942, #16086, #27231, #18526, #5131, #1011, #7685, #22950, #9680, #12081, #18383, #9953, #27088, #13797, #7539, #16237, #7107, #22809, #2986, #15805, #11660, #20236, #9393, #26802, #20382, #868, #10505, #1974, #25356, #1702, #19211, #27368, #23494, #25763, #27504, #16793, #10221, #12492, #7960, #21493, #7827, #23635, #6245, #14914, #12361, #27639, #25213, #16659, #8375, #18666, #20944, #3974, #12777, #3830, #17060, #25492, #14506, #4111, #6107, #5837, #23084, #5701, #12634, #16520, #5972, #25625, #23357, #18931, #23223, #8100, #27914, #21361, #3699, #1568, #1842, #14368, #14639, #3558, #21218, #12216, #10360, #21079 ) ),
 .UNSPECIFIED., .F., .F., .T. ) 
 B_SPLINE_SURFACE_WITH_KNOTS ( ( 2, 2 ),
 ( 3, 2, 2, 2, 2, 2, 2, 2, 2, 2, 2, 2, 2, 2, 2, 2, 2, 2, 2, 2, 2, 2, 2, 2, 2, 2, 2, 2, 2, 2, 2, 2, 2, 2, 2, 2, 2, 2, 2, 2, 2, 2, 2, 2, 2, 2, 2, 2, 2, 2, 3 ),
 ( 0.000000000000000000, 1.000000000000000000 ),
 ( 0.000000000000000000, 0.02000000000000000042, 0.04000000000000000083, 0.05999999999999999778, 0.08000000000000000167, 0.1000000000000000056, 0.1199999999999999956, 0.1400000000000000133, 0.1600000000000000033, 0.1799999999999999933, 0.2000000000000000111, 0.2200000000000000011, 0.2399999999999999911, 0.2600000000000000089, 0.2800000000000000266, 0.2999999999999999889, 0.3200000000000000067, 0.3400000000000000244, 0.3599999999999999867, 0.3800000000000000044, 0.4000000000000000222, 0.4199999999999999845, 0.4400000000000000022, 0.4600000000000000200, 0.4799999999999999822, 0.5000000000000000000, 0.5200000000000000178, 0.5400000000000000355, 0.5600000000000000533, 0.5799999999999999600, 0.5999999999999999778, 0.6199999999999999956, 0.6400000000000000133, 0.6600000000000000311, 0.6800000000000000488, 0.6999999999999999556, 0.7199999999999999734, 0.7399999999999999911, 0.7600000000000000089, 0.7800000000000000266, 0.8000000000000000444, 0.8199999999999999512, 0.8399999999999999689, 0.8599999999999999867, 0.8800000000000000044, 0.9000000000000000222, 0.9200000000000000400, 0.9399999999999999467, 0.9599999999999999645, 0.9799999999999999822, 1.000000000000000000 ),
 .UNSPECIFIED. ) 
 GEOMETRIC_REPRESENTATION_ITEM ( )  RATIONAL_B_SPLINE_SURFACE ( (
 ( 1.000000000000000000, 0.9510565162951535312, 1.000000000000000000, 0.9510565162951535312, 1.000000000000000000, 0.9510565162951535312, 1.000000000000000000, 0.9510565162951535312, 1.000000000000000000, 0.9510565162951535312, 1.000000000000000000, 0.9510565162951535312, 1.000000000000000000, 0.9510565162951535312, 1.000000000000000000, 0.9510565162951535312, 1.000000000000000000, 0.9510565162951535312, 1.000000000000000000, 0.9510565162951535312, 1.000000000000000000, 0.9510565162951535312, 1.000000000000000000, 0.9510565162951535312, 1.000000000000000000, 0.9510565162951535312, 1.000000000000000000, 0.9510565162951535312, 1.000000000000000000, 0.9510565162951535312, 1.000000000000000000, 0.9510565162951535312, 1.000000000000000000, 0.9510565162951535312, 1.000000000000000000, 0.9510565162951535312, 1.000000000000000000, 0.9510565162951535312, 1.000000000000000000, 0.9510565162951535312, 1.000000000000000000, 0.9510565162951535312, 1.000000000000000000, 0.9510565162951535312, 1.000000000000000000, 0.9510565162951535312, 1.000000000000000000, 0.9510565162951535312, 1.000000000000000000, 0.9510565162951535312, 1.000000000000000000, 0.9510565162951535312, 1.000000000000000000, 0.9510565162951535312, 1.000000000000000000, 0.9510565162951535312, 1.000000000000000000, 0.9510565162951535312, 1.000000000000000000, 0.9510565162951535312, 1.000000000000000000, 0.9510565162951535312, 1.000000000000000000, 0.9510565162951535312, 1.000000000000000000, 0.9510565162951535312, 1.000000000000000000, 0.9510565162951535312, 1.000000000000000000, 0.9510565162951535312, 1.000000000000000000, 0.9510565162951535312, 1.000000000000000000, 0.9510565162951535312, 1.000000000000000000, 0.9510565162951535312, 1.000000000000000000, 0.9510565162951535312, 1.000000000000000000, 0.9510565162951535312, 1.000000000000000000, 0.9510565162951535312, 1.000000000000000000, 0.9510565162951535312, 1.000000000000000000, 0.9510565162951535312, 1.000000000000000000, 0.9510565162951535312, 1.000000000000000000, 0.9510565162951535312, 1.000000000000000000, 0.9510565162951535312, 1.000000000000000000, 0.9510565162951535312, 1.000000000000000000, 0.9510565162951535312, 1.000000000000000000, 0.9510565162951535312, 1.000000000000000000, 0.9510565162951535312, 1.000000000000000000),
 ( 1.000000000000000000, 0.9510565162951535312, 1.000000000000000000, 0.9510565162951535312, 1.000000000000000000, 0.9510565162951535312, 1.000000000000000000, 0.9510565162951535312, 1.000000000000000000, 0.9510565162951535312, 1.000000000000000000, 0.9510565162951535312, 1.000000000000000000, 0.9510565162951535312, 1.000000000000000000, 0.9510565162951535312, 1.000000000000000000, 0.9510565162951535312, 1.000000000000000000, 0.9510565162951535312, 1.000000000000000000, 0.9510565162951535312, 1.000000000000000000, 0.9510565162951535312, 1.000000000000000000, 0.9510565162951535312, 1.000000000000000000, 0.9510565162951535312, 1.000000000000000000, 0.9510565162951535312, 1.000000000000000000, 0.9510565162951535312, 1.000000000000000000, 0.9510565162951535312, 1.000000000000000000, 0.9510565162951535312, 1.000000000000000000, 0.9510565162951535312, 1.000000000000000000, 0.9510565162951535312, 1.000000000000000000, 0.9510565162951535312, 1.000000000000000000, 0.9510565162951535312, 1.000000000000000000, 0.9510565162951535312, 1.000000000000000000, 0.9510565162951535312, 1.000000000000000000, 0.9510565162951535312, 1.000000000000000000, 0.9510565162951535312, 1.000000000000000000, 0.9510565162951535312, 1.000000000000000000, 0.9510565162951535312, 1.000000000000000000, 0.9510565162951535312, 1.000000000000000000, 0.9510565162951535312, 1.000000000000000000, 0.9510565162951535312, 1.000000000000000000, 0.9510565162951535312, 1.000000000000000000, 0.9510565162951535312, 1.000000000000000000, 0.9510565162951535312, 1.000000000000000000, 0.9510565162951535312, 1.000000000000000000, 0.9510565162951535312, 1.000000000000000000, 0.9510565162951535312, 1.000000000000000000, 0.9510565162951535312, 1.000000000000000000, 0.9510565162951535312, 1.000000000000000000, 0.9510565162951535312, 1.000000000000000000, 0.9510565162951535312, 1.000000000000000000, 0.9510565162951535312, 1.000000000000000000, 0.9510565162951535312, 1.000000000000000000, 0.9510565162951535312, 1.000000000000000000, 0.9510565162951535312, 1.000000000000000000, 0.9510565162951535312, 1.000000000000000000, 0.9510565162951535312, 1.000000000000000000, 0.9510565162951535312, 1.000000000000000000, 0.9510565162951535312, 1.000000000000000000, 0.9510565162951535312, 1.000000000000000000) ) ) 
 REPRESENTATION_ITEM ( '' )  SURFACE ( )  );
#25776 = CARTESIAN_POINT ( 'NONE',  ( 51.42518405393695957, 36.98164062499999005, -5.622872871577872189 ) ) ;
#25777 = VECTOR ( 'NONE', #12816, 1000.000000000000000 ) ;
#25778 = CARTESIAN_POINT ( 'NONE',  ( 13.14518615778179900, 39.31328125108392868, 5.444914386472293977 ) ) ;
#25779 = CARTESIAN_POINT ( 'NONE',  ( 208.5748159460630120, 36.58476562499999574, 5.622872871577869525 ) ) ;
#25780 = CARTESIAN_POINT ( 'NONE',  ( 51.42518405393695957, 39.36289062499999858, -5.622872871577872189 ) ) ;
#25781 = CARTESIAN_POINT ( 'NONE',  ( 98.15313185440925281, 4.458734125000016313, 2.500000001365592084 ) ) ;
#25782 = CARTESIAN_POINT ( 'NONE',  ( 65.00000000000000000, 38.37070312608393152, 13.14518615778179544 ) ) ;
#25783 = CARTESIAN_POINT ( 'NONE',  ( 104.4587341249999781, 1.846868145590750521, 7.000000001365592972 ) ) ;
#25784 = DIRECTION ( 'NONE',  ( 0.000000000000000000, 0.000000000000000000, -1.000000000000000000 ) ) ;
#25785 = CARTESIAN_POINT ( 'NONE',  ( 96.84719886470463734, 94.68749999863440792, -3.152801135295366208 ) ) ;
#25786 = AXIS2_PLACEMENT_3D ( 'NONE', #3031, #1050, #7434 ) ;
#25787 = CARTESIAN_POINT ( 'NONE',  ( 116.4251840539369596, 39.41249999999999432, 0.000000000000000000 ) ) ;
#25788 = CARTESIAN_POINT ( 'NONE',  ( -13.57481594606304753, 40.15664062500000142, -5.622872871577873077 ) ) ;
#25789 = CARTESIAN_POINT ( 'NONE',  ( 139.2950502721270425, 39.46210937608393721, 9.295050272127046043 ) ) ;
#25790 = EDGE_LOOP ( 'NONE', ( #7035, #14924, #16208, #27960 ) ) ;
#25791 = CARTESIAN_POINT ( 'NONE',  ( 96.84719886470459471, 84.56250000136560629, -3.152801135295383084 ) ) ;
#25792 = CARTESIAN_POINT ( 'NONE',  ( 130.0000000000000000, 39.71015625216787015, 13.57481594606304576 ) ) ;
#25793 = ORIENTED_EDGE ( 'NONE', *, *, #10798, .T. ) ;
#25794 = CYLINDRICAL_SURFACE ( 'NONE', #12934, 5.000000000000000888 ) ;
#25795 = CARTESIAN_POINT ( 'NONE',  ( 78.14518615778179367, 34.74921875108395142, 5.444914386472293977 ) ) ;
#25796 = EDGE_LOOP ( 'NONE', ( #2825, #14984, #19190, #16685 ) ) ;
#25797 = VECTOR ( 'NONE', #21267, 999.9999999999997726 ) ;
#25798 = CARTESIAN_POINT ( 'NONE',  ( 133.8654143754132235, 54.10683252460147941, -15.00000000000000000 ) ) ;
#25799 = CARTESIAN_POINT ( 'NONE',  ( 98.15313185440925281, 4.458734125000016313, 2.500000001365592084 ) ) ;
#25800 = ORIENTED_EDGE ( 'NONE', *, *, #22015, .T. ) ;
#25801 = CARTESIAN_POINT ( 'NONE',  ( 9.295050272127047819, 34.69960937608393436, 9.295050272127046043 ) ) ;
#25802 = CARTESIAN_POINT ( 'NONE',  ( 5.444914386472302859, 40.20625000108394431, 13.14518615778179189 ) ) ;
#25803 = CARTESIAN_POINT ( 'NONE',  ( 181.4251840539369596, 37.97382812716787726, 5.622872871577880183 ) ) ;
#25804 = CARTESIAN_POINT ( 'NONE',  ( -13.14518615778179189, 35.84062500108394289, 5.444914386472304635 ) ) ;
#25805 = DIRECTION ( 'NONE',  ( -1.000000000000000000, 0.000000000000000000, 0.000000000000000000 ) ) ;
#25806 = DIRECTION ( 'NONE',  ( -0.000000000000000000, 1.000000000000000000, -0.000000000000000000 ) ) ;
#25807 = PRODUCT_RELATED_PRODUCT_CATEGORY ( 'part', '', ( #26282 ) ) ;
#25808 = CARTESIAN_POINT ( 'NONE',  ( 139.2950502721270425, 40.25585937608393294, 9.295050272127046043 ) ) ;
#25809 = CARTESIAN_POINT ( 'NONE',  ( 13.14518615778179900, 37.13046875108393863, 5.444914386472293977 ) ) ;
#25810 = ADVANCED_FACE ( 'NONE', ( #19407 ), #8381, .F. ) ;
#25811 = ORIENTED_EDGE ( 'NONE', *, *, #21552, .F. ) ;
#25812 = CARTESIAN_POINT ( 'NONE',  ( 139.2950502721270425, 36.28710937608393294, -9.295050272127046043 ) ) ;
#25813 = CARTESIAN_POINT ( 'NONE',  ( 55.40115559117954547, 37.13046874999999147, 9.598844408820459861 ) ) ;
#25814 = CARTESIAN_POINT ( 'NONE',  ( 94.99999999999995737, 1.387778780781445676E-14, 9.999999999999998224 ) ) ;
#25815 = CARTESIAN_POINT ( 'NONE',  ( 95.54126587499996504, 1.387778780781445676E-14, 14.68750000136559208 ) ) ;
#25816 = CARTESIAN_POINT ( 'NONE',  ( 104.3262379212492590, 115.9545556584642867, -46.69999999999999574 ) ) ;
#25817 = CARTESIAN_POINT ( 'NONE',  ( 96.84719886470459471, -3.152801135295355994, 5.562500001365591196 ) ) ;
#25818 = CARTESIAN_POINT ( 'NONE',  ( 104.9952793366501851, 103.1245878333314323, -52.42500000273119554 ) ) ;
#25819 = CYLINDRICAL_SURFACE ( 'NONE', #21364, 5.000000000000004441 ) ;
#25820 = AXIS2_PLACEMENT_3D ( 'NONE', #22204, #11344, #19634 ) ;
#25821 = CARTESIAN_POINT ( 'NONE',  ( 112.9999999999999858, 100.0000000000000000, -13.00000000000000711 ) ) ;
#25822 = CARTESIAN_POINT ( 'NONE',  ( -13.14518615778179189, 33.45937500108392726, 5.444914386472304635 ) ) ;
#25823 = CARTESIAN_POINT ( 'NONE',  ( -8.049105076161786076E-16, 38.17226562608394147, -13.14518615778179544 ) ) ;
#25824 = CARTESIAN_POINT ( 'NONE',  ( 95.00472066334982912, 116.8754121666685393, -48.17499999726882010 ) ) ;
#25825 = ORIENTED_EDGE ( 'NONE', *, *, #17318, .F. ) ;
#25826 = CARTESIAN_POINT ( 'NONE',  ( 5.444914386472297529, 32.56640625108394005, -13.14518615778179722 ) ) ;
#25827 = CYLINDRICAL_SURFACE ( 'NONE', #2539, 5.000000000000000888 ) ;
#25828 = CARTESIAN_POINT ( 'NONE',  ( 99.99999999999995737, 5.000000000000018652, 5.750000000000000000 ) ) ;
#25829 = CARTESIAN_POINT ( 'NONE',  ( -9.180175813647995398, 55.00000000000000000, 15.00000000000000000 ) ) ;
#25830 = CARTESIAN_POINT ( 'NONE',  ( 65.00000000000000000, 36.43593749999999432, 13.57481594606304576 ) ) ;
#25831 =( BOUNDED_SURFACE ( )  B_SPLINE_SURFACE ( 1, 2, ( 
 ( #25650, #1455, #25791, #22977, #21106, #18958, #12244, #14396, #6134, #21391, #25385, #4001, #1594, #14664, #7854, #1312, #1868, #27666, #14799, #23113, #12666, #20972, #16686, #27395, #23523, #3588, #10534, #8128, #16825, #8263, #23385, #19240, #3442, #21247, #19098, #9982, #27940, #27807, #20835, #5999, #16949, #25521, #14257, #3857, #12517, #18692, #16549, #8399, #23249, #17088, #14536, #1728, #10110, #12109, #7987, #18824, #27531, #3726, #10392, #4701, #15220, #23797, #4420, #8826, #6410, #19799, #9110, #13073, #4275, #17804, #26218, #6268, #13362, #12933, #10806, #14943, #8969, #19658, #17515, #21666, #23663 ),
 ( #2143, #19520, #4138, #17657, #140, #6678, #26072, #2288, #2567, #6822, #26364, #15364, #12801, #21522, #22089, #24078, #15079, #2, #4556, #13217, #19376, #8686, #2001, #283, #15513, #23938, #21811, #17376, #10668, #17232, #25935, #6541, #24222, #11229, #10946, #28080, #19946, #424, #8544, #21950, #2428, #11089, #2979, #18233, #17944, #7386, #1147, #9534, #2843, #24652, #24358, #16079, #26508, #570, #5125, #9673, #13655, #9814, #6964, #13792, #11654, #24504, #26654, #18376, #5415, #9388, #16230, #22514, #26942, #20092, #13511, #14083, #20377, #27081, #7102, #24929, #4990, #712, #11370, #7533, #9252 ) ),
 .UNSPECIFIED., .F., .F., .F. ) 
 B_SPLINE_SURFACE_WITH_KNOTS ( ( 2, 2 ),
 ( 3, 2, 2, 2, 2, 2, 2, 2, 2, 2, 2, 2, 2, 2, 2, 2, 2, 2, 2, 2, 2, 2, 2, 2, 2, 2, 2, 2, 2, 2, 2, 2, 2, 2, 2, 2, 2, 2, 2, 2, 3 ),
 ( 0.000000000000000000, 1.000000000000000000 ),
 ( 0.000000000000000000, 0.02500000000000000139, 0.05000000000000000278, 0.07499999999999999722, 0.1000000000000000056, 0.1250000000000000000, 0.1499999999999999944, 0.1749999999999999889, 0.2000000000000000111, 0.2250000000000000056, 0.2500000000000000000, 0.2750000000000000222, 0.2999999999999999889, 0.3250000000000000111, 0.3499999999999999778, 0.3750000000000000000, 0.4000000000000000222, 0.4249999999999999889, 0.4500000000000000111, 0.4749999999999999778, 0.5000000000000000000, 0.5250000000000000222, 0.5500000000000000444, 0.5749999999999999556, 0.5999999999999999778, 0.6250000000000000000, 0.6500000000000000222, 0.6750000000000000444, 0.6999999999999999556, 0.7249999999999999778, 0.7500000000000000000, 0.7750000000000000222, 0.8000000000000000444, 0.8249999999999999556, 0.8499999999999999778, 0.8750000000000000000, 0.9000000000000000222, 0.9250000000000000444, 0.9499999999999999556, 0.9749999999999999778, 1.000000000000000000 ),
 .UNSPECIFIED. ) 
 GEOMETRIC_REPRESENTATION_ITEM ( )  RATIONAL_B_SPLINE_SURFACE ( (
 ( 1.000000000000000000, 0.9238795325112867385, 1.000000000000000000, 0.9238795325112867385, 1.000000000000000000, 0.9238795325112867385, 1.000000000000000000, 0.9238795325112867385, 1.000000000000000000, 0.9238795325112867385, 1.000000000000000000, 0.9238795325112867385, 1.000000000000000000, 0.9238795325112867385, 1.000000000000000000, 0.9238795325112867385, 1.000000000000000000, 0.9238795325112867385, 1.000000000000000000, 0.9238795325112867385, 1.000000000000000000, 0.9238795325112867385, 1.000000000000000000, 0.9238795325112867385, 1.000000000000000000, 0.9238795325112867385, 1.000000000000000000, 0.9238795325112867385, 1.000000000000000000, 0.9238795325112867385, 1.000000000000000000, 0.9238795325112867385, 1.000000000000000000, 0.9238795325112867385, 1.000000000000000000, 0.9238795325112867385, 1.000000000000000000, 0.9238795325112867385, 1.000000000000000000, 0.9238795325112867385, 1.000000000000000000, 0.9238795325112867385, 1.000000000000000000, 0.9238795325112867385, 1.000000000000000000, 0.9238795325112867385, 1.000000000000000000, 0.9238795325112867385, 1.000000000000000000, 0.9238795325112867385, 1.000000000000000000, 0.9238795325112867385, 1.000000000000000000, 0.9238795325112867385, 1.000000000000000000, 0.9238795325112867385, 1.000000000000000000, 0.9238795325112867385, 1.000000000000000000, 0.9238795325112867385, 1.000000000000000000, 0.9238795325112867385, 1.000000000000000000, 0.9238795325112867385, 1.000000000000000000, 0.9238795325112867385, 1.000000000000000000, 0.9238795325112867385, 1.000000000000000000, 0.9238795325112867385, 1.000000000000000000, 0.9238795325112867385, 1.000000000000000000, 0.9238795325112867385, 1.000000000000000000, 0.9238795325112867385, 1.000000000000000000, 0.9238795325112867385, 1.000000000000000000, 0.9238795325112867385, 1.000000000000000000),
 ( 1.000000000000000000, 0.9238795325112867385, 1.000000000000000000, 0.9238795325112867385, 1.000000000000000000, 0.9238795325112867385, 1.000000000000000000, 0.9238795325112867385, 1.000000000000000000, 0.9238795325112867385, 1.000000000000000000, 0.9238795325112867385, 1.000000000000000000, 0.9238795325112867385, 1.000000000000000000, 0.9238795325112867385, 1.000000000000000000, 0.9238795325112867385, 1.000000000000000000, 0.9238795325112867385, 1.000000000000000000, 0.9238795325112867385, 1.000000000000000000, 0.9238795325112867385, 1.000000000000000000, 0.9238795325112867385, 1.000000000000000000, 0.9238795325112867385, 1.000000000000000000, 0.9238795325112867385, 1.000000000000000000, 0.9238795325112867385, 1.000000000000000000, 0.9238795325112867385, 1.000000000000000000, 0.9238795325112867385, 1.000000000000000000, 0.9238795325112867385, 1.000000000000000000, 0.9238795325112867385, 1.000000000000000000, 0.9238795325112867385, 1.000000000000000000, 0.9238795325112867385, 1.000000000000000000, 0.9238795325112867385, 1.000000000000000000, 0.9238795325112867385, 1.000000000000000000, 0.9238795325112867385, 1.000000000000000000, 0.9238795325112867385, 1.000000000000000000, 0.9238795325112867385, 1.000000000000000000, 0.9238795325112867385, 1.000000000000000000, 0.9238795325112867385, 1.000000000000000000, 0.9238795325112867385, 1.000000000000000000, 0.9238795325112867385, 1.000000000000000000, 0.9238795325112867385, 1.000000000000000000, 0.9238795325112867385, 1.000000000000000000, 0.9238795325112867385, 1.000000000000000000, 0.9238795325112867385, 1.000000000000000000, 0.9238795325112867385, 1.000000000000000000, 0.9238795325112867385, 1.000000000000000000, 0.9238795325112867385, 1.000000000000000000, 0.9238795325112867385, 1.000000000000000000, 0.9238795325112867385, 1.000000000000000000) ) ) 
 REPRESENTATION_ITEM ( '' )  SURFACE ( )  );
#25832 = CARTESIAN_POINT ( 'NONE',  ( 208.1451861577818079, 40.15664062608393436, -1.609821015232357215E-15 ) ) ;
#25833 = ORIENTED_EDGE ( 'NONE', *, *, #21171, .F. ) ;
#25834 = DIRECTION ( 'NONE',  ( 0.000000000000000000, 0.000000000000000000, 1.000000000000000000 ) ) ;
#25835 = CARTESIAN_POINT ( 'NONE',  ( 107.0000000000000000, 110.0000000000000000, -54.00000000000001421 ) ) ;
#25836 = CARTESIAN_POINT ( 'NONE',  ( 61.96060294919745814, 53.88964894337311051, -14.99999999999999822 ) ) ;
#25837 = ORIENTED_EDGE ( 'NONE', *, *, #24542, .F. ) ;
#25838 = CARTESIAN_POINT ( 'NONE',  ( 104.3262379212492590, 104.0454443415356991, -49.30000000000000426 ) ) ;
#25839 = CARTESIAN_POINT ( 'NONE',  ( -2.276146844545014591, 51.46995505939283788, -14.99999999999999822 ) ) ;
#25840 = CARTESIAN_POINT ( 'NONE',  ( 104.9999999999999858, 92.87499999726881583, -6.938893903907228378E-15 ) ) ;
#25841 = CARTESIAN_POINT ( 'NONE',  ( 120.4011555911795455, 33.85625000216787583, -9.598844408820458085 ) ) ;
#25842 = CARTESIAN_POINT ( 'NONE',  ( 70.44491438647230552, 40.50390625108394005, -13.14518615778179900 ) ) ;
#25843 = EDGE_CURVE ( 'NONE', #3824, #3142, #25163, .T. ) ;
#25844 = CARTESIAN_POINT ( 'NONE',  ( 9.598844408820459861, 37.32890624999999574, 9.598844408820456309 ) ) ;
#25845 = CARTESIAN_POINT ( 'NONE',  ( 208.1451861577817795, 33.26093750108393721, -5.444914386472297529 ) ) ;
#25846 = ORIENTED_EDGE ( 'NONE', *, *, #6873, .F. ) ;
#25847 = EDGE_CURVE ( 'NONE', #17997, #20267, #10369, .T. ) ;
#25848 = VERTEX_POINT ( 'NONE', #2669 ) ;
#25849 = ORIENTED_EDGE ( 'NONE', *, *, #1836, .T. ) ;
#25850 = CARTESIAN_POINT ( 'NONE',  ( 13.14518615778179900, 39.61093750108393863, -5.444914386472297529 ) ) ;
#25851 = SHAPE_REPRESENTATION_RELATIONSHIP ( 'NONE' , 'NONE' ,  #14947, #4607 ) ;
#25852 = EDGE_CURVE ( 'NONE', #23414, #1457, #5492, .T. ) ;
#25853 = DIRECTION ( 'NONE',  ( 0.000000000000000000, 0.000000000000000000, -1.000000000000000000 ) ) ;
#25854 = CARTESIAN_POINT ( 'NONE',  ( 51.85481384221820633, 40.55351562608393579, 0.000000000000000000 ) ) ;
#25855 = CARTESIAN_POINT ( 'NONE',  ( 95.54126587499996504, 82.37500000136563472, -1.846868145590750077 ) ) ;
#25856 = CARTESIAN_POINT ( 'NONE',  ( 200.4449143864723055, 37.62656250108393152, 13.14518615778179189 ) ) ;
#25857 = CARTESIAN_POINT ( 'NONE',  ( 139.5988444088204687, 39.80937500216786873, 9.598844408820456309 ) ) ;
#25858 = CARTESIAN_POINT ( 'NONE',  ( 181.4251840539369596, 40.65273437608393436, 0.000000000000000000 ) ) ;
#25859 = CARTESIAN_POINT ( 'NONE',  ( 94.99999999999995737, 1.387778780781445676E-14, 34.79898987322334136 ) ) ;
#25860 = CARTESIAN_POINT ( 'NONE',  ( 107.0000000000000142, 110.0000000000000000, -55.00000000000000711 ) ) ;
#25861 = CARTESIAN_POINT ( 'NONE',  ( 102.4976396683250783, 117.6869444889999841, -48.22499999726881725 ) ) ;
#25862 = VECTOR ( 'NONE', #24751, 1000.000000000000000 ) ;
#25863 = EDGE_CURVE ( 'NONE', #21015, #12194, #3657, .T. ) ;
#25864 = ORIENTED_EDGE ( 'NONE', *, *, #21145, .F. ) ;
#25865 = CARTESIAN_POINT ( 'NONE',  ( 9.598844408820459861, 38.12265624999999858, 9.598844408820456309 ) ) ;
#25866 = CARTESIAN_POINT ( 'NONE',  ( 13.14518615778179544, 36.98164062608393010, -1.609821015232357215E-15 ) ) ;
#25867 = AXIS2_PLACEMENT_3D ( 'NONE', #344, #7269, #15959 ) ;
#25868 =( BOUNDED_CURVE ( )  B_SPLINE_CURVE ( 2, ( #1918, #6183, #3773, #28129, #21438 ),
 .UNSPECIFIED., .F., .T. ) 
 B_SPLINE_CURVE_WITH_KNOTS ( ( 3, 2, 3 ),
 ( 0.000000000000000000, 0.01041666666666679446, 0.02083333333333358892 ),
 .UNSPECIFIED. ) 
 CURVE ( )  GEOMETRIC_REPRESENTATION_ITEM ( )  RATIONAL_B_SPLINE_CURVE ( ( 1.000000000000000000, 0.9238795325112867385, 1.000000000000000000, 0.9238795325112848511, 1.000000000000001776 ) ) 
 REPRESENTATION_ITEM ( '' )  );
#25869 = CARTESIAN_POINT ( 'NONE',  ( 104.9999999999999716, 1.449011120738813565E-14, 0.6250000027311856110 ) ) ;
#25870 = CARTESIAN_POINT ( 'NONE',  ( 124.5550856135277087, 35.34453125108393579, 13.14518615778179722 ) ) ;
#25871 = CARTESIAN_POINT ( 'NONE',  ( 74.29505027212704249, 34.50117187608393010, 9.295050272127046043 ) ) ;
#25872 = CARTESIAN_POINT ( 'NONE',  ( 208.1451861577818079, 37.18007812608393436, -1.609821015232357215E-15 ) ) ;
#25873 = PLANE ( 'NONE',  #24813 ) ;
#25874 =( BOUNDED_CURVE ( )  B_SPLINE_CURVE ( 2, ( #3291, #18809, #12501, #14380, #11961, #9832, #18539, #27243, #5847 ),
 .UNSPECIFIED., .F., .F. ) 
 B_SPLINE_CURVE_WITH_KNOTS ( ( 3, 2, 2, 2, 3 ),
 ( 0.1428571428571428492, 0.1517857142857142738, 0.1607142857142857539, 0.1696428571428571785, 0.1785714285714286031 ),
 .UNSPECIFIED. ) 
 CURVE ( )  GEOMETRIC_REPRESENTATION_ITEM ( )  RATIONAL_B_SPLINE_CURVE ( ( 1.000000000000000000, 0.9238795325112867385, 1.000000000000000000, 0.9238795325112867385, 1.000000000000000000, 0.9238795325112867385, 1.000000000000000000, 0.9238795325112865164, 1.000000000000000222 ) ) 
 REPRESENTATION_ITEM ( '' )  );
#25875 = CARTESIAN_POINT ( 'NONE',  ( 5.444914386472302859, 34.45156250108393436, 13.14518615778179189 ) ) ;
#25876 = CARTESIAN_POINT ( 'NONE',  ( 134.9250267836615080, 49.99999999893073266, -12.67776588291936690 ) ) ;
#25877 = CARTESIAN_POINT ( 'NONE',  ( 187.2214956318787245, 35.99999999999997868, 10.60546543669477515 ) ) ;
#25878 = EDGE_CURVE ( 'NONE', #3914, #18296, #26470, .T. ) ;
#25879 = CARTESIAN_POINT ( 'NONE',  ( 99.99999999999998579, 138.0000000000000000, -11.50000000000002309 ) ) ;
#25880 = CARTESIAN_POINT ( 'NONE',  ( -13.14518615778179189, 39.01562500108393294, 5.444914386472304635 ) ) ;
#25881 = PLANE ( 'NONE',  #14270 ) ;
#25882 = CARTESIAN_POINT ( 'NONE',  ( 98.96446609406727646, 122.5500000021849587, -2.499999999999997780 ) ) ;
#25883 = VECTOR ( 'NONE', #26175, 1000.000000000000000 ) ;
#25884 = CARTESIAN_POINT ( 'NONE',  ( 63.86123188289986530, 50.00000000043846882, 13.56816686242530601 ) ) ;
#25885 = ORIENTED_EDGE ( 'NONE', *, *, #5672, .T. ) ;
#25886 = CARTESIAN_POINT ( 'NONE',  ( 104.4587341249999781, 1.846868145590750299, 7.000000001365591196 ) ) ;
#25887 = CARTESIAN_POINT ( 'NONE',  ( 78.04200858115000017, 36.00000000000000000, -3.640726557253424200 ) ) ;
#25888 = ORIENTED_EDGE ( 'NONE', *, *, #21004, .F. ) ;
#25889 = CARTESIAN_POINT ( 'NONE',  ( 120.4011555911795455, 40.90078124999999432, -9.598844408820458085 ) ) ;
#25890 = CARTESIAN_POINT ( 'NONE',  ( 95.54126587499995082, 1.846868145590750077, 10.37500000136559208 ) ) ;
#25891 = DIRECTION ( 'NONE',  ( 0.000000000000000000, 0.000000000000000000, 1.000000000000000000 ) ) ;
#25892 = EDGE_CURVE ( 'NONE', #4566, #26480, #19621, .T. ) ;
#25893 = CARTESIAN_POINT ( 'NONE',  ( -13.14518615778179900, 39.71015625108393010, -5.444914386472297529 ) ) ;
#25894 = DIRECTION ( 'NONE',  ( 0.000000000000000000, -0.000000000000000000, -1.000000000000000000 ) ) ;
#25895 = CARTESIAN_POINT ( 'NONE',  ( 104.4587341249999781, 82.12500000136560629, 1.846868145590721655 ) ) ;
#25896 = CARTESIAN_POINT ( 'NONE',  ( 78.14518615778179367, 37.22968750108393721, -5.444914386472297529 ) ) ;
#25897 = CARTESIAN_POINT ( 'NONE',  ( 93.46109445667491400, 105.2492070361643215, -52.92500000273119554 ) ) ;
#25898 = CARTESIAN_POINT ( 'NONE',  ( -9.295050272127046043, 39.66054687608393436, -9.295050272127046043 ) ) ;
#25899 = CARTESIAN_POINT ( 'NONE',  ( 195.0000000000000000, 36.00000000000000000, -2.255140518769849538E-14 ) ) ;
#25900 = CARTESIAN_POINT ( 'NONE',  ( -18.00000000000000355, 52.00000000000000711, 13.00000000000000178 ) ) ;
#25901 = CARTESIAN_POINT ( 'NONE',  ( 99.99999999999997158, 117.3602355696678501, -50.99999999453762456 ) ) ;
#25902 = CARTESIAN_POINT ( 'NONE',  ( 135.6228728715778971, 40.45429687500001137, 13.57481594606304576 ) ) ;
#25903 = EDGE_LOOP ( 'NONE', ( #27674, #9398, #9183, #8497 ) ) ;
#25904 = CARTESIAN_POINT ( 'NONE',  ( 97.83688103937537051, 103.3426043859339103, -56.09999999453764730 ) ) ;
#25905 = DIRECTION ( 'NONE',  ( 0.000000000000000000, 0.000000000000000000, 1.000000000000000000 ) ) ;
#25906 = CARTESIAN_POINT ( 'NONE',  ( 99.99999999999995737, 80.18750000136559208, -4.458734125000016313 ) ) ;
#25907 = CARTESIAN_POINT ( 'NONE',  ( 120.7049497278729575, 35.89023437608393152, 9.295050272127047819 ) ) ;
#25908 = CARTESIAN_POINT ( 'NONE',  ( 55.40115559117954547, 36.23750000216787726, -9.598844408820458085 ) ) ;
#25909 = CARTESIAN_POINT ( 'NONE',  ( 102.0710678118654187, 83.31249999999998579, 5.000000000000011546 ) ) ;
#25910 = CARTESIAN_POINT ( 'NONE',  ( -8.312177448680279460E-16, 36.93203125216787441, -13.57481594606304576 ) ) ;
#25911 = AXIS2_PLACEMENT_3D ( 'NONE', #4062, #18876, #3782 ) ;
#25912 = CARTESIAN_POINT ( 'NONE',  ( 104.9999999999999716, 1.449011120738813565E-14, 6.499999999999999112 ) ) ;
#25913 = CARTESIAN_POINT ( 'NONE',  ( 104.9999999999999716, 1.449011120738813565E-14, 1.499999999999999556 ) ) ;
#25914 =( BOUNDED_CURVE ( )  B_SPLINE_CURVE ( 2, ( #21568, #27706, #21711, #25692, #10290, #8170, #8445, #14986, #8303 ),
 .UNSPECIFIED., .F., .F. ) 
 B_SPLINE_CURVE_WITH_KNOTS ( ( 3, 2, 2, 2, 3 ),
 ( 0.1500000000000001332, 0.1750000000000001554, 0.2000000000000001776, 0.2250000000000001998, 0.2500000000000002220 ),
 .UNSPECIFIED. ) 
 CURVE ( )  GEOMETRIC_REPRESENTATION_ITEM ( )  RATIONAL_B_SPLINE_CURVE ( ( 0.9999999999999995559, 0.9238795325112871826, 1.000000000000000000, 0.9238795325112867385, 1.000000000000000000, 0.9238795325112867385, 1.000000000000000000, 0.9238795325112860723, 1.000000000000000666 ) ) 
 REPRESENTATION_ITEM ( '' )  );
#25915 = CARTESIAN_POINT ( 'NONE',  ( 208.1451861577818079, 38.56914062608393579, -1.609821015232357215E-15 ) ) ;
#25916 = CARTESIAN_POINT ( 'NONE',  ( -13.57481594606304398, 38.66835937499999432, 5.622872871577880183 ) ) ;
#25917 = CARTESIAN_POINT ( 'NONE',  ( 120.7049497278729575, 36.48554687608393721, -9.295050272127046043 ) ) ;
#25918 = CARTESIAN_POINT ( 'NONE',  ( 2.493653234604083739E-15, 35.64218749999999147, 13.57481594606304576 ) ) ;
#25919 = CARTESIAN_POINT ( 'NONE',  ( 214.9999999999999716, 80.00000000000000000, -15.00000000000000000 ) ) ;
#25920 = CARTESIAN_POINT ( 'NONE',  ( 130.3247243111959790, 53.49346745874645137, 14.99999999999996447 ) ) ;
#25921 = CARTESIAN_POINT ( 'NONE',  ( 94.99999999999995737, 1.387778780781445676E-14, 0.5625000013655921949 ) ) ;
#25922 = CARTESIAN_POINT ( 'NONE',  ( 2.414731522848535132E-15, 37.77539062608393294, 13.14518615778179544 ) ) ;
#25923 = CARTESIAN_POINT ( 'NONE',  ( -13.14518615778179189, 39.80937500108392868, 5.444914386472304635 ) ) ;
#25924 = CARTESIAN_POINT ( 'NONE',  ( 208.5748159460630688, 39.01562500000000000, -1.662435489736055892E-15 ) ) ;
#25925 = LINE ( 'NONE', #17220, #11276 ) ;
#25926 = CARTESIAN_POINT ( 'NONE',  ( 96.84719886470459471, 3.152801135295383084, 3.562500001365592972 ) ) ;
#25927 = CARTESIAN_POINT ( 'NONE',  ( 78.14518615778179367, 37.77539062608393294, -1.609821015232357215E-15 ) ) ;
#25928 = CARTESIAN_POINT ( 'NONE',  ( 104.4587341249999781, -1.846868145590721655, 0.8750000013655925279 ) ) ;
#25929 = CYLINDRICAL_SURFACE ( 'NONE', #25954, 7.000000000000006217 ) ;
#25930 = CARTESIAN_POINT ( 'NONE',  ( 101.8468681455907330, 92.12499999863437949, 4.458734124999979898 ) ) ;
#25931 = CARTESIAN_POINT ( 'NONE',  ( 97.94614682514237813, 122.9999999999999858, -0.2688731231943997102 ) ) ;
#25932 = CARTESIAN_POINT ( 'NONE',  ( 9.598844408820456309, 35.14609374999999858, -9.598844408820458085 ) ) ;
#25933 = CARTESIAN_POINT ( 'NONE',  ( 107.0000000000000142, 107.7255621263696526, -45.10000000000000853 ) ) ;
#25934 = ORIENTED_EDGE ( 'NONE', *, *, #18560, .F. ) ;
#25935 = CARTESIAN_POINT ( 'NONE',  ( 96.46446609406721961, 83.12500000000000000, 3.535533905932727539 ) ) ;
#25936 = CARTESIAN_POINT ( 'NONE',  ( 96.84719886470463734, 92.68749999863440792, -3.152801135295366208 ) ) ;
#25937 = ORIENTED_EDGE ( 'NONE', *, *, #11586, .F. ) ;
#25938 = AXIS2_PLACEMENT_3D ( 'NONE', #3477, #20867, #1351 ) ;
#25939 = CARTESIAN_POINT ( 'NONE',  ( 208.5748159460630688, 37.52734375216787299, -1.662435489736055892E-15 ) ) ;
#25940 = CARTESIAN_POINT ( 'NONE',  ( 78.14518615778179367, 34.00507812608393721, -1.609821015232357215E-15 ) ) ;
#25941 = EDGE_LOOP ( 'NONE', ( #13830, #23253, #26759, #11301 ) ) ;
#25942 = CARTESIAN_POINT ( 'NONE',  ( 94.99999999999995737, 1.387778780781445676E-14, 34.79898987322334136 ) ) ;
#25943 = CARTESIAN_POINT ( 'NONE',  ( 99.99999999999995737, 4.458734125000016313, 4.437500001365592084 ) ) ;
#25944 = VERTEX_POINT ( 'NONE', #104 ) ;
#25945 = CARTESIAN_POINT ( 'NONE',  ( 219.9999999999999716, 55.00000000000000000, 14.99999999999994316 ) ) ;
#25946 = CARTESIAN_POINT ( 'NONE',  ( 3.755639919285892248, 31.58960996655074993, -13.14518615778179544 ) ) ;
#25947 = CARTESIAN_POINT ( 'NONE',  ( 208.5748159460630688, 36.73359375216787015, -1.662435489736055892E-15 ) ) ;
#25948 =( BOUNDED_CURVE ( )  B_SPLINE_CURVE ( 2, ( #7212, #13904, #11483, #7356, #22632, #2815, #11767, #5524, #20491 ),
 .UNSPECIFIED., .F., .T. ) 
 B_SPLINE_CURVE_WITH_KNOTS ( ( 3, 2, 2, 2, 3 ),
 ( 0.8500000000000007550, 0.8750000000000008882, 0.9000000000000009104, 0.9250000000000009326, 0.9500000000000009548 ),
 .UNSPECIFIED. ) 
 CURVE ( )  GEOMETRIC_REPRESENTATION_ITEM ( )  RATIONAL_B_SPLINE_CURVE ( ( 0.9999999999999976685, 0.9238795325112890700, 1.000000000000000000, 0.9238795325112867385, 1.000000000000000000, 0.9238795325112867385, 1.000000000000000000, 0.9238795325112837409, 1.000000000000003109 ) ) 
 REPRESENTATION_ITEM ( '' )  );
#25949 = CARTESIAN_POINT ( 'NONE',  ( -5.444914386472297529, 36.43593750108394147, -13.14518615778179722 ) ) ;
#25950 = CARTESIAN_POINT ( 'NONE',  ( -20.00000000000000355, 55.00000000000000000, -10.00000000000000000 ) ) ;
#25951 = CARTESIAN_POINT ( 'NONE',  ( 107.0000000000000142, 110.0000000000000000, -51.00000000000000711 ) ) ;
#25952 = CARTESIAN_POINT ( 'NONE',  ( 120.7049497278729575, 39.85898437608393152, -9.295050272127046043 ) ) ;
#25954 = AXIS2_PLACEMENT_3D ( 'NONE', #27934, #2135, #6404 ) ;
#25953 = CARTESIAN_POINT ( 'NONE',  ( -5.444914386472297529, 39.01562500108394005, -13.14518615778179900 ) ) ;
#25955 = CARTESIAN_POINT ( 'NONE',  ( 120.7049497278729575, 33.50898437608393010, 9.295050272127047819 ) ) ;
#25956 = CARTESIAN_POINT ( 'NONE',  ( 59.37712712842213136, 35.59257812499999574, 13.57481594606304753 ) ) ;
#25957 = DIRECTION ( 'NONE',  ( 0.000000000000000000, 0.000000000000000000, 1.000000000000000000 ) ) ;
#25958 = CARTESIAN_POINT ( 'NONE',  ( 104.4587341249999781, -1.846868145590721655, 14.12500000136559208 ) ) ;
#25959 = CARTESIAN_POINT ( 'NONE',  ( 196.6855116490827697, 35.99999999999997868, 13.05727741351676130 ) ) ;
#25960 = AXIS2_PLACEMENT_3D ( 'NONE', #21757, #19604, #23884 ) ;
#25961 = CARTESIAN_POINT ( 'NONE',  ( 99.99999999999995737, 4.458734125000016313, 3.187500001365592972 ) ) ;
#25962 = CARTESIAN_POINT ( 'NONE',  ( 91.91746824999998466, 112.6261737610028320, -51.22500000273119980 ) ) ;
#25963 = CARTESIAN_POINT ( 'NONE',  ( 94.99999999999995737, 1.387778780781445676E-14, 1.125000002731184390 ) ) ;
#25964 = DIRECTION ( 'NONE',  ( 0.000000000000000000, 0.000000000000000000, 1.000000000000000000 ) ) ;
#25965 = CARTESIAN_POINT ( 'NONE',  ( -5.444914386472297529, 34.05468750108393294, -13.14518615778179900 ) ) ;
#25966 = CARTESIAN_POINT ( 'NONE',  ( 97.92893218813451028, 5.000000000000018652, 7.937500002731185056 ) ) ;
#25967 = CARTESIAN_POINT ( 'NONE',  ( 102.4976396683250783, 102.3130555110000159, -51.27499999726882152 ) ) ;
#25968 = VERTEX_POINT ( 'NONE', #26615 ) ;
#25969 = CARTESIAN_POINT ( 'NONE',  ( 99.99999999999998579, 123.7500000010924737, -2.066987299999998751 ) ) ;
#25970 = CARTESIAN_POINT ( 'NONE',  ( 97.93301270000000613, 123.0000000010925021, 0.8561741729129328515 ) ) ;
#25971 = FACE_OUTER_BOUND ( 'NONE', #7532, .T. ) ;
#25972 = LINE ( 'NONE', #23835, #16588 ) ;
#25973 = EDGE_CURVE ( 'NONE', #26178, #4636, #4563, .T. ) ;
#25974 = CARTESIAN_POINT ( 'NONE',  ( 208.1451861577817795, 37.72578125108393721, 5.444914386472293977 ) ) ;
#25975 = VERTEX_POINT ( 'NONE', #15894 ) ;
#25976 = CYLINDRICAL_SURFACE ( 'NONE', #14684, 7.000000000000006217 ) ;
#25977 = CARTESIAN_POINT ( 'NONE',  ( 99.99999999999998579, 110.0000000000000000, -145.0000000000000284 ) ) ;
#25978 = CARTESIAN_POINT ( 'NONE',  ( 98.15313185440925281, 4.458734125000016313, 14.50000000136559208 ) ) ;
#25979 = ORIENTED_EDGE ( 'NONE', *, *, #12250, .F. ) ;
#25980 = CARTESIAN_POINT ( 'NONE',  ( 104.3262379212492590, 115.9545556584642867, -50.70000000000000284 ) ) ;
#25981 = AXIS2_PLACEMENT_3D ( 'NONE', #16812, #5989, #23374 ) ;
#25982 = CARTESIAN_POINT ( 'NONE',  ( -5.444914386472297529, 38.81718750108393579, -13.14518615778179900 ) ) ;
#25983 = CARTESIAN_POINT ( 'NONE',  ( 97.93301270000000613, 123.1500000010924651, -9.540979117872439019E-15 ) ) ;
#25984 = CARTESIAN_POINT ( 'NONE',  ( 130.0000000000000000, 39.56132812608393579, -13.14518615778179544 ) ) ;
#25985 = DIRECTION ( 'NONE',  ( 0.000000000000000000, 0.000000000000000000, 1.000000000000000000 ) ) ;
#25986 = CARTESIAN_POINT ( 'NONE',  ( 104.9999999999999716, 81.68750000273119838, -2.071067811865491937 ) ) ;
#25987 = DIRECTION ( 'NONE',  ( -0.000000000000000000, -1.000000000000000000, -0.000000000000000000 ) ) ;
#25988 = AXIS2_PLACEMENT_3D ( 'NONE', #23703, #14842, #23840 ) ;
#25989 = CARTESIAN_POINT ( 'NONE',  ( 189.5550856135277229, 34.25312500108393010, -13.14518615778179900 ) ) ;
#25990 = ORIENTED_EDGE ( 'NONE', *, *, #27781, .T. ) ;
#25991 = ORIENTED_EDGE ( 'NONE', *, *, #12644, .F. ) ;
#25992 = CARTESIAN_POINT ( 'NONE',  ( -5.444914386472299306, 40.10703125108393152, 13.14518615778179722 ) ) ;
#25993 = CARTESIAN_POINT ( 'NONE',  ( 99.99999999999995737, -4.458734124999988779, 9.937500001365593860 ) ) ;
#25994 = CARTESIAN_POINT ( 'NONE',  ( 78.14518615778180788, 39.31328125108392868, 5.444914386472293977 ) ) ;
#25995 = CARTESIAN_POINT ( 'NONE',  ( -8.312177448680279460E-16, 31.37578125216787583, -13.57481594606304576 ) ) ;
#25996 = CARTESIAN_POINT ( 'NONE',  ( 208.1451861577818079, 38.56914062608393579, -1.609821015232357215E-15 ) ) ;
#25997 = CARTESIAN_POINT ( 'NONE',  ( -5.444914386472297529, 39.01562500108394005, -13.14518615778179722 ) ) ;
#25998 = DIRECTION ( 'NONE',  ( 0.000000000000000000, 0.000000000000000000, -1.000000000000000000 ) ) ;
#25999 = CARTESIAN_POINT ( 'NONE',  ( -13.57481594606304576, 37.82499999999999574, 0.000000000000000000 ) ) ;
#26000 = CYLINDRICAL_SURFACE ( 'NONE', #1820, 13.57481594606304576 ) ;
#26001 = CARTESIAN_POINT ( 'NONE',  ( 106.5389055433250860, 114.7507929638356785, -52.42499999726882010 ) ) ;
#26002 = VERTEX_POINT ( 'NONE', #18042 ) ;
#26003 = CARTESIAN_POINT ( 'NONE',  ( 13.57481594606304753, 35.89023437499999858, -5.622872871577873077 ) ) ;
#26004 = CARTESIAN_POINT ( 'NONE',  ( 13.14518615778179544, 37.77539062608393294, -1.609821015232357215E-15 ) ) ;
#26005 = CARTESIAN_POINT ( 'NONE',  ( 103.5355339059327093, 3.535533905932755072, 0.7500000027311857220 ) ) ;
#26006 = CARTESIAN_POINT ( 'NONE',  ( 120.7049497278729575, 36.08867187608393579, 9.295050272127047819 ) ) ;
#26007 = CARTESIAN_POINT ( 'NONE',  ( 70.44491438647230552, 32.36796875108393579, -13.14518615778179900 ) ) ;
#26008 = CARTESIAN_POINT ( 'NONE',  ( 185.7049497278729575, 37.47773437608393010, -9.295050272127046043 ) ) ;
#26009 = ADVANCED_FACE ( 'NONE', ( #7346, #16037 ), #20191, .F. ) ;
#26010 = CARTESIAN_POINT ( 'NONE',  ( 107.0000000000000142, 107.7255621263696526, -45.60000000546237686 ) ) ;
#26011 = CARTESIAN_POINT ( 'NONE',  ( -9.295050272127046043, 31.72304687608393081, -9.295050272127046043 ) ) ;
#26012 = CARTESIAN_POINT ( 'NONE',  ( 133.8639252651224467, 54.10645156200379802, -14.99999999999999467 ) ) ;
#26013 = CARTESIAN_POINT ( 'NONE',  ( 2.493653234604083739E-15, 38.91640625216786731, 13.57481594606304576 ) ) ;
#26014 = CARTESIAN_POINT ( 'NONE',  ( -9.295050272127044266, 33.70742187608393436, 9.295050272127047819 ) ) ;
#26015 = DIRECTION ( 'NONE',  ( 0.000000000000000000, 0.000000000000000000, -1.000000000000000000 ) ) ;
#26016 = CARTESIAN_POINT ( 'NONE',  ( -5.444914386472297529, 36.43593750108392726, -13.14518615778179900 ) ) ;
#26017 = LINE ( 'NONE', #23882, #16084 ) ;
#26018 = CARTESIAN_POINT ( 'NONE',  ( 104.9999999999999716, 79.68750000273119838, -2.071067811865491937 ) ) ;
#26019 = CARTESIAN_POINT ( 'NONE',  ( 56.22739075386999730, 50.37415326813798089, 14.99999999999999112 ) ) ;
#26020 = EDGE_LOOP ( 'NONE', ( #7593, #23008, #22192, #2364 ) ) ;
#26021 = CARTESIAN_POINT ( 'NONE',  ( 95.54126587499995082, -1.846868145590724986, 10.50000000136559208 ) ) ;
#26022 = ORIENTED_EDGE ( 'NONE', *, *, #8955, .F. ) ;
#26023 = CARTESIAN_POINT ( 'NONE',  ( 102.0669872999999939, 124.2000000010924907, -0.8561741729129507261 ) ) ;
#26024 = CARTESIAN_POINT ( 'NONE',  ( 95.54126587499996504, 1.387778780781445676E-14, 11.43750000136559208 ) ) ;
#26025 = DIRECTION ( 'NONE',  ( -0.000000000000000000, 1.000000000000000000, -0.000000000000000000 ) ) ;
#26026 = CARTESIAN_POINT ( 'NONE',  ( 5.444914386472297529, 40.30546875108393579, -13.14518615778179900 ) ) ;
#26027 = CYLINDRICAL_SURFACE ( 'NONE', #25424, 3.000000000000004441 ) ;
#26028 = CARTESIAN_POINT ( 'NONE',  ( 104.4587341249999639, 81.18750000136559208, -1.442382525525748735E-14 ) ) ;
#26029 = CARTESIAN_POINT ( 'NONE',  ( 51.85481384221819923, 36.73359375108393010, -5.444914386472297529 ) ) ;
#26030 = CARTESIAN_POINT ( 'NONE',  ( 99.99999999999998579, 118.4984768113314004, -51.62500000273119127 ) ) ;
#26031 = CYLINDRICAL_SURFACE ( 'NONE', #20524, 9.000000000000007105 ) ;
#26032 =( BOUNDED_CURVE ( )  B_SPLINE_CURVE ( 2, ( #5494, #1502, #10155, #24875, #3349 ),
 .UNSPECIFIED., .F., .F. ) 
 B_SPLINE_CURVE_WITH_KNOTS ( ( 3, 2, 3 ),
 ( 0.000000000000000000, 0.02500000000000002220, 0.05000000000000004441 ),
 .UNSPECIFIED. ) 
 CURVE ( )  GEOMETRIC_REPRESENTATION_ITEM ( )  RATIONAL_B_SPLINE_CURVE ( ( 1.000000000000000000, 0.9238795325112867385, 1.000000000000000000, 0.9238795325112866275, 1.000000000000000222 ) ) 
 REPRESENTATION_ITEM ( '' )  );
#26033 = ORIENTED_EDGE ( 'NONE', *, *, #17472, .F. ) ;
#26034 = CARTESIAN_POINT ( 'NONE',  ( 102.0710678118653618, 80.43750000273118417, 5.000000000000031086 ) ) ;
#26035 = CARTESIAN_POINT ( 'NONE',  ( 6.944426393311537993, 31.75150625057403175, -11.16113171639042356 ) ) ;
#26036 = CARTESIAN_POINT ( 'NONE',  ( 93.00000000000000000, 107.7255621263696526, -56.39999999453763024 ) ) ;
#26037 = CARTESIAN_POINT ( 'NONE',  ( 143.5748159460630688, 36.63437499999999858, -1.662435489736055892E-15 ) ) ;
#26038 = ORIENTED_EDGE ( 'NONE', *, *, #26373, .F. ) ;
#26039 = CARTESIAN_POINT ( 'NONE',  ( 99.99999999999995737, 1.387778780781445676E-14, 34.79898987322334136 ) ) ;
#26040 = CARTESIAN_POINT ( 'NONE',  ( -13.14518615778179900, 35.93984375108393436, -5.444914386472297529 ) ) ;
#26041 = CARTESIAN_POINT ( 'NONE',  ( -13.57481594606304576, 37.13046875216787868, 0.000000000000000000 ) ) ;
#26042 = CARTESIAN_POINT ( 'NONE',  ( 143.1451861577818079, 37.77539062608393294, -1.609821015232357215E-15 ) ) ;
#26043 = EDGE_CURVE ( 'NONE', #25384, #6320, #9631, .T. ) ;
#26044 = CARTESIAN_POINT ( 'NONE',  ( 51.42518405393695957, 32.36796875216787583, 0.000000000000000000 ) ) ;
#26045 = CARTESIAN_POINT ( 'NONE',  ( 13.04200858114962713, 35.99999999999998579, -3.640726557254823081 ) ) ;
#26046 = CARTESIAN_POINT ( 'NONE',  ( -13.57481594606304753, 36.28710937716787299, -5.622872871577873077 ) ) ;
#26047 = EDGE_CURVE ( 'NONE', #2435, #10403, #14376, .T. ) ;
#26048 = CARTESIAN_POINT ( 'NONE',  ( 102.0710678118654329, -4.999999999999989342, 6.312499999999999112 ) ) ;
#26049 = CARTESIAN_POINT ( 'NONE',  ( 99.99999999999997158, 118.4984768113314146, -48.37499999726881583 ) ) ;
#26050 = CARTESIAN_POINT ( 'NONE',  ( 208.1451861577817795, 36.93203125108394147, 5.444914386472293977 ) ) ;
#26051 = CARTESIAN_POINT ( 'NONE',  ( 214.9999999999999716, 55.00000000000000000, -9.999999999999998224 ) ) ;
#26052 = VECTOR ( 'NONE', #5396, 1000.000000000000000 ) ;
#26053 = EDGE_CURVE ( 'NONE', #26480, #20976, #3342, .T. ) ;
#26054 = CARTESIAN_POINT ( 'NONE',  ( 189.3771271284220177, 37.77539062716787299, -13.57481594606295339 ) ) ;
#26055 = CARTESIAN_POINT ( 'NONE',  ( 102.0710678118654329, 5.000000000000018652, 6.687499999999999112 ) ) ;
#26056 = CARTESIAN_POINT ( 'NONE',  ( 107.0000000000000000, 110.0000000000000000, -47.49999999453763877 ) ) ;
#26057 = CARTESIAN_POINT ( 'NONE',  ( -9.598844408820458085, 37.72578124999999005, -9.598844408820458085 ) ) ;
#26058 = CARTESIAN_POINT ( 'NONE',  ( 96.46446609406721961, -3.535533905932727539, 12.25000000273118594 ) ) ;
#26059 = CARTESIAN_POINT ( 'NONE',  ( -5.444914386472299306, 38.51953125108393294, 13.14518615778179722 ) ) ;
#26060 = CARTESIAN_POINT ( 'NONE',  ( -13.14518615778179544, 40.55351562608393579, 0.000000000000000000 ) ) ;
#26061 = CARTESIAN_POINT ( 'NONE',  ( 181.4251840539369596, 33.01289062500000426, -5.622872871577873077 ) ) ;
#26062 = CARTESIAN_POINT ( 'NONE',  ( 93.46109445667491400, 105.2492070361643215, -45.17500000273119554 ) ) ;
#26063 = CARTESIAN_POINT ( 'NONE',  ( 99.99999999999995737, -4.458734124999988779, 0.9375000013655925279 ) ) ;
#26064 = CARTESIAN_POINT ( 'NONE',  ( 55.70494972787295751, 34.30273437608393294, 9.295050272127047819 ) ) ;
#26065 = CARTESIAN_POINT ( 'NONE',  ( 101.8468681455907046, 4.458734125000016313, 3.125000001365592528 ) ) ;
#26066 = CARTESIAN_POINT ( 'NONE',  ( 130.0000000000000000, 36.00000000000000000, -1.503427012513233026E-14 ) ) ;
#26067 = CARTESIAN_POINT ( 'NONE',  ( 101.8468681455907330, 91.49999999863440792, -4.458734124999994997 ) ) ;
#26068 = CARTESIAN_POINT ( 'NONE',  ( 104.9999999999999716, 2.071067811865491937, 4.562500000000000000 ) ) ;
#26069 = CARTESIAN_POINT ( 'NONE',  ( 13.57481594606304576, 37.42812499999999432, -1.662435489736055892E-15 ) ) ;
#26070 = CARTESIAN_POINT ( 'NONE',  ( -20.00000000000000000, 80.00000000000000000, 15.00000000000000178 ) ) ;
#26071 = ORIENTED_EDGE ( 'NONE', *, *, #24275, .T. ) ;
#26072 = CARTESIAN_POINT ( 'NONE',  ( 103.5355339059327093, 84.62500000000000000, -3.535533905932755072 ) ) ;
#26073 = CARTESIAN_POINT ( 'NONE',  ( 104.4587341249999781, 94.31249999863440792, -6.938893903907228378E-15 ) ) ;
#26074 = CARTESIAN_POINT ( 'NONE',  ( 67.00729701006973471, 35.99999999999998579, -13.40042260803721419 ) ) ;
#26075 = ORIENTED_EDGE ( 'NONE', *, *, #6201, .T. ) ;
#26076 = AXIS2_PLACEMENT_3D ( 'NONE', #5048, #2903, #18441 ) ;
#26077 =( BOUNDED_CURVE ( )  B_SPLINE_CURVE ( 2, ( #25835, #12976, #4179, #27984, #19560, #16992, #6040, #17133, #12841, #2043, #6309 ),
 .UNSPECIFIED., .F., .F. ) 
 B_SPLINE_CURVE_WITH_KNOTS ( ( 3, 2, 2, 2, 2, 3 ),
 ( 0.9000000000000000222, 0.9200000000000000400, 0.9399999999999999467, 0.9599999999999999645, 0.9799999999999999822, 1.000000000000000000 ),
 .UNSPECIFIED. ) 
 CURVE ( )  GEOMETRIC_REPRESENTATION_ITEM ( )  RATIONAL_B_SPLINE_CURVE ( ( 1.000000000000000000, 0.9510565162951535312, 1.000000000000000000, 0.9510565162951535312, 1.000000000000000000, 0.9510565162951535312, 1.000000000000000000, 0.9510565162951535312, 1.000000000000000000, 0.9510565162951535312, 1.000000000000000000 ) ) 
 REPRESENTATION_ITEM ( '' )  );
#26078 = CARTESIAN_POINT ( 'NONE',  ( 99.99999999999997158, 102.6397644303321215, -50.50000000000000000 ) ) ;
#26079 = CARTESIAN_POINT ( 'NONE',  ( 55.70494972787295751, 34.30273437608393294, -9.295050272127046043 ) ) ;
#26080 = ORIENTED_EDGE ( 'NONE', *, *, #20686, .F. ) ;
#26081 = CARTESIAN_POINT ( 'NONE',  ( -9.598844408820454532, 33.26093750216787726, 9.598844408820459861 ) ) ;
#26082 = ADVANCED_FACE ( 'NONE', ( #18336 ), #27043, .T. ) ;
#26083 = CARTESIAN_POINT ( 'NONE',  ( 95.54126587499996504, 1.387778780781445676E-14, 3.687500001365593416 ) ) ;
#26084 = ORIENTED_EDGE ( 'NONE', *, *, #26446, .T. ) ;
#26085 = CARTESIAN_POINT ( 'NONE',  ( 13.14518615778179722, 34.05468750108394005, -5.444914386472297529 ) ) ;
#26086 = CARTESIAN_POINT ( 'NONE',  ( 13.14518615778179900, 39.61093750108393863, -5.444914386472297529 ) ) ;
#26087 = UNCERTAINTY_MEASURE_WITH_UNIT (LENGTH_MEASURE( 1.000000000000000082E-05 ), #4325, 'distance_accuracy_value', 'NONE');
#26088 = CARTESIAN_POINT ( 'NONE',  ( 181.4251840539369596, 37.18007812716787441, 5.622872871577880183 ) ) ;
#26089 = CARTESIAN_POINT ( 'NONE',  ( 2.414731522848535132E-15, 35.98945312608393010, 13.14518615778179544 ) ) ;
#26090 = CARTESIAN_POINT ( 'NONE',  ( 51.63999894807758295, 40.42949218912590936, 0.000000000000000000 ) ) ;
#26091 = CARTESIAN_POINT ( 'NONE',  ( 195.9830651850982406, 49.99999999949031348, 13.54930971656779626 ) ) ;
#26092 = CARTESIAN_POINT ( 'NONE',  ( 208.5748159460630688, 39.90859375216787441, -1.662435489736055892E-15 ) ) ;
#26093 = ORIENTED_EDGE ( 'NONE', *, *, #648, .T. ) ;
#26094 = CARTESIAN_POINT ( 'NONE',  ( 2.414731522848535132E-15, 38.56914062608393579, 13.14518615778179544 ) ) ;
#26095 = CARTESIAN_POINT ( 'NONE',  ( 120.7049497278729575, 35.69179687608393436, -9.295050272127046043 ) ) ;
#26096 = CARTESIAN_POINT ( 'NONE',  ( 78.57481594606305464, 34.25312499999999716, -1.662435489736055892E-15 ) ) ;
#26097 = CARTESIAN_POINT ( 'NONE',  ( 103.5355339059327093, 3.535533905932755072, 9.624999999999998224 ) ) ;
#26098 = CARTESIAN_POINT ( 'NONE',  ( 104.4587341249999639, 1.442382525525748735E-14, 9.187500001365592084 ) ) ;
#26100 = CARTESIAN_POINT ( 'NONE',  ( 99.99999999999998579, 110.0000000000000000, -145.0000000000000284 ) ) ;
#26099 = CIRCLE ( 'NONE', #16994, 5.000000000000000888 ) ;
#26101 = CARTESIAN_POINT ( 'NONE',  ( 95.54126587499995082, -1.846868145590724986, 1.500000001365591418 ) ) ;
#26102 = CARTESIAN_POINT ( 'NONE',  ( 96.46446615806316061, 80.00000000000000000, -3.535533969928681852 ) ) ;
#26103 = CARTESIAN_POINT ( 'NONE',  ( 99.99999999999995737, 1.387778780781445676E-14, 0.000000000000000000 ) ) ;
#26104 = CARTESIAN_POINT ( 'NONE',  ( 96.84719886470459471, 80.56250000136559208, -3.152801135295383084 ) ) ;
#26105 = CARTESIAN_POINT ( 'NONE',  ( 91.91746824999997045, 112.6261737610028320, -49.72499999726882436 ) ) ;
#26106 = CARTESIAN_POINT ( 'NONE',  ( 13.14518615778179900, 35.54296875108394715, 5.444914386472293977 ) ) ;
#26107 = CARTESIAN_POINT ( 'NONE',  ( 93.46109445667489979, 105.2492070361643215, -49.67499999726882010 ) ) ;
#26108 = VERTEX_POINT ( 'NONE', #22763 ) ;
#26109 = CARTESIAN_POINT ( 'NONE',  ( -20.00000000000000355, 55.00000000000000000, -9.999999999999998224 ) ) ;
#26110 = CYLINDRICAL_SURFACE ( 'NONE', #1626, 13.57481594606304398 ) ;
#26111 = DIRECTION ( 'NONE',  ( 1.000000000000000000, 0.000000000000000000, 0.000000000000000000 ) ) ;
#26112 = CARTESIAN_POINT ( 'NONE',  ( 189.5550856135277229, 37.52734375108393294, 13.14518615778179722 ) ) ;
#26113 =( BOUNDED_CURVE ( )  B_SPLINE_CURVE ( 2, ( #14918, #8105, #4115, #23774, #25496, #1847, #8239, #10783, #10509, #23227, #19215 ),
 .UNSPECIFIED., .F., .T. ) 
 B_SPLINE_CURVE_WITH_KNOTS ( ( 3, 2, 2, 2, 2, 3 ),
 ( 0.5999999999999998668, 0.6199999999999998845, 0.6399999999999999023, 0.6599999999999999201, 0.6799999999999999378, 0.6999999999999998446 ),
 .UNSPECIFIED. ) 
 CURVE ( )  GEOMETRIC_REPRESENTATION_ITEM ( )  RATIONAL_B_SPLINE_CURVE ( ( 1.000000000000000222, 0.9510565162951533091, 1.000000000000000000, 0.9510565162951535312, 1.000000000000000000, 0.9510565162951535312, 1.000000000000000000, 0.9510565162951535312, 1.000000000000000000, 0.9510565162951537532, 0.9999999999999997780 ) ) 
 REPRESENTATION_ITEM ( '' )  );
#26114 = ORIENTED_EDGE ( 'NONE', *, *, #10025, .T. ) ;
#26115 = CARTESIAN_POINT ( 'NONE',  ( 104.9999999999999716, 1.449011120738813565E-14, 9.625000002731184168 ) ) ;
#26116 = DIRECTION ( 'NONE',  ( 5.782411586589358625E-17, -0.000000000000000000, 1.000000000000000000 ) ) ;
#26117 = CARTESIAN_POINT ( 'NONE',  ( 104.4587341249999639, 1.442382525525748735E-14, 14.18750000136559208 ) ) ;
#26118 = ORIENTED_EDGE ( 'NONE', *, *, #13074, .F. ) ;
#26119 = CARTESIAN_POINT ( 'NONE',  ( 107.0000000000000142, 112.2744378736303332, -48.90000000000000568 ) ) ;
#26120 = CARTESIAN_POINT ( 'NONE',  ( -13.14518615778179900, 38.91640625108393436, -5.444914386472297529 ) ) ;
#26121 = CARTESIAN_POINT ( 'NONE',  ( 101.4615807364564546, 123.4500000010924765, 1.461580736456455476 ) ) ;
#26122 = CARTESIAN_POINT ( 'NONE',  ( 130.0000000000000000, 39.16445312608392726, 13.14518615778179544 ) ) ;
#26123 = CARTESIAN_POINT ( 'NONE',  ( -9.295050272127044266, 40.05742187608393579, 9.295050272127047819 ) ) ;
#26124 = CARTESIAN_POINT ( 'NONE',  ( 102.0710678118654613, 92.68749999726883004, 4.999999999999983125 ) ) ;
#26125 = CARTESIAN_POINT ( 'NONE',  ( 65.00000000000000000, 39.36289062608393152, 13.14518615778179544 ) ) ;
#26126 = CARTESIAN_POINT ( 'NONE',  ( 84.99999999999998579, 118.0000000000000000, -13.00000000000000711 ) ) ;
#26127 = ORIENTED_EDGE ( 'NONE', *, *, #23963, .T. ) ;
#26128 = CARTESIAN_POINT ( 'NONE',  ( 181.8548138422181921, 33.55859375108393294, -5.444914386472297529 ) ) ;
#26129 = ORIENTED_EDGE ( 'NONE', *, *, #24303, .F. ) ;
#26130 = ADVANCED_FACE ( 'NONE', ( #7638 ), #6388, .T. ) ;
#26131 = ORIENTED_EDGE ( 'NONE', *, *, #21153, .T. ) ;
#26132 = CARTESIAN_POINT ( 'NONE',  ( 9.295050272127046043, 40.45429687608393721, -9.295050272127046043 ) ) ;
#26133 = CARTESIAN_POINT ( 'NONE',  ( 96.84719886470459471, -3.152801135295355994, 11.81250000136559208 ) ) ;
#26134 = CARTESIAN_POINT ( 'NONE',  ( 55.70494972787295751, 39.66054687608393436, -9.295050272127046043 ) ) ;
#26135 = CARTESIAN_POINT ( 'NONE',  ( 95.54126587499996504, 81.50000000136560629, 1.846868145590724986 ) ) ;
#26136 = CARTESIAN_POINT ( 'NONE',  ( 200.4449143864723055, 39.51171875108393294, -13.14518615778179722 ) ) ;
#26137 = CARTESIAN_POINT ( 'NONE',  ( -5.444914386472297529, 38.22187500108393721, -13.14518615778179722 ) ) ;
#26138 = CARTESIAN_POINT ( 'NONE',  ( 186.2416656076466097, 50.00000000000000000, 10.38725784495168192 ) ) ;
#26139 = CARTESIAN_POINT ( 'NONE',  ( -8.312177448680279460E-16, 37.62656249999999858, -13.57481594606304576 ) ) ;
#26140 = CARTESIAN_POINT ( 'NONE',  ( 185.7049497278729575, 40.65273437608393436, -9.295050272127046043 ) ) ;
#26141 = CARTESIAN_POINT ( 'NONE',  ( 97.50236033167490746, 117.6869444889999841, -52.02499999726882862 ) ) ;
#26142 = ORIENTED_EDGE ( 'NONE', *, *, #4985, .F. ) ;
#26143 = VECTOR ( 'NONE', #5483, 1000.000000000000000 ) ;
#26144 = CARTESIAN_POINT ( 'NONE',  ( -8.312177448680279460E-16, 36.03906250000000000, -13.57481594606304576 ) ) ;
#26145 = CARTESIAN_POINT ( 'NONE',  ( 9.295050272127047819, 37.67617187608393436, 9.295050272127046043 ) ) ;
#26146 = CARTESIAN_POINT ( 'NONE',  ( 99.99999999999995737, -4.999999999999990230, 0.3750000027311853890 ) ) ;
#26147 = CARTESIAN_POINT ( 'NONE',  ( 124.5550856135277087, 35.84062500108394289, -13.14518615778179900 ) ) ;
#26148 = CARTESIAN_POINT ( 'NONE',  ( 74.29505027212704249, 32.91367187608393152, 9.295050272127046043 ) ) ;
#26149 = CARTESIAN_POINT ( 'NONE',  ( 204.2950502721270425, 37.87460937608393863, 9.295050272127046043 ) ) ;
#26150 = CARTESIAN_POINT ( 'NONE',  ( 204.1801758136480203, 55.00000000000000000, 14.99999999999994671 ) ) ;
#26151 =( NAMED_UNIT ( * ) PLANE_ANGLE_UNIT ( ) SI_UNIT ( $, .RADIAN. ) );
#26152 = CARTESIAN_POINT ( 'NONE',  ( 126.1969456267529921, 54.09082899096177499, -15.00000000000000355 ) ) ;
#26153 = DIRECTION ( 'NONE',  ( 0.000000000000000000, -1.000000000000000000, 0.000000000000000000 ) ) ;
#26154 = FACE_OUTER_BOUND ( 'NONE', #6617, .T. ) ;
#26155 = CARTESIAN_POINT ( 'NONE',  ( 91.91746824999999887, 110.0000000000000000, -51.12500000273119127 ) ) ;
#26156 = CARTESIAN_POINT ( 'NONE',  ( 13.14518615778179544, 36.18789062608393436, -1.609821015232357215E-15 ) ) ;
#26157 = FACE_OUTER_BOUND ( 'NONE', #24800, .T. ) ;
#26158 = CARTESIAN_POINT ( 'NONE',  ( 104.9999999999999716, 79.62500000273119838, -1.449011120738813565E-14 ) ) ;
#26159 = CARTESIAN_POINT ( 'NONE',  ( 99.99999999999998579, 124.3999999999999915, 2.499999999999978684 ) ) ;
#26160 = ADVANCED_FACE ( 'NONE', ( #26659 ), #13659, .T. ) ;
#26161 = VECTOR ( 'NONE', #5241, 1000.000000000000000 ) ;
#26162 = LINE ( 'NONE', #17325, #3174 ) ;
#26163 = CARTESIAN_POINT ( 'NONE',  ( 103.1528011352953342, 3.152801135295383084, 7.062500001365592084 ) ) ;
#26164 = ORIENTED_EDGE ( 'NONE', *, *, #618, .T. ) ;
#26165 = CARTESIAN_POINT ( 'NONE',  ( 98.96446609406727646, 123.3500000021849701, -2.499999999999997780 ) ) ;
#26166 = CARTESIAN_POINT ( 'NONE',  ( 103.1528011352953342, -3.152801135295355106, 10.81250000136559208 ) ) ;
#26167 = CYLINDRICAL_SURFACE ( 'NONE', #12291, 4.999999999999989342 ) ;
#26168 = CARTESIAN_POINT ( 'NONE',  ( 13.14518615778179900, 38.51953125108393294, 5.444914386472293977 ) ) ;
#26169 = CARTESIAN_POINT ( 'NONE',  ( -13.14518615778179544, 40.65273437608393436, 0.000000000000000000 ) ) ;
#26170 = CARTESIAN_POINT ( 'NONE',  ( 96.84719886470459471, 80.81250000136559208, 3.152801135295355994 ) ) ;
#26171 = CARTESIAN_POINT ( 'NONE',  ( 78.14518615778179367, 33.95546875108393436, 5.444914386472293977 ) ) ;
#26172 = CARTESIAN_POINT ( 'NONE',  ( 106.5389055433251002, 105.2492070361643215, -52.32500000273119412 ) ) ;
#26173 = CARTESIAN_POINT ( 'NONE',  ( 9.295050272127046043, 37.08085937608393579, -9.295050272127046043 ) ) ;
#26174 = CARTESIAN_POINT ( 'NONE',  ( -5.622872871578011633, 39.56132812500000284, 13.57481594606290720 ) ) ;
#26175 = DIRECTION ( 'NONE',  ( -0.000000000000000000, -1.000000000000000000, -0.000000000000000000 ) ) ;
#26176 = CARTESIAN_POINT ( 'NONE',  ( 107.0000000000000000, 112.2744378736303190, -55.39999999453763735 ) ) ;
#26177 = CARTESIAN_POINT ( 'NONE',  ( 130.0000000000000000, 37.22968749999999716, 13.57481594606304576 ) ) ;
#26178 = VERTEX_POINT ( 'NONE', #11233 ) ;
#26179 = CARTESIAN_POINT ( 'NONE',  ( 104.9999999999999716, -2.071067811865452857, 8.437500000000000000 ) ) ;
#26180 = CARTESIAN_POINT ( 'NONE',  ( -9.295050272127044266, 35.29492187608393294, 9.295050272127047819 ) ) ;
#26181 = CARTESIAN_POINT ( 'NONE',  ( -8.312177448680279460E-16, 36.13828125216787157, -13.57481594606304576 ) ) ;
#26182 = CARTESIAN_POINT ( 'NONE',  ( 130.0000000000000000, 37.97382812608393721, -13.14518615778179544 ) ) ;
#26183 = CARTESIAN_POINT ( 'NONE',  ( 78.57481594606305464, 32.76484375216787015, -1.662435489736055892E-15 ) ) ;
#26184 = VECTOR ( 'NONE', #5984, 1000.000000000000000 ) ;
#26185 = DIRECTION ( 'NONE',  ( -1.000000000000000000, 0.000000000000000000, 0.000000000000000000 ) ) ;
#26186 = CARTESIAN_POINT ( 'NONE',  ( -13.57481594606304576, 32.36796875216787583, 0.000000000000000000 ) ) ;
#26187 = CARTESIAN_POINT ( 'NONE',  ( 96.46446609406721961, 3.535533905932755072, 3.875000000000000000 ) ) ;
#26188 = CARTESIAN_POINT ( 'NONE',  ( 104.9952793366501567, 116.8754121666685393, -46.57499999726881157 ) ) ;
#26189 = EDGE_CURVE ( 'NONE', #11798, #27263, #14207, .T. ) ;
#26190 = CARTESIAN_POINT ( 'NONE',  ( 185.7049497278729575, 33.50898437608393010, 9.295050272127047819 ) ) ;
#26191 = AXIS2_PLACEMENT_3D ( 'NONE', #17275, #10576, #8725 ) ;
#26192 = CIRCLE ( 'NONE', #4348, 5.000000000000000888 ) ;
#26193 = FACE_OUTER_BOUND ( 'NONE', #2942, .T. ) ;
#26194 = EDGE_LOOP ( 'NONE', ( #21726, #26691, #7457, #8181 ) ) ;
#26195 = CARTESIAN_POINT ( 'NONE',  ( 181.4251840539369596, 40.15664062499999432, -5.622872871577872189 ) ) ;
#26196 = CARTESIAN_POINT ( 'NONE',  ( 87.00000000000000000, 100.0000000000000000, -13.00000000000000533 ) ) ;
#26197 = CARTESIAN_POINT ( 'NONE',  ( -13.57481594606304576, 32.36796875216787583, 0.000000000000000000 ) ) ;
#26198 = CARTESIAN_POINT ( 'NONE',  ( 5.622872871577871301, 36.78320312499999289, -13.57481594606304753 ) ) ;
#26199 = CYLINDRICAL_SURFACE ( 'NONE', #25271, 13.57481594606304398 ) ;
#26200 =( BOUNDED_CURVE ( )  B_SPLINE_CURVE ( 2, ( #16184, #3226, #22187, #17903, #24609, #24747, #9629, #9769, #9350 ),
 .UNSPECIFIED., .F., .F. ) 
 B_SPLINE_CURVE_WITH_KNOTS ( ( 3, 2, 2, 2, 3 ),
 ( 0.5208333333333332593, 0.5312499999999997780, 0.5416666666666664076, 0.5520833333333330373, 0.5624999999999996669 ),
 .UNSPECIFIED. ) 
 CURVE ( )  GEOMETRIC_REPRESENTATION_ITEM ( )  RATIONAL_B_SPLINE_CURVE ( ( 1.000000000000000888, 0.9238795325112859613, 1.000000000000000000, 0.9238795325112867385, 1.000000000000000000, 0.9238795325112867385, 1.000000000000000000, 0.9238795325112891810, 0.9999999999999975575 ) ) 
 REPRESENTATION_ITEM ( '' )  );
#26201 = CARTESIAN_POINT ( 'NONE',  ( 9.295050272127046043, 38.07304687608393579, -9.295050272127046043 ) ) ;
#26202 = CARTESIAN_POINT ( 'NONE',  ( -13.14518615778179544, 36.58476562608393579, 0.000000000000000000 ) ) ;
#26203 = EDGE_CURVE ( 'NONE', #18001, #15330, #25702, .T. ) ;
#26204 = CARTESIAN_POINT ( 'NONE',  ( 195.0000000000000000, 35.64218749999999147, 13.57481594606304576 ) ) ;
#26205 = CARTESIAN_POINT ( 'NONE',  ( 102.4976396683250925, 102.3130555110000159, -46.77500000273119696 ) ) ;
#26206 = CARTESIAN_POINT ( 'NONE',  ( 99.99999988184244160, 117.0000000000000000, -45.00000000000000711 ) ) ;
#26207 = CARTESIAN_POINT ( 'NONE',  ( 51.85481384221820633, 34.25312500108393010, 5.444914386472304635 ) ) ;
#26208 = EDGE_CURVE ( 'NONE', #20844, #5424, #18088, .T. ) ;
#26209 = CARTESIAN_POINT ( 'NONE',  ( 99.99999999999995737, 4.458734125000016313, 3.187500001365592972 ) ) ;
#26210 = LINE ( 'NONE', #12512, #21 ) ;
#26211 = CARTESIAN_POINT ( 'NONE',  ( 99.99999999999998579, 91.56249999863440792, -4.458734124999994997 ) ) ;
#26212 = CARTESIAN_POINT ( 'NONE',  ( 97.92893218813455292, 93.56249999726884425, 5.000000000000011546 ) ) ;
#26213 = CARTESIAN_POINT ( 'NONE',  ( 13.57481594606304931, 35.79101562499999289, 5.622872871577869525 ) ) ;
#26214 = CARTESIAN_POINT ( 'NONE',  ( 135.4449143864723055, 38.61875000108393152, 13.14518615778179189 ) ) ;
#26215 = EDGE_CURVE ( 'NONE', #4003, #24599, #6549, .T. ) ;
#26216 = ORIENTED_EDGE ( 'NONE', *, *, #23255, .F. ) ;
#26217 = ORIENTED_EDGE ( 'NONE', *, *, #2565, .T. ) ;
#26218 = CARTESIAN_POINT ( 'NONE',  ( 103.1528011352953342, 80.31250000136559208, -3.152801135295383084 ) ) ;
#26219 = CARTESIAN_POINT ( 'NONE',  ( 94.99999999999995737, 83.18750000273119838, 2.071067811865466624 ) ) ;
#26220 = AXIS2_PLACEMENT_3D ( 'NONE', #4100, #24182, #6505 ) ;
#26221 = CARTESIAN_POINT ( 'NONE',  ( 99.99999999999998579, 93.06249999863440792, 4.458734124999981674 ) ) ;
#26222 = CARTESIAN_POINT ( 'NONE',  ( 63.18349958271478073, 36.00000000000000711, -13.35830014193481929 ) ) ;
#26223 = EDGE_CURVE ( 'NONE', #1875, #15313, #1009, .T. ) ;
#26224 = CARTESIAN_POINT ( 'NONE',  ( 95.67376207875069838, 104.0454443415356991, -52.70000000000000284 ) ) ;
#26225 = CARTESIAN_POINT ( 'NONE',  ( 59.55508561352770158, 35.04687500108393294, -13.14518615778179900 ) ) ;
#26226 = VERTEX_POINT ( 'NONE', #24933 ) ;
#26227 = DIRECTION ( 'NONE',  ( -0.000000000000000000, -1.000000000000000000, -0.000000000000000000 ) ) ;
#26228 = CARTESIAN_POINT ( 'NONE',  ( 96.84719886470459471, -3.152801135295355994, 3.812500001365591640 ) ) ;
#26229 = ORIENTED_EDGE ( 'NONE', *, *, #14634, .F. ) ;
#26230 = CARTESIAN_POINT ( 'NONE',  ( -5.444914386472297529, 35.84062500108394289, -13.14518615778179722 ) ) ;
#26231 = CARTESIAN_POINT ( 'NONE',  ( -8.049105076161786076E-16, 38.17226562608394147, -13.14518615778179544 ) ) ;
#26232 = CARTESIAN_POINT ( 'NONE',  ( 189.3771271284221314, 34.89804687716787868, 13.57481594606304753 ) ) ;
#26233 = CIRCLE ( 'NONE', #13929, 13.57481594606304398 ) ;
#26234 = CARTESIAN_POINT ( 'NONE',  ( -9.295050272127046043, 34.89804687608393152, -9.295050272127046043 ) ) ;
#26235 = CARTESIAN_POINT ( 'NONE',  ( -13.57481594606304576, 40.99999999999999289, 0.000000000000000000 ) ) ;
#26236 = EDGE_CURVE ( 'NONE', #4294, #4960, #20214, .T. ) ;
#26237 = DIRECTION ( 'NONE',  ( -0.000000000000000000, 1.000000000000000000, 0.000000000000000000 ) ) ;
#26238 = EDGE_LOOP ( 'NONE', ( #21035, #25649, #15729, #19408 ) ) ;
#26239 = CARTESIAN_POINT ( 'NONE',  ( 9.295050272127046043, 37.27929687608394005, -9.295050272127046043 ) ) ;
#26240 = CARTESIAN_POINT ( 'NONE',  ( 143.1451861577818079, 34.55078125108393294, 5.444914386472293977 ) ) ;
#26241 = CARTESIAN_POINT ( 'NONE',  ( 59.37712712842213136, 36.08867187500000284, -13.57481594606304753 ) ) ;
#26242 = CARTESIAN_POINT ( 'NONE',  ( -8.312177448680279460E-16, 38.51953125216787299, -13.57481594606304576 ) ) ;
#26243 = CARTESIAN_POINT ( 'NONE',  ( 99.99999999999995737, 4.458734125000016313, 12.43750000136559208 ) ) ;
#26244 = DIRECTION ( 'NONE',  ( 7.228014483236696740E-18, 0.000000000000000000, 1.000000000000000000 ) ) ;
#26246 = ADVANCED_FACE ( 'NONE', ( #16236 ), #9298, .T. ) ;
#26245 = CARTESIAN_POINT ( 'NONE',  ( 101.8468681455907046, 4.458734125000016313, 13.12500000136559208 ) ) ;
#26247 = CARTESIAN_POINT ( 'NONE',  ( 108.0825317500000011, 112.6261737610028320, -50.02500000273118275 ) ) ;
#26248 = CARTESIAN_POINT ( 'NONE',  ( 102.4999999999999858, 123.8500000000000085, -1.035533905932742638 ) ) ;
#26249 = CARTESIAN_POINT ( 'NONE',  ( -8.312177448680279460E-16, 40.80156249999999574, -13.57481594606304576 ) ) ;
#26250 = CARTESIAN_POINT ( 'NONE',  ( 102.4976396683250783, 117.6869444889999841, -46.22499999726882436 ) ) ;
#26251 = CARTESIAN_POINT ( 'NONE',  ( -13.14518615778179544, 35.19570312608393436, 0.000000000000000000 ) ) ;
#26252 = EDGE_CURVE ( 'NONE', #16430, #19618, #23134, .T. ) ;
#26253 = CARTESIAN_POINT ( 'NONE',  ( 108.0825317499999869, 107.3738262389971538, -50.97499999726881015 ) ) ;
#26254 = ORIENTED_EDGE ( 'NONE', *, *, #22954, .F. ) ;
#26255 = LINE ( 'NONE', #8717, #14966 ) ;
#26256 =( BOUNDED_CURVE ( )  B_SPLINE_CURVE ( 2, ( #17580, #2209, #6746, #19583, #17440, #10872, #4623, #15431, #21876 ),
 .UNSPECIFIED., .F., .F. ) 
 B_SPLINE_CURVE_WITH_KNOTS ( ( 3, 2, 2, 2, 3 ),
 ( 0.06250000000000004163, 0.07291666666666665741, 0.08333333333333325932, 0.09374999999999987510, 0.1041666666666664909 ),
 .UNSPECIFIED. ) 
 CURVE ( )  GEOMETRIC_REPRESENTATION_ITEM ( )  RATIONAL_B_SPLINE_CURVE ( ( 0.9999999999999996669, 0.9238795325112870716, 1.000000000000000000, 0.9238795325112867385, 1.000000000000000000, 0.9238795325112867385, 1.000000000000000000, 0.9238795325112880708, 0.9999999999999986677 ) ) 
 REPRESENTATION_ITEM ( '' )  );
#26257 = AXIS2_PLACEMENT_3D ( 'NONE', #7192, #15889, #26894 ) ;
#26258 = DIRECTION ( 'NONE',  ( 0.000000000000000000, -1.000000000000000000, 0.000000000000000000 ) ) ;
#26259 = CARTESIAN_POINT ( 'NONE',  ( 0.000000000000000000, 40.99999999999999289, 0.000000000000000000 ) ) ;
#26260 = CARTESIAN_POINT ( 'NONE',  ( 208.1451861577817795, 38.61875000108393152, -5.444914386472297529 ) ) ;
#26261 = ORIENTED_EDGE ( 'NONE', *, *, #18000, .F. ) ;
#26262 = DIRECTION ( 'NONE',  ( 0.000000000000000000, 1.000000000000000000, 0.000000000000000000 ) ) ;
#26263 = LINE ( 'NONE', #6722, #13986 ) ;
#26264 = ORIENTED_EDGE ( 'NONE', *, *, #23963, .F. ) ;
#26265 = CARTESIAN_POINT ( 'NONE',  ( 105.6631189606246295, 114.1144967660473242, -52.80000000000000426 ) ) ;
#26266 = CARTESIAN_POINT ( 'NONE',  ( 2.414731522848535132E-15, 39.16445312608392726, 13.14518615778179544 ) ) ;
#26267 = CARTESIAN_POINT ( 'NONE',  ( 102.0669872999999939, 124.4000000010924651, -0.8561741729129507261 ) ) ;
#26268 = CARTESIAN_POINT ( 'NONE',  ( 135.6228728715778686, 32.91367187716787157, -13.57481594606304753 ) ) ;
#26269 = CARTESIAN_POINT ( 'NONE',  ( 217.9999999999999716, 52.00000000000000711, 0.000000000000000000 ) ) ;
#26270 = CARTESIAN_POINT ( 'NONE',  ( 102.0710678118654613, 92.06249999726880162, -4.999999999999997335 ) ) ;
#26271 = CLOSED_SHELL ( 'NONE', ( #14818, #21019, #17599, #25325, #27632, #7925, #3241, #16277, #18123, #13474, #7933, #24757, #5528, #10565, #26406, #5704, #6907, #15699, #12774, #27763, #6504, #24157, #11890, #23258, #1138, #4857, #25221, #3527, #18200, #22194, #14012, #13999, #19772, #20306, #16657, #10371, #1364, #26865, #19086 ) ) ;
#26272 = CARTESIAN_POINT ( 'NONE',  ( 55.70494972787295751, 39.06523437608392868, -9.295050272127046043 ) ) ;
#26273 = DIRECTION ( 'NONE',  ( 0.000000000000000000, -1.000000000000000000, 0.000000000000000000 ) ) ;
#26274 = CARTESIAN_POINT ( 'NONE',  ( 200.4449143864723055, 33.85625000108393579, 13.14518615778179189 ) ) ;
#26275 = EDGE_CURVE ( 'NONE', #2879, #11095, #12196, .T. ) ;
#26276 = VERTEX_POINT ( 'NONE', #7033 ) ;
#26277 = ORIENTED_EDGE ( 'NONE', *, *, #4304, .T. ) ;
#26278 = CARTESIAN_POINT ( 'NONE',  ( -8.049105076161786076E-16, 39.75976562608394005, -13.14518615778179544 ) ) ;
#26279 = DIRECTION ( 'NONE',  ( 1.000000000000000000, 0.000000000000000000, 0.000000000000000000 ) ) ;
#26280 = CARTESIAN_POINT ( 'NONE',  ( 96.84719886470459471, -3.152801135295355994, 9.812500001365593860 ) ) ;
#26281 = CARTESIAN_POINT ( 'NONE',  ( 9.598844408820459861, 38.12265624999999858, 9.598844408820456309 ) ) ;
#26282 = PRODUCT ( 'main air inlet', 'main air inlet', '', ( #27929 ) ) ;
#26283 = CARTESIAN_POINT ( 'NONE',  ( 96.84719886470459471, 82.31250000136559208, -3.152801135295383084 ) ) ;
#26284 = CARTESIAN_POINT ( 'NONE',  ( 185.7049497278729575, 38.07304687608393579, -9.295050272127046043 ) ) ;
#26285 = CARTESIAN_POINT ( 'NONE',  ( 13.14518615778179722, 38.71796875108393721, 5.444914386472293977 ) ) ;
#26286 = DIRECTION ( 'NONE',  ( 5.782411586589357392E-17, 3.469446951953611231E-16, 1.000000000000000000 ) ) ;
#26287 = FACE_OUTER_BOUND ( 'NONE', #14845, .T. ) ;
#26288 = CARTESIAN_POINT ( 'NONE',  ( 97.83688103937537051, 103.3426043859339103, -49.60000000000000853 ) ) ;
#26289 = CARTESIAN_POINT ( 'NONE',  ( 97.50236033167490746, 102.3130555110000159, -53.22499999726882436 ) ) ;
#26290 = VERTEX_POINT ( 'NONE', #20453 ) ;
#26291 = CARTESIAN_POINT ( 'NONE',  ( 9.598844408820456309, 37.52734375000000000, -9.598844408820458085 ) ) ;
#26292 = CARTESIAN_POINT ( 'NONE',  ( -5.444914386472297529, 35.64218750108392442, -13.14518615778179900 ) ) ;
#26293 = CIRCLE ( 'NONE', #5369, 24.13397459621556962 ) ;
#26294 = ORIENTED_EDGE ( 'NONE', *, *, #21282, .T. ) ;
#26295 = CARTESIAN_POINT ( 'NONE',  ( 143.1451861577818079, 37.13046875108393863, 5.444914386472293977 ) ) ;
#26296 = AXIS2_PLACEMENT_3D ( 'NONE', #17983, #21987, #17845 ) ;
#26297 = CARTESIAN_POINT ( 'NONE',  ( 51.85481384221820633, 33.45937500108392726, 5.444914386472304635 ) ) ;
#26298 = CARTESIAN_POINT ( 'NONE',  ( 181.8548138422181921, 38.32109375108394289, -5.444914386472297529 ) ) ;
#26299 = EDGE_LOOP ( 'NONE', ( #10988, #24663 ) ) ;
#26300 = DIRECTION ( 'NONE',  ( -0.000000000000000000, -0.000000000000000000, -1.000000000000000000 ) ) ;
#26301 = CARTESIAN_POINT ( 'NONE',  ( -9.295050272127044266, 32.71523437608393436, 9.295050272127047819 ) ) ;
#26302 = CARTESIAN_POINT ( 'NONE',  ( 130.8389268692911571, 53.50081894914646341, -15.00000000000000000 ) ) ;
#26303 = CARTESIAN_POINT ( 'NONE',  ( 143.5748159460630688, 39.90859375216787441, -1.662435489736055892E-15 ) ) ;
#26304 = CARTESIAN_POINT ( 'NONE',  ( 2.493653234604083739E-15, 39.61093749999999147, 13.57481594606304576 ) ) ;
#26305 = DIRECTION ( 'NONE',  ( 1.000000000000000000, 0.000000000000000000, 0.000000000000000000 ) ) ;
#26306 = CARTESIAN_POINT ( 'NONE',  ( 97.50000000000000000, 123.5000000021849615, -9.540979117872439019E-15 ) ) ;
#26307 = CARTESIAN_POINT ( 'NONE',  ( 2.816687638038913930E-15, 23.00000000000000000, 23.00000000000001421 ) ) ;
#26308 = VERTEX_POINT ( 'NONE', #11585 ) ;
#26309 =( NAMED_UNIT ( * ) PLANE_ANGLE_UNIT ( ) SI_UNIT ( $, .RADIAN. ) );
#26310 = CARTESIAN_POINT ( 'NONE',  ( 95.54126587499996504, 1.387778780781445676E-14, 10.43750000136559208 ) ) ;
#26311 = ORIENTED_EDGE ( 'NONE', *, *, #8641, .F. ) ;
#26312 = CARTESIAN_POINT ( 'NONE',  ( 97.93301269999999192, 124.5000000010924879, -0.8561741729129505041 ) ) ;
#26313 = CARTESIAN_POINT ( 'NONE',  ( 104.4587341249999781, -1.846868145590721655, 11.87500000136559031 ) ) ;
#26314 = CARTESIAN_POINT ( 'NONE',  ( 123.8822400544581228, 54.65941425415167032, 14.99999999999996980 ) ) ;
#26315 = VECTOR ( 'NONE', #2517, 1000.000000000000000 ) ;
#26316 = CARTESIAN_POINT ( 'NONE',  ( 13.14518615778179900, 39.41250000108393436, -5.444914386472297529 ) ) ;
#26317 = CARTESIAN_POINT ( 'NONE',  ( 116.4251840539369738, 38.76757812716787299, 5.622872871577880183 ) ) ;
#26318 = CARTESIAN_POINT ( 'NONE',  ( 103.1528011352953342, 80.31250000136559208, -3.152801135295383084 ) ) ;
#26319 = CARTESIAN_POINT ( 'NONE',  ( 65.00000000000000000, 34.99726562608393721, -13.14518615778179544 ) ) ;
#26320 = CARTESIAN_POINT ( 'NONE',  ( 93.46109445667491400, 105.2492070361643215, -45.17500000273119554 ) ) ;
#26321 = CARTESIAN_POINT ( 'NONE',  ( -9.295050272127046043, 38.07304687608393579, -9.295050272127046043 ) ) ;
#26322 = AXIS2_PLACEMENT_3D ( 'NONE', #18542, #7411, #16105 ) ;
#26323 = DIRECTION ( 'NONE',  ( 0.000000000000000000, 0.000000000000000000, -1.000000000000000000 ) ) ;
#26324 = CARTESIAN_POINT ( 'NONE',  ( 195.0000000000000000, -7.395377635281828788, -2.255140518769849538E-14 ) ) ;
#26325 = CARTESIAN_POINT ( 'NONE',  ( 102.1631189606246153, 116.6573956140660897, -55.09999999453764019 ) ) ;
#26326 = CARTESIAN_POINT ( 'NONE',  ( 116.4251840539369596, 38.66835937499999432, 5.622872871577880183 ) ) ;
#26327 = VERTEX_POINT ( 'NONE', #11445 ) ;
#26328 = CARTESIAN_POINT ( 'NONE',  ( 99.99999999999998579, 124.0000000000000000, -2.499999999999997780 ) ) ;
#26329 = CARTESIAN_POINT ( 'NONE',  ( 13.14518615778179544, 37.97382812608393721, -1.609821015232357215E-15 ) ) ;
#26330 = CARTESIAN_POINT ( 'NONE',  ( 9.598844408820456309, 36.03906250216787299, -9.598844408820458085 ) ) ;
#26331 = CARTESIAN_POINT ( 'NONE',  ( 116.8548138422182063, 37.42812500108393436, 5.444914386472304635 ) ) ;
#26332 = CARTESIAN_POINT ( 'NONE',  ( 74.59884440882045453, 34.25312500216787015, 9.598844408820456309 ) ) ;
#26333 = ORIENTED_EDGE ( 'NONE', *, *, #14339, .F. ) ;
#26334 = EDGE_CURVE ( 'NONE', #11263, #8015, #2247, .T. ) ;
#26335 = CARTESIAN_POINT ( 'NONE',  ( 104.9999999999999716, 83.50000000000000000, -1.449011120738813565E-14 ) ) ;
#26336 = CARTESIAN_POINT ( 'NONE',  ( -13.57481594606304576, 34.00507812716787015, 5.622872871577880183 ) ) ;
#26337 = AXIS2_PLACEMENT_3D ( 'NONE', #3326, #1063, #7053 ) ;
#26338 = VECTOR ( 'NONE', #19247, 1000.000000000000000 ) ;
#26339 = CARTESIAN_POINT ( 'NONE',  ( 96.46446609406721961, -3.535533905932727539, 2.124999999999998224 ) ) ;
#26340 = CARTESIAN_POINT ( 'NONE',  ( 94.99999999999995737, 85.00000000000000000, -1.387778780781445676E-14 ) ) ;
#26341 = AXIS2_PLACEMENT_3D ( 'NONE', #5977, #6621, #15594 ) ;
#26342 = CARTESIAN_POINT ( 'NONE',  ( 200.4449143864723055, 35.54296875108393294, -13.14518615778179900 ) ) ;
#26343 = DIRECTION ( 'NONE',  ( 0.000000000000000000, -1.000000000000000000, 0.000000000000000000 ) ) ;
#26344 = PLANE ( 'NONE',  #7759 ) ;
#26345 = CARTESIAN_POINT ( 'NONE',  ( 195.0000000000000000, 39.21406249999999716, -13.57481594606304576 ) ) ;
#26346 = CARTESIAN_POINT ( 'NONE',  ( 99.99999999999998579, 130.0000000000000000, -5.204170427930421283E-15 ) ) ;
#26347 = CARTESIAN_POINT ( 'NONE',  ( 200.6228728715780107, 36.78320312499999289, -13.57481594606290898 ) ) ;
#26348 = CARTESIAN_POINT ( 'NONE',  ( -8.312177448680279460E-16, 38.42031249999999432, -13.57481594606304576 ) ) ;
#26349 = CARTESIAN_POINT ( 'NONE',  ( -1.271138771240642784, 36.00000000000000000, -13.43002483374384681 ) ) ;
#26350 = CARTESIAN_POINT ( 'NONE',  ( -5.444914386472297529, 39.01562500108394005, -13.14518615778179900 ) ) ;
#26351 = CARTESIAN_POINT ( 'NONE',  ( -13.14518615778179544, 37.37851562608393863, 0.000000000000000000 ) ) ;
#26352 = CARTESIAN_POINT ( 'NONE',  ( 208.5748159460630688, 34.25312499999999716, -1.662435489736055892E-15 ) ) ;
#26353 = CONTEXT_DEPENDENT_SHAPE_REPRESENTATION ( #16978, #3493 ) ;
#26354 = CARTESIAN_POINT ( 'NONE',  ( 99.99999999999995737, 81.87500000273119838, -5.000000000000018652 ) ) ;
#26355 = CARTESIAN_POINT ( 'NONE',  ( 104.4587341249999781, 95.56249999863440792, -6.938893903907228378E-15 ) ) ;
#26356 = CARTESIAN_POINT ( 'NONE',  ( 70.44491438647230552, 35.24531250108393010, 13.14518615778179189 ) ) ;
#26357 = CARTESIAN_POINT ( 'NONE',  ( 99.99999999999995737, 4.458734125000016313, 1.187500001365592750 ) ) ;
#26358 = CARTESIAN_POINT ( 'NONE',  ( 99.95774716806533888, 123.0000000000000426, 2.503702194450118323 ) ) ;
#26359 = VERTEX_POINT ( 'NONE', #18017 ) ;
#26360 = CARTESIAN_POINT ( 'NONE',  ( 97.92893218813451028, 5.000000000000018652, 4.812500000000000000 ) ) ;
#26361 = CARTESIAN_POINT ( 'NONE',  ( -9.598844408820454532, 37.13046874999999147, 9.598844408820459861 ) ) ;
#26362 = CARTESIAN_POINT ( 'NONE',  ( 135.4449143864723055, 36.23750000108393721, 13.14518615778179189 ) ) ;
#26363 = VERTEX_POINT ( 'NONE', #14010 ) ;
#26364 = CARTESIAN_POINT ( 'NONE',  ( 103.5355339059327093, 84.37500000000000000, 3.535533905932726206 ) ) ;
#26365 = CARTESIAN_POINT ( 'NONE',  ( 96.46446609406721961, 83.00000000273119838, -3.535533905932755072 ) ) ;
#26366 = CARTESIAN_POINT ( 'NONE',  ( 101.8468681455907330, 92.12499999863437949, 4.458734124999979898 ) ) ;
#26367 = AXIS2_PLACEMENT_3D ( 'NONE', #742, #24387, #13540 ) ;
#26368 = CARTESIAN_POINT ( 'NONE',  ( 51.82584278307725612, 36.00000000000001421, 0.03826467346021202032 ) ) ;
#26369 = CARTESIAN_POINT ( 'NONE',  ( 104.3262379212492448, 104.0454443415356991, -48.30000000000001137 ) ) ;
#26370 = CARTESIAN_POINT ( 'NONE',  ( 78.14518615778179367, 33.26093750108393721, -5.444914386472297529 ) ) ;
#26371 = ADVANCED_BREP_SHAPE_REPRESENTATION ( '', ( #26591, #26844 ), #20877 ) ;
#26372 = ORIENTED_EDGE ( 'NONE', *, *, #2185, .F. ) ;
#26373 = EDGE_CURVE ( 'NONE', #6096, #15330, #24964, .T. ) ;
#26374 = CARTESIAN_POINT ( 'NONE',  ( 130.0000000000000000, 38.91640625216786731, 13.57481594606304576 ) ) ;
#26375 = CARTESIAN_POINT ( 'NONE',  ( 104.9999999999999574, 2.071067811865491937, 13.56250000000000000 ) ) ;
#26376 = EDGE_CURVE ( 'NONE', #11554, #19382, #6969, .T. ) ;
#26377 = ORIENTED_EDGE ( 'NONE', *, *, #19400, .T. ) ;
#26378 = DIRECTION ( 'NONE',  ( -1.000000000000000000, -0.000000000000000000, -0.000000000000000000 ) ) ;
#26379 = CARTESIAN_POINT ( 'NONE',  ( 5.444914386472297529, 40.50390625108394005, -13.14518615778179900 ) ) ;
#26380 = CARTESIAN_POINT ( 'NONE',  ( 208.5748159460630120, 33.60820312716787583, -5.622872871577873077 ) ) ;
#26381 =( BOUNDED_CURVE ( )  B_SPLINE_CURVE ( 2, ( #3925, #3506, #21308, #12311, #23173, #12167, #27589, #1791, #10457 ),
 .UNSPECIFIED., .F., .F. ) 
 B_SPLINE_CURVE_WITH_KNOTS ( ( 3, 2, 2, 2, 3 ),
 ( 0.6071428571428570953, 0.6160714285714286031, 0.6250000000000000000, 0.6339285714285712858, 0.6428571428571427937 ),
 .UNSPECIFIED. ) 
 CURVE ( )  GEOMETRIC_REPRESENTATION_ITEM ( )  RATIONAL_B_SPLINE_CURVE ( ( 1.000000000000000000, 0.9238795325112867385, 1.000000000000000000, 0.9238795325112867385, 1.000000000000000000, 0.9238795325112867385, 1.000000000000000000, 0.9238795325112877377, 0.9999999999999990008 ) ) 
 REPRESENTATION_ITEM ( '' )  );
#26382 = CARTESIAN_POINT ( 'NONE',  ( -5.444914386472299306, 37.52734375108393294, 13.14518615778179722 ) ) ;
#26383 = CARTESIAN_POINT ( 'NONE',  ( 13.57481594606304931, 36.68398437716787441, 5.622872871577868636 ) ) ;
#26384 = CARTESIAN_POINT ( 'NONE',  ( 116.8548138422182205, 37.52734375108393294, -5.444914386472297529 ) ) ;
#26385 = CARTESIAN_POINT ( 'NONE',  ( -13.14518615778179189, 35.24531250108393721, 5.444914386472304635 ) ) ;
#26386 = COLOUR_RGB ( '', 0.66274510, 0.83137255, 0.94901961) ;
#26387 = CARTESIAN_POINT ( 'NONE',  ( 139.2950502721270425, 36.08867187608392868, 9.295050272127046043 ) ) ;
#26388 = CARTESIAN_POINT ( 'NONE',  ( 78.57481594606304043, 34.20351562499999432, 5.622872871577869525 ) ) ;
#26389 = CARTESIAN_POINT ( 'NONE',  ( 102.0669872999999939, 124.4000000010924651, -0.8561741729129507261 ) ) ;
#26390 = VECTOR ( 'NONE', #22803, 1000.000000000000000 ) ;
#26391 = EDGE_CURVE ( 'NONE', #10301, #9895, #15407, .T. ) ;
#26392 = CARTESIAN_POINT ( 'NONE',  ( 103.1528011352953342, 3.152801135295383084, 10.31250000136559208 ) ) ;
#26393 = CARTESIAN_POINT ( 'NONE',  ( 130.0000000000000000, 36.03906250000000000, -13.57481594606304576 ) ) ;
#26394 = CARTESIAN_POINT ( 'NONE',  ( 98.15313185440923860, -4.458734124999987891, 12.62500000136559208 ) ) ;
#26395 = CARTESIAN_POINT ( 'NONE',  ( 108.0825317500000011, 107.3738262389971538, -44.22500000273118559 ) ) ;
#26396 = DIRECTION ( 'NONE',  ( 0.000000000000000000, -1.000000000000000000, 0.000000000000000000 ) ) ;
#26397 = CARTESIAN_POINT ( 'NONE',  ( 91.91746824999997045, 107.3738262389971680, -49.52499999726881441 ) ) ;
#26398 = CARTESIAN_POINT ( 'NONE',  ( -13.14518615778179900, 37.52734375108393294, -5.444914386472297529 ) ) ;
#26399 = CARTESIAN_POINT ( 'NONE',  ( 95.00472066334982912, 103.1245878333314323, -53.57499999726881157 ) ) ;
#26400 = ORIENTED_EDGE ( 'NONE', *, *, #3840, .T. ) ;
#26401 = CARTESIAN_POINT ( 'NONE',  ( 93.00000000000000000, 110.0000000000000000, -46.50000000546238255 ) ) ;
#26402 = DIRECTION ( 'NONE',  ( 0.000000000000000000, 0.000000000000000000, -1.000000000000000000 ) ) ;
#26403 = DIRECTION ( 'NONE',  ( 5.782411586589357392E-17, -0.000000000000000000, 1.000000000000000000 ) ) ;
#26404 = CARTESIAN_POINT ( 'NONE',  ( 200.4449143864723055, 38.42031250108393436, 13.14518615778179189 ) ) ;
#26405 = ORIENTED_EDGE ( 'NONE', *, *, #4266, .F. ) ;
#26406 = ADVANCED_FACE ( 'NONE', ( #19284 ), #41, .T. ) ;
#26407 = DIRECTION ( 'NONE',  ( 5.782411586589357392E-17, -0.000000000000000000, 1.000000000000000000 ) ) ;
#26408 = CARTESIAN_POINT ( 'NONE',  ( 96.84719886470459471, 3.152801135295383084, 13.56250000136559386 ) ) ;
#26409 = CIRCLE ( 'NONE', #12282, 11.57481594606304398 ) ;
#26410 = VERTEX_POINT ( 'NONE', #19697 ) ;
#26411 = CARTESIAN_POINT ( 'NONE',  ( 91.91746824999998466, 107.3738262389971538, -51.27500000273119696 ) ) ;
#26412 = CARTESIAN_POINT ( 'NONE',  ( -9.295050272127044266, 39.06523437608392868, 9.295050272127047819 ) ) ;
#26413 = CARTESIAN_POINT ( 'NONE',  ( 102.4999999999999716, 123.0500000000000114, -1.035533905932742638 ) ) ;
#26414 = EDGE_CURVE ( 'NONE', #19519, #21081, #11125, .T. ) ;
#26415 = CARTESIAN_POINT ( 'NONE',  ( 120.7049497278729575, 39.85898437608393152, 9.295050272127047819 ) ) ;
#26416 = CARTESIAN_POINT ( 'NONE',  ( 5.444914386472297529, 40.50390625108394005, -13.14518615778179722 ) ) ;
#26417 = CARTESIAN_POINT ( 'NONE',  ( 104.9999999999999716, 93.93749999726881583, -2.071067811865478170 ) ) ;
#26418 = CARTESIAN_POINT ( 'NONE',  ( 59.55508561352770158, 39.01562500108394005, -13.14518615778179900 ) ) ;
#26419 = CARTESIAN_POINT ( 'NONE',  ( 61.95539054307062088, 53.89089363584123760, -15.00000000000000000 ) ) ;
#26420 = CARTESIAN_POINT ( 'NONE',  ( 204.5988444088204687, 40.50390624999999289, 9.598844408820456309 ) ) ;
#26421 = ADVANCED_FACE ( 'NONE', ( #19417 ), #12840, .F. ) ;
#26422 =( BOUNDED_CURVE ( )  B_SPLINE_CURVE ( 2, ( #18257, #17683, #22536, #21971, #24527, #5012, #11109, #24242, #19823 ),
 .UNSPECIFIED., .F., .F. ) 
 B_SPLINE_CURVE_WITH_KNOTS ( ( 3, 2, 2, 2, 3 ),
 ( 0.6458333333333333703, 0.6562500000000000000, 0.6666666666666665186, 0.6770833333333332593, 0.6874999999999997780 ),
 .UNSPECIFIED. ) 
 CURVE ( )  GEOMETRIC_REPRESENTATION_ITEM ( )  RATIONAL_B_SPLINE_CURVE ( ( 1.000000000000000000, 0.9238795325112867385, 1.000000000000000000, 0.9238795325112867385, 1.000000000000000000, 0.9238795325112867385, 1.000000000000000000, 0.9238795325112884038, 0.9999999999999983347 ) ) 
 REPRESENTATION_ITEM ( '' )  );
#26423 = VERTEX_POINT ( 'NONE', #26115 ) ;
#26424 = ORIENTED_EDGE ( 'NONE', *, *, #24827, .T. ) ;
#26425 = CARTESIAN_POINT ( 'NONE',  ( 5.444914386472297529, 38.91640625108393436, -13.14518615778179900 ) ) ;
#26426 = CARTESIAN_POINT ( 'NONE',  ( 96.84719886470459471, 3.152801135295383084, 11.56250000136559208 ) ) ;
#26427 = CARTESIAN_POINT ( 'NONE',  ( 51.85481384221820633, 40.50390625108394005, -5.444914386472297529 ) ) ;
#26428 = CARTESIAN_POINT ( 'NONE',  ( 103.1528011352953342, 82.06250000136559208, -3.152801135295383084 ) ) ;
#26429 = CARTESIAN_POINT ( 'NONE',  ( 208.1451861577818079, 40.15664062608393436, -1.609821015232357215E-15 ) ) ;
#26430 = CIRCLE ( 'NONE', #20061, 13.57481594606304576 ) ;
#26431 = CARTESIAN_POINT ( 'NONE',  ( 9.295050272127046043, 38.07304687608393579, -9.295050272127046043 ) ) ;
#26432 = CARTESIAN_POINT ( 'NONE',  ( 96.84719886470463734, 91.18749999863440792, 3.152801135295351997 ) ) ;
#26433 = CARTESIAN_POINT ( 'NONE',  ( 185.7049497278729575, 38.46992187608393721, 9.295050272127047819 ) ) ;
#26434 = CARTESIAN_POINT ( 'NONE',  ( 108.0825317499999869, 112.6261737610028320, -54.52499999726880731 ) ) ;
#26435 = EDGE_LOOP ( 'NONE', ( #21669, #8583, #22378, #14082 ) ) ;
#26436 = CARTESIAN_POINT ( 'NONE',  ( 9.598844408820456309, 35.93984374999999432, -9.598844408820458085 ) ) ;
#26437 = CARTESIAN_POINT ( 'NONE',  ( -8.049105076161786076E-16, 37.18007812608393436, -13.14518615778179544 ) ) ;
#26438 = VERTEX_POINT ( 'NONE', #4595 ) ;
#26439 = CARTESIAN_POINT ( 'NONE',  ( 143.1451861577818079, 32.41757812608393863, -1.609821015232357215E-15 ) ) ;
#26440 = CARTESIAN_POINT ( 'NONE',  ( 55.70494972787295751, 34.30273437608393294, 9.295050272127047819 ) ) ;
#26441 = CARTESIAN_POINT ( 'NONE',  ( 200.4449143864723055, 38.61875000108393152, 13.14518615778179189 ) ) ;
#26442 = ORIENTED_EDGE ( 'NONE', *, *, #9550, .T. ) ;
#26443 = CARTESIAN_POINT ( 'NONE',  ( 99.99999999999995737, 1.387778780781445676E-14, 34.79898987322334136 ) ) ;
#26444 = CARTESIAN_POINT ( 'NONE',  ( 2.414731522848535132E-15, 32.02070312608393010, 13.14518615778179544 ) ) ;
#26445 = CARTESIAN_POINT ( 'NONE',  ( 102.0710678118654329, -4.999999999999989342, 1.437500002731185056 ) ) ;
#26446 = EDGE_CURVE ( 'NONE', #26438, #25528, #10200, .T. ) ;
#26447 = VECTOR ( 'NONE', #9092, 999.9999999999998863 ) ;
#26448 = CARTESIAN_POINT ( 'NONE',  ( 65.00000000000000000, 40.80156249999999574, -13.57481594606304576 ) ) ;
#26449 = CARTESIAN_POINT ( 'NONE',  ( 108.0825317500000011, 112.6261737610028320, -54.02500000273118985 ) ) ;
#26450 = CARTESIAN_POINT ( 'NONE',  ( 104.9999999999999574, 2.071067811865501263, 10.56249999999999645 ) ) ;
#26451 = CARTESIAN_POINT ( 'NONE',  ( 98.23223304703363112, 124.2000000021849502, -1.767766952966370209 ) ) ;
#26452 = CARTESIAN_POINT ( 'NONE',  ( 98.96446609406726225, 124.0499999999999829, -2.499999999999998668 ) ) ;
#26453 = VECTOR ( 'NONE', #27686, 1000.000000000000000 ) ;
#26454 = ORIENTED_EDGE ( 'NONE', *, *, #26275, .T. ) ;
#26455 = SHAPE_REPRESENTATION_RELATIONSHIP ( 'NONE' , 'NONE' ,  #14045, #2892 ) ;
#26456 = EDGE_LOOP ( 'NONE', ( #23335, #6910, #20724, #26311 ) ) ;
#26457 = CARTESIAN_POINT ( 'NONE',  ( 101.8468681455906903, 4.458734125000016313, 4.125000001365592084 ) ) ;
#26458 = ORIENTED_EDGE ( 'NONE', *, *, #7139, .F. ) ;
#26459 = CARTESIAN_POINT ( 'NONE',  ( 99.14382582708707048, 123.6000000010924680, -2.066987299999999195 ) ) ;
#26460 = CARTESIAN_POINT ( 'NONE',  ( 98.15313185440925281, 4.458734125000016313, 7.250000001365591196 ) ) ;
#26461 = CARTESIAN_POINT ( 'NONE',  ( 69.15728635496172672, 36.00000000000000000, -12.92256159328856135 ) ) ;
#26462 = CARTESIAN_POINT ( 'NONE',  ( 9.295050272127046043, 34.69960937608393436, -9.295050272127046043 ) ) ;
#26463 = FACE_BOUND ( 'NONE', #25570, .T. ) ;
#26464 = CARTESIAN_POINT ( 'NONE',  ( 99.99999999999995737, 82.93750000136560629, 4.458734124999988779 ) ) ;
#26465 = CARTESIAN_POINT ( 'NONE',  ( 78.14518615778179367, 36.33671875108394289, 5.444914386472293977 ) ) ;
#26466 = CARTESIAN_POINT ( 'NONE',  ( 104.9952793366501851, 116.8754121666685393, -51.82500000273120122 ) ) ;
#26467 = CARTESIAN_POINT ( 'NONE',  ( -5.444914386472299306, 39.11484375108393863, 13.14518615778179722 ) ) ;
#26468 = DIRECTION ( 'NONE',  ( -0.000000000000000000, -1.000000000000000000, -0.000000000000000000 ) ) ;
#26469 = CARTESIAN_POINT ( 'NONE',  ( 0.000000000000000000, 40.99999999999999289, 0.000000000000000000 ) ) ;
#26470 = LINE ( 'NONE', #242, #14232 ) ;
#26471 = CARTESIAN_POINT ( 'NONE',  ( 143.5748159460630404, 37.47773437500001137, -5.622872871577873077 ) ) ;
#26472 = ORIENTED_EDGE ( 'NONE', *, *, #8793, .F. ) ;
#26473 = ORIENTED_EDGE ( 'NONE', *, *, #27991, .T. ) ;
#26474 = CARTESIAN_POINT ( 'NONE',  ( -9.598844408820458085, 40.20625000216787726, -9.598844408820458085 ) ) ;
#26475 = CARTESIAN_POINT ( 'NONE',  ( 13.14518615778179900, 36.33671875108394289, 5.444914386472293977 ) ) ;
#26476 = CARTESIAN_POINT ( 'NONE',  ( 13.57481594606304753, 36.78320312716786589, -5.622872871577873077 ) ) ;
#26477 = CARTESIAN_POINT ( 'NONE',  ( 99.99999999999995737, 5.000000000000018652, 8.875000002731184168 ) ) ;
#26478 = CARTESIAN_POINT ( 'NONE',  ( 135.4449143864723055, 33.16171875108393152, -13.14518615778179900 ) ) ;
#26479 = CARTESIAN_POINT ( 'NONE',  ( 70.62287287157786864, 32.91367187716787157, -13.57481594606304753 ) ) ;
#26480 = VERTEX_POINT ( 'NONE', #9012 ) ;
#26481 = DIRECTION ( 'NONE',  ( -0.000000000000000000, -1.000000000000000000, -0.000000000000000000 ) ) ;
#26482 = CARTESIAN_POINT ( 'NONE',  ( 5.622872871577878406, 33.40976562716787157, 13.57481594606304576 ) ) ;
#26483 = CARTESIAN_POINT ( 'NONE',  ( 59.37712712842203189, 37.97382812499999716, 13.57481594606295161 ) ) ;
#26484 = CARTESIAN_POINT ( 'NONE',  ( 95.00472066334981491, 103.1245878333314465, -47.57499999726882578 ) ) ;
#26485 = CARTESIAN_POINT ( 'NONE',  ( 13.57481594606304576, 38.32109375216786873, -1.662435489736055892E-15 ) ) ;
#26486 = CARTESIAN_POINT ( 'NONE',  ( 208.1451861577817795, 33.75703125108393010, 5.444914386472293977 ) ) ;
#26487 = FACE_OUTER_BOUND ( 'NONE', #1222, .T. ) ;
#26488 = CARTESIAN_POINT ( 'NONE',  ( 131.1371678245417627, 36.00000000000000000, 13.09590655363595602 ) ) ;
#26489 = CARTESIAN_POINT ( 'NONE',  ( 208.5748159460630688, 39.01562500000000000, -1.662435489736055892E-15 ) ) ;
#26490 = CARTESIAN_POINT ( 'NONE',  ( 99.99999999999995737, -4.999999999999990230, 10.37500000273118594 ) ) ;
#26491 = CARTESIAN_POINT ( 'NONE',  ( 138.3922152916384221, 55.00000000000001421, 14.99999999999997158 ) ) ;
#26492 = CARTESIAN_POINT ( 'NONE',  ( -13.57481594606304576, 38.66835937499999432, 5.622872871577880183 ) ) ;
#26493 = LINE ( 'NONE', #20077, #16170 ) ;
#26494 = CARTESIAN_POINT ( 'NONE',  ( 5.444914386472297529, 38.91640625108393436, -13.14518615778179900 ) ) ;
#26495 = CARTESIAN_POINT ( 'NONE',  ( -9.295050272127046043, 37.27929687608393294, -9.295050272127046043 ) ) ;
#26496 = CARTESIAN_POINT ( 'NONE',  ( 185.4011555911795313, 35.34453124999998863, -9.598844408820458085 ) ) ;
#26497 = CARTESIAN_POINT ( 'NONE',  ( -8.312177448680279460E-16, 36.13828125216787157, -13.57481594606304576 ) ) ;
#26498 = CARTESIAN_POINT ( 'NONE',  ( 98.15313185440925281, -4.458734124999987891, 0.8750000013655926390 ) ) ;
#26499 = CARTESIAN_POINT ( 'NONE',  ( 65.00000000000000000, 34.79882812608393294, -13.14518615778179544 ) ) ;
#26500 = EDGE_CURVE ( 'NONE', #21442, #21964, #11280, .T. ) ;
#26501 = CARTESIAN_POINT ( 'NONE',  ( 98.15313185440923860, -4.458734124999987891, 1.625000001365591862 ) ) ;
#26502 = CARTESIAN_POINT ( 'NONE',  ( 100.7645585624018025, 123.0000000000000426, -2.384778589250489578 ) ) ;
#26503 = VERTEX_POINT ( 'NONE', #13114 ) ;
#26504 = DIRECTION ( 'NONE',  ( 0.000000000000000000, 0.8660254037844380415, 0.5000000000000009992 ) ) ;
#26505 = CARTESIAN_POINT ( 'NONE',  ( -5.622872871577873077, 36.88242187499999858, -13.57481594606304753 ) ) ;
#26506 = CARTESIAN_POINT ( 'NONE',  ( 116.8548138422182063, 38.42031250108393436, 5.444914386472304635 ) ) ;
#26507 = EDGE_LOOP ( 'NONE', ( #22240, #11741, #12149, #14304 ) ) ;
#26508 = CARTESIAN_POINT ( 'NONE',  ( 99.99999999999995737, 81.75000000000000000, -5.000000000000018652 ) ) ;
#26509 = DIRECTION ( 'NONE',  ( 0.000000000000000000, 0.000000000000000000, 1.000000000000000000 ) ) ;
#26510 = CARTESIAN_POINT ( 'NONE',  ( 99.99999999999995737, 80.87500000273119838, -5.000000000000018652 ) ) ;
#26511 = CARTESIAN_POINT ( 'NONE',  ( 101.8468681455907330, 92.49999999863442213, -4.458734124999994997 ) ) ;
#26512 = CARTESIAN_POINT ( 'NONE',  ( 101.8468681455907330, 95.37499999863440792, 4.458734124999979898 ) ) ;
#26513 = CARTESIAN_POINT ( 'NONE',  ( 99.99999999999997158, 117.3602355696678501, -47.50000000000001421 ) ) ;
#26514 = CARTESIAN_POINT ( 'NONE',  ( 51.85481384221819923, 31.97109375108393436, -5.444914386472297529 ) ) ;
#26515 = ORIENTED_EDGE ( 'NONE', *, *, #14922, .T. ) ;
#26516 = FACE_OUTER_BOUND ( 'NONE', #2566, .T. ) ;
#26517 = AXIS2_PLACEMENT_3D ( 'NONE', #22458, #19885, #22172 ) ;
#26518 = CARTESIAN_POINT ( 'NONE',  ( 94.99999999999995737, -2.071067811865466624, 12.06250000000000000 ) ) ;
#26519 = ORIENTED_EDGE ( 'NONE', *, *, #24830, .T. ) ;
#26520 = CARTESIAN_POINT ( 'NONE',  ( 13.14518615778179544, 35.59257812608393579, -1.609821015232357215E-15 ) ) ;
#26521 = CARTESIAN_POINT ( 'NONE',  ( 195.0000000000000000, 33.75703125216787726, -13.57481594606304576 ) ) ;
#26522 = ORIENTED_EDGE ( 'NONE', *, *, #21332, .F. ) ;
#26523 = CARTESIAN_POINT ( 'NONE',  ( 5.444914386472302859, 32.86406250108392868, 13.14518615778179189 ) ) ;
#26524 = CARTESIAN_POINT ( 'NONE',  ( -8.312177448680279460E-16, 36.93203125216787441, -13.57481594606304576 ) ) ;
#26525 = CARTESIAN_POINT ( 'NONE',  ( 135.4449143864723339, 36.23750000108393721, 13.14518615778179189 ) ) ;
#26526 = ORIENTED_EDGE ( 'NONE', *, *, #11191, .F. ) ;
#26527 = CARTESIAN_POINT ( 'NONE',  ( 2.414731522848535132E-15, 33.80664062608393294, 13.14518615778179544 ) ) ;
#26528 = CARTESIAN_POINT ( 'NONE',  ( 97.83688103937537051, 103.3426043859339103, -50.10000000546237686 ) ) ;
#26529 = CARTESIAN_POINT ( 'NONE',  ( 51.42518405393695957, 35.44374999999999432, 0.000000000000000000 ) ) ;
#26530 = CARTESIAN_POINT ( 'NONE',  ( 101.4615807364564546, 124.2500000010924737, 1.461580736456455476 ) ) ;
#26531 = CARTESIAN_POINT ( 'NONE',  ( 95.54126587499995082, -1.846868145590724986, 9.750000001365593860 ) ) ;
#26532 = CARTESIAN_POINT ( 'NONE',  ( 207.5314254911195349, 35.99999999999997868, -5.200562670744174554 ) ) ;
#26533 = CARTESIAN_POINT ( 'NONE',  ( 98.15313185440925281, -4.458734124999987891, 1.625000001365591640 ) ) ;
#26534 = CARTESIAN_POINT ( 'NONE',  ( 93.46109445667491400, 114.7507929638356785, -45.32500000273119412 ) ) ;
#26535 = CARTESIAN_POINT ( 'NONE',  ( 195.0000000000000000, -7.395377635281828788, -2.255140518769849538E-14 ) ) ;
#26536 = DIRECTION ( 'NONE',  ( 0.000000000000000000, 0.000000000000000000, 1.000000000000000000 ) ) ;
#26537 = CARTESIAN_POINT ( 'NONE',  ( 99.99999999999997158, 101.5015231886685712, -47.12499999726882294 ) ) ;
#26538 = CARTESIAN_POINT ( 'NONE',  ( -9.295050272127044266, 36.08867187608393579, 9.295050272127047819 ) ) ;
#26539 = CIRCLE ( 'NONE', #5593, 11.57481594606304398 ) ;
#26540 = CARTESIAN_POINT ( 'NONE',  ( 91.91746824999997045, 107.3738262389971538, -55.77499999726882862 ) ) ;
#26541 = ORIENTED_EDGE ( 'NONE', *, *, #18597, .T. ) ;
#26542 = CARTESIAN_POINT ( 'NONE',  ( 102.0669873000000081, 123.5000000010924737, 0.8561741729129311862 ) ) ;
#26543 =( BOUNDED_SURFACE ( )  B_SPLINE_SURFACE ( 1, 2, ( 
 ( #27695, #4309, #21420, #1479, #28111, #8157, #6028, #10135, #4170, #23553, #4030, #21274, #6163, #6439, #10700, #21557, #12695, #18847, #25411, #8575, #14563, #19406, #19273, #5893, #27972, #23278, #18985, #3751, #23693, #14974, #19129, #27836, #16849, #12413, #21133, #1618, #3886, #17265, #15108, #1757, #10276, #23829, #25548, #14692, #23412, #1898, #12547, #10564, #8430, #8290, #17119, #16982, #25823, #6297, #19831, #19551, #11261, #21699, #23971, #316, #4879, #8857, #5021, #2174, #9003, #26398, #19688, #21843, #13543, #601, #4587, #11404, #17695, #22121, #15253, #8714, #9280, #6853, #22265, #2319, #20123, #175, #24110, #6571, #2739, #4450, #17977, #15542, #24250, #15689, #2600, #26686, #10836, #459, #26538, #17406, #7133, #6995, #32, #13393, #21979, #13104, #10976, #4733, #19981, #26106, #17548, #15830, #2455, #24536, #13247, #9141, #26251, #6711, #15398, #11117, #17834, #24391, #7419, #25237, #22403, #5160, #22692, #20260, #5303, #16547, #746, #22547, #3439, #13686, #15969, #18551, #7852, #27116, #12106, #11832, #9565, #895, #13967, #20696, #11543, #9419, #27255, #2872, #20556, #1179, #18409, #3162, #3016, #1037, #14254, #7714, #11685, #14113, #22837, #9708, #7566, #16406, #16260, #25103, #24960, #20409, #3303, #5446, #18690, #11973, #18268, #1309, #26974, #5589, #18118, #24683, #20832, #9980, #9845, #27393, #16114, #26833, #7278, #22975, #13823, #24819, #14533 ),
 ( #14394, #12661, #10530, #1453, #4135, #19236, #12242, #25647, #5996, #18822, #16684, #19095, #27803, #20970, #7985, #12798, #14661, #25788, #16821, #6131, #25383, #5727, #27663, #27529, #10108, #25517, #1725, #21519, #23382, #23247, #3854, #8259, #5862, #27937, #8541, #12515, #3724, #17227, #14796, #23110, #1998, #12386, #10246, #3584, #8396, #16946, #23520, #21244, #10387, #10665, #6265, #17085, #3998, #21104, #1592, #19373, #18955, #21388, #8125, #1865, #14938, #23660, #28077, #2667, #24075, #9107, #13069, #9249, #6407, #4553, #2425, #23935, #26069, #17801, #4844, #8822, #15655, #13213, #26361, #19516, #12930, #13507, #21947, #26505, #6538, #24355, #4415, #136, #10803, #6961, #8683, #22228, #11085, #19795, #19942, #6819, #2707, #15076, #4698, #2563, #21662, #11367, #11226, #4271, #17653, #26213, #17373, #15216, #279, #8965, #2139, #21806, #20089, #6674, #567, #17512, #15509, #2284, #25932, #19654, #10942, #15361, #24219, #13359, #23794, #22086, #421, #16076, #20518, #18081, #3268, #20796, #24784, #15932, #1276, #9669, #17941, #16367, #24649, #22510, #26651, #20658, #3129, #1000, #9531, #13931, #14220, #18516, #1143, #11795, #7099, #15797, #25068, #2840, #27221, #7529, #4987, #16225, #11508, #7240, #13652, #11936, #9810, #7383, #5265, #5122, #24500, #709, #9384, #20374, #7675, #5555, #18229, #22367, #3401, #22938, #12071, #2976, #18372, #26794, #22658, #27077, #13789 ) ),
 .UNSPECIFIED., .F., .F., .F. ) 
 B_SPLINE_SURFACE_WITH_KNOTS ( ( 2, 2 ),
 ( 3, 2, 2, 2, 2, 2, 2, 2, 2, 2, 2, 2, 2, 2, 2, 2, 2, 2, 2, 2, 2, 2, 2, 2, 2, 2, 2, 2, 2, 2, 2, 2, 2, 2, 2, 2, 2, 2, 2, 2, 2, 2, 2, 2, 2, 2, 2, 2, 2, 2, 2, 2, 2, 2, 2, 2, 2, 2, 2, 2, 2, 2, 2, 2, 2, 2, 2, 2, 2, 2, 2, 2, 2, 2, 2, 2, 2, 2, 2, 2, 2, 2, 2, 2, 2, 2, 2, 2, 2, 2, 2, 3 ),
 ( 0.000000000000000000, 1.000000000000000000 ),
 ( 0.000000000000000000, 0.01041666666666666609, 0.02083333333333333218, 0.03125000000000000000, 0.04166666666666666435, 0.05208333333333333565, 0.06250000000000000000, 0.07291666666666667129, 0.08333333333333332871, 0.09375000000000000000, 0.1041666666666666713, 0.1145833333333333287, 0.1250000000000000000, 0.1354166666666666574, 0.1458333333333333426, 0.1562500000000000000, 0.1666666666666666574, 0.1770833333333333426, 0.1875000000000000000, 0.1979166666666666574, 0.2083333333333333426, 0.2187500000000000000, 0.2291666666666666574, 0.2395833333333333426, 0.2500000000000000000, 0.2604166666666666852, 0.2708333333333333148, 0.2812500000000000000, 0.2916666666666666852, 0.3020833333333333148, 0.3125000000000000000, 0.3229166666666666852, 0.3333333333333333148, 0.3437500000000000000, 0.3541666666666666852, 0.3645833333333333148, 0.3750000000000000000, 0.3854166666666666852, 0.3958333333333333148, 0.4062500000000000000, 0.4166666666666666852, 0.4270833333333333148, 0.4375000000000000000, 0.4479166666666666852, 0.4583333333333333148, 0.4687500000000000000, 0.4791666666666666852, 0.4895833333333333148, 0.5000000000000000000, 0.5104166666666666297, 0.5208333333333333703, 0.5312500000000000000, 0.5416666666666666297, 0.5520833333333333703, 0.5625000000000000000, 0.5729166666666666297, 0.5833333333333333703, 0.5937500000000000000, 0.6041666666666666297, 0.6145833333333333703, 0.6250000000000000000, 0.6354166666666666297, 0.6458333333333333703, 0.6562500000000000000, 0.6666666666666666297, 0.6770833333333333703, 0.6875000000000000000, 0.6979166666666666297, 0.7083333333333333703, 0.7187500000000000000, 0.7291666666666666297, 0.7395833333333333703, 0.7500000000000000000, 0.7604166666666666297, 0.7708333333333333703, 0.7812500000000000000, 0.7916666666666666297, 0.8020833333333333703, 0.8125000000000000000, 0.8229166666666666297, 0.8333333333333333703, 0.8437500000000000000, 0.8541666666666666297, 0.8645833333333333703, 0.8750000000000000000, 0.8854166666666666297, 0.8958333333333333703, 0.9062500000000000000, 0.9166666666666666297, 0.9270833333333333703, 0.9375000000000000000, 0.9448586968893691873 ),
 .UNSPECIFIED. ) 
 GEOMETRIC_REPRESENTATION_ITEM ( )  RATIONAL_B_SPLINE_SURFACE ( (
 ( 1.000000000000000000, 0.9238795325112867385, 1.000000000000000000, 0.9238795325112867385, 1.000000000000000000, 0.9238795325112867385, 1.000000000000000000, 0.9238795325112867385, 1.000000000000000000, 0.9238795325112867385, 1.000000000000000000, 0.9238795325112867385, 1.000000000000000000, 0.9238795325112867385, 1.000000000000000000, 0.9238795325112867385, 1.000000000000000000, 0.9238795325112867385, 1.000000000000000000, 0.9238795325112867385, 1.000000000000000000, 0.9238795325112867385, 1.000000000000000000, 0.9238795325112867385, 1.000000000000000000, 0.9238795325112867385, 1.000000000000000000, 0.9238795325112867385, 1.000000000000000000, 0.9238795325112867385, 1.000000000000000000, 0.9238795325112867385, 1.000000000000000000, 0.9238795325112867385, 1.000000000000000000, 0.9238795325112867385, 1.000000000000000000, 0.9238795325112867385, 1.000000000000000000, 0.9238795325112867385, 1.000000000000000000, 0.9238795325112867385, 1.000000000000000000, 0.9238795325112867385, 1.000000000000000000, 0.9238795325112867385, 1.000000000000000000, 0.9238795325112867385, 1.000000000000000000, 0.9238795325112867385, 1.000000000000000000, 0.9238795325112867385, 1.000000000000000000, 0.9238795325112867385, 1.000000000000000000, 0.9238795325112867385, 1.000000000000000000, 0.9238795325112867385, 1.000000000000000000, 0.9238795325112867385, 1.000000000000000000, 0.9238795325112867385, 1.000000000000000000, 0.9238795325112867385, 1.000000000000000000, 0.9238795325112867385, 1.000000000000000000, 0.9238795325112867385, 1.000000000000000000, 0.9238795325112867385, 1.000000000000000000, 0.9238795325112867385, 1.000000000000000000, 0.9238795325112867385, 1.000000000000000000, 0.9238795325112867385, 1.000000000000000000, 0.9238795325112867385, 1.000000000000000000, 0.9238795325112867385, 1.000000000000000000, 0.9238795325112867385, 1.000000000000000000, 0.9238795325112867385, 1.000000000000000000, 0.9238795325112867385, 1.000000000000000000, 0.9238795325112867385, 1.000000000000000000, 0.9238795325112867385, 1.000000000000000000, 0.9238795325112867385, 1.000000000000000000, 0.9238795325112867385, 1.000000000000000000, 0.9238795325112867385, 1.000000000000000000, 0.9238795325112867385, 1.000000000000000000, 0.9238795325112867385, 1.000000000000000000, 0.9238795325112867385, 1.000000000000000000, 0.9238795325112867385, 1.000000000000000000, 0.9238795325112867385, 1.000000000000000000, 0.9238795325112867385, 1.000000000000000000, 0.9238795325112867385, 1.000000000000000000, 0.9238795325112867385, 1.000000000000000000, 0.9238795325112867385, 1.000000000000000000, 0.9238795325112867385, 1.000000000000000000, 0.9238795325112867385, 1.000000000000000000, 0.9238795325112867385, 1.000000000000000000, 0.9238795325112867385, 1.000000000000000000, 0.9238795325112867385, 1.000000000000000000, 0.9238795325112867385, 1.000000000000000000, 0.9238795325112867385, 1.000000000000000000, 0.9238795325112867385, 1.000000000000000000, 0.9238795325112867385, 1.000000000000000000, 0.9238795325112867385, 1.000000000000000000, 0.9238795325112867385, 1.000000000000000000, 0.9238795325112867385, 1.000000000000000000, 0.9238795325112867385, 1.000000000000000000, 0.9238795325112867385, 1.000000000000000000, 0.9238795325112867385, 1.000000000000000000, 0.9238795325112867385, 1.000000000000000000, 0.9238795325112867385, 1.000000000000000000, 0.9238795325112867385, 1.000000000000000000, 0.9238795325112867385, 1.000000000000000000, 0.9238795325112867385, 1.000000000000000000, 0.9238795325112867385, 1.000000000000000000, 0.9238795325112867385, 1.000000000000000000, 0.9238795325112867385, 1.000000000000000000, 0.9238795325112867385, 1.000000000000000000, 0.9238795325112867385, 1.000000000000000000, 0.9238795325112867385, 1.000000000000000000, 0.9238795325112867385, 1.000000000000000000, 0.9238795325112867385, 1.000000000000000000, 0.9238795325112867385, 1.000000000000000000, 0.9238795325112867385, 1.000000000000000000, 0.9238795325112867385, 1.000000000000000000, 0.9238795325112867385, 1.000000000000000000, 0.9238795325112867385, 1.000000000000000000, 0.9462258450566536361, 0.9684275698016389100),
 ( 1.000000000000000000, 0.9238795325112867385, 1.000000000000000000, 0.9238795325112867385, 1.000000000000000000, 0.9238795325112867385, 1.000000000000000000, 0.9238795325112867385, 1.000000000000000000, 0.9238795325112867385, 1.000000000000000000, 0.9238795325112867385, 1.000000000000000000, 0.9238795325112867385, 1.000000000000000000, 0.9238795325112867385, 1.000000000000000000, 0.9238795325112867385, 1.000000000000000000, 0.9238795325112867385, 1.000000000000000000, 0.9238795325112867385, 1.000000000000000000, 0.9238795325112867385, 1.000000000000000000, 0.9238795325112867385, 1.000000000000000000, 0.9238795325112867385, 1.000000000000000000, 0.9238795325112867385, 1.000000000000000000, 0.9238795325112867385, 1.000000000000000000, 0.9238795325112867385, 1.000000000000000000, 0.9238795325112867385, 1.000000000000000000, 0.9238795325112867385, 1.000000000000000000, 0.9238795325112867385, 1.000000000000000000, 0.9238795325112867385, 1.000000000000000000, 0.9238795325112867385, 1.000000000000000000, 0.9238795325112867385, 1.000000000000000000, 0.9238795325112867385, 1.000000000000000000, 0.9238795325112867385, 1.000000000000000000, 0.9238795325112867385, 1.000000000000000000, 0.9238795325112867385, 1.000000000000000000, 0.9238795325112867385, 1.000000000000000000, 0.9238795325112867385, 1.000000000000000000, 0.9238795325112867385, 1.000000000000000000, 0.9238795325112867385, 1.000000000000000000, 0.9238795325112867385, 1.000000000000000000, 0.9238795325112867385, 1.000000000000000000, 0.9238795325112867385, 1.000000000000000000, 0.9238795325112867385, 1.000000000000000000, 0.9238795325112867385, 1.000000000000000000, 0.9238795325112867385, 1.000000000000000000, 0.9238795325112867385, 1.000000000000000000, 0.9238795325112867385, 1.000000000000000000, 0.9238795325112867385, 1.000000000000000000, 0.9238795325112867385, 1.000000000000000000, 0.9238795325112867385, 1.000000000000000000, 0.9238795325112867385, 1.000000000000000000, 0.9238795325112867385, 1.000000000000000000, 0.9238795325112867385, 1.000000000000000000, 0.9238795325112867385, 1.000000000000000000, 0.9238795325112867385, 1.000000000000000000, 0.9238795325112867385, 1.000000000000000000, 0.9238795325112867385, 1.000000000000000000, 0.9238795325112867385, 1.000000000000000000, 0.9238795325112867385, 1.000000000000000000, 0.9238795325112867385, 1.000000000000000000, 0.9238795325112867385, 1.000000000000000000, 0.9238795325112867385, 1.000000000000000000, 0.9238795325112867385, 1.000000000000000000, 0.9238795325112867385, 1.000000000000000000, 0.9238795325112867385, 1.000000000000000000, 0.9238795325112867385, 1.000000000000000000, 0.9238795325112867385, 1.000000000000000000, 0.9238795325112867385, 1.000000000000000000, 0.9238795325112867385, 1.000000000000000000, 0.9238795325112867385, 1.000000000000000000, 0.9238795325112867385, 1.000000000000000000, 0.9238795325112867385, 1.000000000000000000, 0.9238795325112867385, 1.000000000000000000, 0.9238795325112867385, 1.000000000000000000, 0.9238795325112867385, 1.000000000000000000, 0.9238795325112867385, 1.000000000000000000, 0.9238795325112867385, 1.000000000000000000, 0.9238795325112867385, 1.000000000000000000, 0.9238795325112867385, 1.000000000000000000, 0.9238795325112867385, 1.000000000000000000, 0.9238795325112867385, 1.000000000000000000, 0.9238795325112867385, 1.000000000000000000, 0.9238795325112867385, 1.000000000000000000, 0.9238795325112867385, 1.000000000000000000, 0.9238795325112867385, 1.000000000000000000, 0.9238795325112867385, 1.000000000000000000, 0.9238795325112867385, 1.000000000000000000, 0.9238795325112867385, 1.000000000000000000, 0.9238795325112867385, 1.000000000000000000, 0.9238795325112867385, 1.000000000000000000, 0.9238795325112867385, 1.000000000000000000, 0.9238795325112867385, 1.000000000000000000, 0.9238795325112867385, 1.000000000000000000, 0.9238795325112867385, 1.000000000000000000, 0.9238795325112867385, 1.000000000000000000, 0.9238795325112867385, 1.000000000000000000, 0.9238795325112867385, 1.000000000000000000, 0.9238795325112867385, 1.000000000000000000, 0.9462258450566536361, 0.9684275698016389100) ) ) 
 REPRESENTATION_ITEM ( '' )  SURFACE ( )  );
#26544 = DIRECTION ( 'NONE',  ( 0.000000000000000000, -0.5735764363510443831, 0.8191520442889929088 ) ) ;
#26545 = DIRECTION ( 'NONE',  ( -0.000000000000000000, 1.000000000000000000, -0.000000000000000000 ) ) ;
#26546 = CARTESIAN_POINT ( 'NONE',  ( 208.1451861577817795, 35.44375000108393436, -5.444914386472297529 ) ) ;
#26547 = ORIENTED_EDGE ( 'NONE', *, *, #20938, .T. ) ;
#26548 = CARTESIAN_POINT ( 'NONE',  ( 102.1631189606246153, 116.6573956140660897, -49.09999999453764019 ) ) ;
#26549 = CARTESIAN_POINT ( 'NONE',  ( 96.84719886470459471, 3.152801135295383084, 9.562500001365593860 ) ) ;
#26550 = EDGE_LOOP ( 'NONE', ( #27174, #20415, #9886, #14458 ) ) ;
#26551 = CARTESIAN_POINT ( 'NONE',  ( 97.83688103937538472, 116.6573956140660897, -46.40000000000001279 ) ) ;
#26552 = CARTESIAN_POINT ( 'NONE',  ( 5.444914386472302859, 40.00781250108393294, 13.14518615778179189 ) ) ;
#26553 = CARTESIAN_POINT ( 'NONE',  ( 102.4999999999999858, 123.0000000000000000, -9.847140817659276890E-15 ) ) ;
#26554 = AXIS2_PLACEMENT_3D ( 'NONE', #23702, #24122, #23839 ) ;
#26555 = CARTESIAN_POINT ( 'NONE',  ( 116.8548138422182205, 39.75976562608393294, 0.000000000000000000 ) ) ;
#26556 = CARTESIAN_POINT ( 'NONE',  ( 5.444914386472302859, 39.41250000108393436, 13.14518615778179189 ) ) ;
#26557 = ADVANCED_FACE ( 'NONE', ( #12975 ), #25976, .T. ) ;
#26558 = ORIENTED_EDGE ( 'NONE', *, *, #26215, .F. ) ;
#26559 = CARTESIAN_POINT ( 'NONE',  ( 97.92893218813452449, 93.56249999726883004, 4.999999999999983125 ) ) ;
#26560 = CARTESIAN_POINT ( 'NONE',  ( 78.14518615778179367, 38.81718750108393579, -5.444914386472297529 ) ) ;
#26561 = CARTESIAN_POINT ( 'NONE',  ( 65.83892686928035687, 53.50081894914647052, -15.00000000000000000 ) ) ;
#26562 = CARTESIAN_POINT ( 'NONE',  ( 99.99999999999998579, 118.4984768113314146, -53.87500000273119127 ) ) ;
#26563 = CARTESIAN_POINT ( 'NONE',  ( 200.6228728715778686, 40.45429687500001137, 13.57481594606304576 ) ) ;
#26564 = DIRECTION ( 'NONE',  ( -0.000000000000000000, -1.000000000000000000, -0.000000000000000000 ) ) ;
#26565 = ORIENTED_EDGE ( 'NONE', *, *, #15657, .F. ) ;
#26566 = CARTESIAN_POINT ( 'NONE',  ( -5.444914386472297529, 37.42812500108394147, -13.14518615778179900 ) ) ;
#26567 = CARTESIAN_POINT ( 'NONE',  ( 104.4587341249999639, 1.442382525525748735E-14, 12.18750000136559208 ) ) ;
#26568 = EDGE_CURVE ( 'NONE', #1189, #28194, #6447, .T. ) ;
#26569 = CARTESIAN_POINT ( 'NONE',  ( 51.85481384221821344, 37.42812500108393436, 5.444914386472304635 ) ) ;
#26570 = LINE ( 'NONE', #18148, #21525 ) ;
#26571 = CARTESIAN_POINT ( 'NONE',  ( -13.09590655363597733, 36.00000000000000000, 1.137167824541468031 ) ) ;
#26572 = ADVANCED_FACE ( 'NONE', ( #17132 ), #10845, .F. ) ;
#26573 = CARTESIAN_POINT ( 'NONE',  ( 5.444914386472297529, 36.53515625108394715, -13.14518615778179722 ) ) ;
#26574 = EDGE_LOOP ( 'NONE', ( #21816, #22527, #12894, #14778 ) ) ;
#26575 = CARTESIAN_POINT ( 'NONE',  ( 13.57481594606304576, 34.25312499999999716, -1.662435489736055892E-15 ) ) ;
#26576 = CARTESIAN_POINT ( 'NONE',  ( 181.8548138422182205, 38.37070312608393152, 0.000000000000000000 ) ) ;
#26577 = CARTESIAN_POINT ( 'NONE',  ( 91.91746824999998466, 110.0000000000000000, -55.62499999726882294 ) ) ;
#26578 = ORIENTED_EDGE ( 'NONE', *, *, #11147, .T. ) ;
#26579 = AXIS2_PLACEMENT_3D ( 'NONE', #25182, #27340, #3379 ) ;
#26580 = CARTESIAN_POINT ( 'NONE',  ( -9.598844408820458085, 33.75703124999999005, -9.598844408820458085 ) ) ;
#26581 = CARTESIAN_POINT ( 'NONE',  ( -5.444914386472297529, 34.05468750108393294, -13.14518615778179900 ) ) ;
#26582 = ORIENTED_EDGE ( 'NONE', *, *, #6192, .T. ) ;
#26583 = CARTESIAN_POINT ( 'NONE',  ( 124.5550856135277087, 32.66562500108393863, -13.14518615778179900 ) ) ;
#26584 = CARTESIAN_POINT ( 'NONE',  ( 189.3771271284220745, 36.98164062716787015, -13.57481594606304753 ) ) ;
#26585 = ADVANCED_FACE ( 'NONE', ( #3141 ), #18040, .T. ) ;
#26586 = CARTESIAN_POINT ( 'NONE',  ( 195.0000000000000000, 34.20351562608394147, -13.14518615778179544 ) ) ;
#26587 = ORIENTED_EDGE ( 'NONE', *, *, #13803, .T. ) ;
#26588 = CARTESIAN_POINT ( 'NONE',  ( 97.93301270000000613, 124.5000000010924879, -0.8561741729129506151 ) ) ;
#26589 = CARTESIAN_POINT ( 'NONE',  ( -8.049105076161786076E-16, 31.62382812608393579, -13.14518615778179544 ) ) ;
#26590 = CARTESIAN_POINT ( 'NONE',  ( 103.5355339059327093, -3.535533905932726206, 5.500000002731185056 ) ) ;
#26591 = MANIFOLD_SOLID_BREP ( 'Thread1', #12590 ) ;
#26592 = CARTESIAN_POINT ( 'NONE',  ( 74.59884440882045453, 40.50390624999999289, 9.598844408820456309 ) ) ;
#26593 = CARTESIAN_POINT ( 'NONE',  ( 108.0825317500000011, 112.6261737610028320, -52.02500000273118985 ) ) ;
#26594 =( BOUNDED_CURVE ( )  B_SPLINE_CURVE ( 2, ( #12377, #14654, #7976, #5719, #23102, #25780, #8389, #17075, #23239 ),
 .UNSPECIFIED., .F., .F. ) 
 B_SPLINE_CURVE_WITH_KNOTS ( ( 3, 2, 2, 2, 3 ),
 ( 0.1458333333333336757, 0.1562500000000002776, 0.1666666666666669072, 0.1770833333333335369, 0.1875000000000001388 ),
 .UNSPECIFIED. ) 
 CURVE ( )  GEOMETRIC_REPRESENTATION_ITEM ( )  RATIONAL_B_SPLINE_CURVE ( ( 0.9999999999999975575, 0.9238795325112891810, 1.000000000000000000, 0.9238795325112867385, 1.000000000000000000, 0.9238795325112867385, 1.000000000000000000, 0.9238795325112857393, 1.000000000000001110 ) ) 
 REPRESENTATION_ITEM ( '' )  );
#26595 = CARTESIAN_POINT ( 'NONE',  ( 99.99999999999998579, 93.62499999726881583, 4.999999999999984013 ) ) ;
#26596 = CARTESIAN_POINT ( 'NONE',  ( 9.598844408820456309, 36.73359374999999716, -9.598844408820458085 ) ) ;
#26597 = CARTESIAN_POINT ( 'NONE',  ( 68.80305437324149409, 54.09082899096177499, 14.99999999999997868 ) ) ;
#26598 = EDGE_CURVE ( 'NONE', #27592, #9857, #20974, .T. ) ;
#26599 = VERTEX_POINT ( 'NONE', #20310 ) ;
#26600 = CARTESIAN_POINT ( 'NONE',  ( 104.4587341249999781, 1.846868145590750299, 3.000000001365592528 ) ) ;
#26601 = ORIENTED_EDGE ( 'NONE', *, *, #25176, .F. ) ;
#26602 = CARTESIAN_POINT ( 'NONE',  ( 100.8561741729129153, 122.7000000010924623, -2.066987299999999195 ) ) ;
#26603 = CARTESIAN_POINT ( 'NONE',  ( 104.4587341249999781, -1.846868145590721655, 8.875000001365593860 ) ) ;
#26604 = CARTESIAN_POINT ( 'NONE',  ( 137.6219635341832088, 54.91641323977227529, 14.99999999999996092 ) ) ;
#26605 = ADVANCED_FACE ( 'NONE', ( #3067 ), #11732, .T. ) ;
#26606 = CARTESIAN_POINT ( 'NONE',  ( 5.444914386472297529, 37.13046875108393152, -13.14518615778179900 ) ) ;
#26607 = DIRECTION ( 'NONE',  ( -0.000000000000000000, -1.000000000000000000, -0.000000000000000000 ) ) ;
#26608 = DIRECTION ( 'NONE',  ( -0.000000000000000000, -1.000000000000000000, -0.000000000000000000 ) ) ;
#26609 = CARTESIAN_POINT ( 'NONE',  ( 59.55508561352770158, 35.84062500108394289, -13.14518615778179900 ) ) ;
#26610 = CARTESIAN_POINT ( 'NONE',  ( 93.46109445667491400, 114.7507929638356785, -47.32500000273119412 ) ) ;
#26611 = CARTESIAN_POINT ( 'NONE',  ( -9.295050272127046043, 37.27929687608393294, -9.295050272127046043 ) ) ;
#26612 = EDGE_CURVE ( 'NONE', #10899, #26599, #26806, .T. ) ;
#26613 = CARTESIAN_POINT ( 'NONE',  ( 107.0000000000000284, 112.2744378736302906, -49.40000000546238113 ) ) ;
#26614 = CARTESIAN_POINT ( 'NONE',  ( 8.201446187642728702, 50.69246985422709173, 14.99999999999930012 ) ) ;
#26615 = CARTESIAN_POINT ( 'NONE',  ( -8.312177448680279460E-16, 35.24531249999999716, -13.57481594606304576 ) ) ;
#26616 = CARTESIAN_POINT ( 'NONE',  ( 130.0000000000000000, 36.43593749999999432, 13.57481594606304576 ) ) ;
#26617 = ORIENTED_EDGE ( 'NONE', *, *, #8960, .F. ) ;
#26618 = ADVANCED_FACE ( 'NONE', ( #18168 ), #9466, .T. ) ;
#26619 = ORIENTED_EDGE ( 'NONE', *, *, #11748, .F. ) ;
#26620 = CARTESIAN_POINT ( 'NONE',  ( 130.0000000000000000, 37.32890625216786873, 13.57481594606304576 ) ) ;
#26621 = CARTESIAN_POINT ( 'NONE',  ( -13.14518615778179900, 37.52734375108393294, -5.444914386472297529 ) ) ;
#26622 = CARTESIAN_POINT ( 'NONE',  ( -5.622872871577873077, 38.56914062716788294, -13.57481594606304753 ) ) ;
#26623 = CARTESIAN_POINT ( 'NONE',  ( 94.99999999999995737, -2.071067811865466624, 8.187500002731185944 ) ) ;
#26624 = CARTESIAN_POINT ( 'NONE',  ( 143.1451861577818079, 32.96328125108393436, 5.444914386472293977 ) ) ;
#26625 = CARTESIAN_POINT ( 'NONE',  ( 78.57481594606304043, 33.60820312716787583, -5.622872871577873077 ) ) ;
#26626 = CARTESIAN_POINT ( 'NONE',  ( 103.5355339059327093, 3.535533905932755072, 14.62500000000000000 ) ) ;
#26627 = CARTESIAN_POINT ( 'NONE',  ( -5.622872871577873077, 31.72304687716787441, 13.57481594606304753 ) ) ;
#26628 = CARTESIAN_POINT ( 'NONE',  ( 97.92893218813451028, -4.999999999999989342, 1.187499999999999334 ) ) ;
#26629 = CARTESIAN_POINT ( 'NONE',  ( 97.50236033167490746, 102.3130555110000159, -47.47499999726881725 ) ) ;
#26630 = AXIS2_PLACEMENT_3D ( 'NONE', #19316, #6481, #14879 ) ;
#26631 = CARTESIAN_POINT ( 'NONE',  ( 13.57481594606304753, 39.16445312716788152, -5.622872871577873077 ) ) ;
#26632 = CARTESIAN_POINT ( 'NONE',  ( 195.0000000000000000, 32.81445312608393294, 13.14518615778179544 ) ) ;
#26633 = CARTESIAN_POINT ( 'NONE',  ( 114.9999999999999858, 125.0000000000000000, -15.00000000000001066 ) ) ;
#26634 = CARTESIAN_POINT ( 'NONE',  ( 97.50000000000000000, 125.0254775906283697, 0.3826834323650784575 ) ) ;
#26635 = FACE_OUTER_BOUND ( 'NONE', #15084, .T. ) ;
#26636 = CARTESIAN_POINT ( 'NONE',  ( 99.99999999999995737, 83.25000000000000000, 4.999999999999990230 ) ) ;
#26637 = CARTESIAN_POINT ( 'NONE',  ( 99.99999999999995737, 5.000000000000018652, 12.75000000000000000 ) ) ;
#26638 = CARTESIAN_POINT ( 'NONE',  ( -13.57481594606304753, 38.56914062500000284, -5.622872871577873077 ) ) ;
#26639 = CARTESIAN_POINT ( 'NONE',  ( 143.5748159460630688, 38.27148437500000711, -5.622872871577873966 ) ) ;
#26640 = CARTESIAN_POINT ( 'NONE',  ( -9.295050272127044266, 32.91367187608393152, 9.295050272127047819 ) ) ;
#26641 = CARTESIAN_POINT ( 'NONE',  ( -5.444914386472297529, 34.84843750108393579, -13.14518615778179900 ) ) ;
#26642 = CARTESIAN_POINT ( 'NONE',  ( 195.0000000000000000, 33.26093749999999716, 13.57481594606304576 ) ) ;
#26643 = CARTESIAN_POINT ( 'NONE',  ( 5.622872871577871301, 36.88242187716787157, -13.57481594606304753 ) ) ;
#26645 = EDGE_CURVE ( 'NONE', #3142, #3824, #23821, .T. ) ;
#26644 = CARTESIAN_POINT ( 'NONE',  ( 102.0710678118654329, -4.999999999999989342, 4.437500002731185944 ) ) ;
#26646 = CARTESIAN_POINT ( 'NONE',  ( 2.493653234604083739E-15, 38.81718749999999574, 13.57481594606304576 ) ) ;
#26647 = CARTESIAN_POINT ( 'NONE',  ( 51.85481384221819923, 36.53515625108392584, -5.444914386472297529 ) ) ;
#26648 = CARTESIAN_POINT ( 'NONE',  ( 108.0825317500000011, 112.6261737610028320, -54.27500000273118275 ) ) ;
#26649 = CARTESIAN_POINT ( 'NONE',  ( 98.07597603534063069, 122.9999999999999858, 1.603032847902431612 ) ) ;
#26650 = CARTESIAN_POINT ( 'NONE',  ( 101.4615807364564546, 123.4500000010924765, -1.461580736456474794 ) ) ;
#26651 = CARTESIAN_POINT ( 'NONE',  ( 2.493653234604083739E-15, 34.05468749999999289, 13.57481594606304576 ) ) ;
#26652 = CARTESIAN_POINT ( 'NONE',  ( 124.5550856135277087, 39.01562500108394005, -13.14518615778179900 ) ) ;
#26653 = ORIENTED_EDGE ( 'NONE', *, *, #5500, .F. ) ;
#26654 = CARTESIAN_POINT ( 'NONE',  ( 96.46446609406721961, 81.12500000000000000, 3.535533905932727539 ) ) ;
#26655 = AXIS2_PLACEMENT_3D ( 'NONE', #28032, #10199, #8498 ) ;
#26656 = CARTESIAN_POINT ( 'NONE',  ( 94.99999999999997158, 2.071067811865471953, 5.937500000000001776 ) ) ;
#26657 = CARTESIAN_POINT ( 'NONE',  ( 96.46446609406721961, 82.25000000273119838, 3.535533905932727539 ) ) ;
#26658 = CARTESIAN_POINT ( 'NONE',  ( 95.00000000000000000, 93.50000000000000000, -7.551217303480904118E-15 ) ) ;
#26659 = FACE_OUTER_BOUND ( 'NONE', #9058, .T. ) ;
#26660 = CARTESIAN_POINT ( 'NONE',  ( 91.91746824999998466, 110.0000000000000000, -45.62499999726882294 ) ) ;
#26661 = CARTESIAN_POINT ( 'NONE',  ( 55.40115559117954547, 39.51171874999999289, 9.598844408820459861 ) ) ;
#26662 = CIRCLE ( 'NONE', #720, 13.57481594606304398 ) ;
#26663 = EDGE_LOOP ( 'NONE', ( #22200, #376, #5200, #13430 ) ) ;
#26664 = CARTESIAN_POINT ( 'NONE',  ( 93.00000000000000000, 110.0000000000000000, -50.50000000546237544 ) ) ;
#26665 = CARTESIAN_POINT ( 'NONE',  ( 104.9999999999999574, 2.071067811865491937, 14.56249999999999822 ) ) ;
#26666 = VERTEX_POINT ( 'NONE', #21435 ) ;
#26667 = CARTESIAN_POINT ( 'NONE',  ( 13.14518615778179544, 36.38632812608393863, -1.609821015232357215E-15 ) ) ;
#26668 = CARTESIAN_POINT ( 'NONE',  ( 189.3771271284221314, 33.01289062716787726, -13.57481594606304753 ) ) ;
#26669 = EDGE_LOOP ( 'NONE', ( #8160, #7791, #3213, #11519 ) ) ;
#26670 = CARTESIAN_POINT ( 'NONE',  ( -8.049105076161786076E-16, 31.62382812608393579, -13.14518615778179544 ) ) ;
#26671 = CARTESIAN_POINT ( 'NONE',  ( 217.9999999999999716, 78.00000000000000000, -13.00000000000000000 ) ) ;
#26672 = DIRECTION ( 'NONE',  ( 0.000000000000000000, -1.000000000000000000, -0.000000000000000000 ) ) ;
#26673 = CARTESIAN_POINT ( 'NONE',  ( 5.444914386472302859, 35.44375000108393436, 13.14518615778179189 ) ) ;
#26674 = DIRECTION ( 'NONE',  ( 5.782411586589357392E-17, -0.000000000000000000, 1.000000000000000000 ) ) ;
#26675 = CARTESIAN_POINT ( 'NONE',  ( 68.87838529739120474, 32.03609435653363136, -13.57481594606304576 ) ) ;
#26676 = CARTESIAN_POINT ( 'NONE',  ( 102.0710678118654755, 91.81250000000000000, 4.999999999999961808 ) ) ;
#26677 = CARTESIAN_POINT ( 'NONE',  ( 119.2131532318157952, 36.00000000000000000, 7.561388982944516002 ) ) ;
#26678 = CARTESIAN_POINT ( 'NONE',  ( 104.4587341249999781, -1.846868145590721655, 11.12500000136559386 ) ) ;
#26679 = CARTESIAN_POINT ( 'NONE',  ( 99.99999999999998579, 95.00000000000000000, -6.938893903907228378E-15 ) ) ;
#26680 = CARTESIAN_POINT ( 'NONE',  ( 96.84719886470459471, -3.152801135295355994, 13.56250000136559208 ) ) ;
#26681 = CARTESIAN_POINT ( 'NONE',  ( 93.46109445667491400, 105.2492070361643215, -48.92500000273119554 ) ) ;
#26682 = CARTESIAN_POINT ( 'NONE',  ( 98.15313185440925281, 91.87499999863439371, -4.458734124999994997 ) ) ;
#26683 = VECTOR ( 'NONE', #22474, 1000.000000000000000 ) ;
#26684 = CARTESIAN_POINT ( 'NONE',  ( 104.9999999999999716, 83.62500000273119838, -1.449011120738813565E-14 ) ) ;
#26685 = CARTESIAN_POINT ( 'NONE',  ( 95.00472066334981491, 116.8754121666685393, -51.92499999726881299 ) ) ;
#26686 = CARTESIAN_POINT ( 'NONE',  ( 5.444914386472302859, 36.23750000108393721, 13.14518615778179189 ) ) ;
#26687 = ORIENTED_EDGE ( 'NONE', *, *, #5102, .F. ) ;
#26688 = CARTESIAN_POINT ( 'NONE',  ( 2.493653234604083739E-15, 38.02343749999999289, 13.57481594606304576 ) ) ;
#26689 = CARTESIAN_POINT ( 'NONE',  ( 97.92893218813455292, 91.68749999999997158, 5.000000000000003553 ) ) ;
#26690 = CARTESIAN_POINT ( 'NONE',  ( 195.0000000000000000, 34.40195312608393152, 13.14518615778179544 ) ) ;
#26691 = ORIENTED_EDGE ( 'NONE', *, *, #5336, .T. ) ;
#26692 = CARTESIAN_POINT ( 'NONE',  ( 203.2113140151944890, 50.68678854790359622, -14.99999999999862332 ) ) ;
#26693 = CARTESIAN_POINT ( 'NONE',  ( 95.54126587499995082, -1.846868145590724986, 12.75000000136559386 ) ) ;
#26694 = ADVANCED_FACE ( 'NONE', ( #14577 ), #27989, .T. ) ;
#26695 = VERTEX_POINT ( 'NONE', #25281 ) ;
#26696 = CARTESIAN_POINT ( 'NONE',  ( 91.91746824999998466, 107.3738262389971538, -53.27500000273119696 ) ) ;
#26697 = CARTESIAN_POINT ( 'NONE',  ( 5.444914386472297529, 37.13046875108393152, -13.14518615778179900 ) ) ;
#26698 = VECTOR ( 'NONE', #14055, 1000.000000000000000 ) ;
#26699 = CARTESIAN_POINT ( 'NONE',  ( 99.99999999999995737, 79.37500000273119838, 4.999999999999990230 ) ) ;
#26700 = CARTESIAN_POINT ( 'NONE',  ( 130.0000000000000000, 36.78320312608393294, 13.14518615778179544 ) ) ;
#26701 = CARTESIAN_POINT ( 'NONE',  ( 9.295050272127046043, 40.45429687608393721, -9.295050272127046043 ) ) ;
#26702 = CARTESIAN_POINT ( 'NONE',  ( -9.295050272127044266, 36.68398437608392726, 9.295050272127047819 ) ) ;
#26703 = CARTESIAN_POINT ( 'NONE',  ( 99.99999999999998579, 92.62499999726881583, 4.999999999999984013 ) ) ;
#26704 = CARTESIAN_POINT ( 'NONE',  ( 70.44491438647230552, 36.53515625108393294, -13.14518615778179900 ) ) ;
#26705 = CARTESIAN_POINT ( 'NONE',  ( 63.10781664291035753, 53.66387243068089674, -15.00000000000000000 ) ) ;
#26706 = CARTESIAN_POINT ( 'NONE',  ( 93.46109445667491400, 105.2492070361643215, -49.17500000273119554 ) ) ;
#26707 = CARTESIAN_POINT ( 'NONE',  ( 189.5550856135277229, 32.96328125108393436, 13.14518615778179722 ) ) ;
#26708 = CARTESIAN_POINT ( 'NONE',  ( 65.00000000000000000, 38.42031249999999432, -13.57481594606304576 ) ) ;
#26709 = ORIENTED_EDGE ( 'NONE', *, *, #27487, .F. ) ;
#26710 = CARTESIAN_POINT ( 'NONE',  ( -13.14518615778179900, 35.14609375108393152, -5.444914386472297529 ) ) ;
#26711 = CARTESIAN_POINT ( 'NONE',  ( 95.54126587499996504, 1.846868145590750077, 5.625000001365592972 ) ) ;
#26712 =( BOUNDED_CURVE ( )  B_SPLINE_CURVE ( 2, ( #11399, #22115, #20118, #596, #6704, #9276, #17689, #21838, #8709, #21974, #15245, #2451, #2168, #15392, #26680, #10830, #4445, #7128, #23824, #23966, #4303, #26245, #12960, #21694, #8996, #17541, #2314, #19546, #13097, #26394, #6848, #10971, #15537, #4728, #19683, #13388, #2595, #27111, #20404, #13962, #13681, #20255, #26970, #9703, #22687, #20691, #16109, #1174, #5297, #3157, #740, #5584, #24814, #11968, #9839, #7561, #9414, #11827, #12100, #16401, #27250, #14249, #18546, #7414, #22970, #18404, #13818, #18113, #20551, #7273, #1032, #22398, #16255, #18685, #2867, #24678, #3434, #15825, #26827, #7707, #9973, #25099, #20827, #24955, #889, #22542, #1304, #27388, #9560, #5440, #5155, #14108, #22832, #15964, #3298, #24530, #5016, #18263, #11538, #3010, #11681, #18950, #1721, #5992, #12657, #8121, #21382, #25513, #14527, #16942, #14657, #12796, #3850, #12381, #23655, #25377, #27933, #10661, #10104, #25783, #1861, #10526, #19090, #19232, #16816, #19369, #16542, #8392, #18817, #17081, #23378, #12511, #6261, #8255, #14934, #25232, #14792, #4131, #3579, #21515, #1994, #1448, #5723, #7847, #23515, #16678, #14388, #27799, #23105, #12236, #20965, #27524, #7980, #5857, #21239, #23242, #3719, #10383, #25643, #21099, #1587, #10242, #3994, #27659, #6127, #19939, #15505, #132, #22083, #2560, #11221, #418, #4410, #22223, #19792, #19512, #8961, #2703, #11081, #13065, #26209, #26065, #4267, #10938, #21944, #6671, #4694, #8818, #13355, #17507, #6534, #17649, #15357, #4842, #24072, #21802, #15652, #17369, #9104, #11362, #2134, #2422, #4549, #17798, #274, #26501, #13210, #28072, #8537, #6957, #10799, #24351, #26357, #6815, #13503, #24215, #17223, #25928, #6403, #15072, #23790, #12926, #21658, #8130, #8679 ),
 .UNSPECIFIED., .F., .F. ) 
 B_SPLINE_CURVE_WITH_KNOTS ( ( 3, 2, 2, 2, 2, 2, 2, 2, 2, 2, 2, 2, 2, 2, 2, 2, 2, 2, 2, 2, 2, 2, 2, 2, 2, 2, 2, 2, 2, 2, 2, 2, 2, 2, 2, 2, 2, 2, 2, 2, 2, 2, 2, 2, 2, 2, 2, 2, 2, 2, 2, 2, 2, 2, 2, 2, 2, 2, 2, 2, 2, 2, 2, 2, 2, 2, 2, 2, 2, 2, 2, 2, 2, 2, 2, 2, 2, 2, 2, 2, 2, 2, 2, 2, 2, 2, 2, 2, 2, 2, 2, 2, 2, 2, 2, 2, 2, 2, 2, 2, 2, 2, 2, 2, 2, 2, 2, 2, 2, 2, 2, 2, 3 ),
 ( 0.000000000000000000, 0.008928571428571428076, 0.01785714285714285615, 0.02678571428571428423, 0.03571428571428571230, 0.04464285714285714385, 0.05357142857142856845, 0.06250000000000000000, 0.07142857142857142461, 0.08035714285714286309, 0.08928571428571428770, 0.09821428571428571230, 0.1071428571428571369, 0.1160714285714285754, 0.1250000000000000000, 0.1339285714285714246, 0.1428571428571428492, 0.1517857142857142738, 0.1607142857142857262, 0.1696428571428571508, 0.1785714285714285754, 0.1875000000000000000, 0.1964285714285714246, 0.2053571428571428492, 0.2142857142857142738, 0.2232142857142857262, 0.2321428571428571508, 0.2410714285714285754, 0.2500000000000000000, 0.2589285714285714524, 0.2678571428571428492, 0.2767857142857143016, 0.2857142857142856984, 0.2946428571428571508, 0.3035714285714285476, 0.3125000000000000000, 0.3214285714285714524, 0.3303571428571428492, 0.3392857142857143016, 0.3482142857142856984, 0.3571428571428571508, 0.3660714285714285476, 0.3750000000000000000, 0.3839285714285714524, 0.3928571428571428492, 0.4017857142857143016, 0.4107142857142856984, 0.4196428571428571508, 0.4285714285714285476, 0.4375000000000000000, 0.4464285714285714524, 0.4553571428571428492, 0.4642857142857143016, 0.4732142857142856984, 0.4821428571428571508, 0.4910714285714285476, 0.5000000000000000000, 0.5089285714285713969, 0.5178571428571429047, 0.5267857142857143016, 0.5357142857142856984, 0.5446428571428570953, 0.5535714285714286031, 0.5625000000000000000, 0.5714285714285713969, 0.5803571428571429047, 0.5892857142857143016, 0.5982142857142856984, 0.6071428571428570953, 0.6160714285714286031, 0.6250000000000000000, 0.6339285714285713969, 0.6428571428571429047, 0.6517857142857143016, 0.6607142857142856984, 0.6696428571428570953, 0.6785714285714286031, 0.6875000000000000000, 0.6964285714285713969, 0.7053571428571429047, 0.7142857142857143016, 0.7232142857142856984, 0.7321428571428570953, 0.7410714285714286031, 0.7500000000000000000, 0.7589285714285713969, 0.7678571428571429047, 0.7767857142857143016, 0.7857142857142856984, 0.7946428571428570953, 0.8035714285714286031, 0.8125000000000000000, 0.8214285714285713969, 0.8303571428571429047, 0.8392857142857143016, 0.8482142857142856984, 0.8571428571428570953, 0.8660714285714286031, 0.8750000000000000000, 0.8839285714285713969, 0.8928571428571429047, 0.9017857142857143016, 0.9107142857142856984, 0.9196428571428570953, 0.9285714285714286031, 0.9375000000000000000, 0.9464285714285713969, 0.9553571428571429047, 0.9642857142857143016, 0.9732142857142856984, 0.9821428571428570953, 0.9910714285714286031, 1.000000000000000000 ),
 .UNSPECIFIED. ) 
 CURVE ( )  GEOMETRIC_REPRESENTATION_ITEM ( )  RATIONAL_B_SPLINE_CURVE ( ( 1.000000000000000000, 0.9238795325112867385, 1.000000000000000000, 0.9238795325112867385, 1.000000000000000000, 0.9238795325112867385, 1.000000000000000000, 0.9238795325112867385, 1.000000000000000000, 0.9238795325112867385, 1.000000000000000000, 0.9238795325112867385, 1.000000000000000000, 0.9238795325112867385, 1.000000000000000000, 0.9238795325112867385, 1.000000000000000000, 0.9238795325112867385, 1.000000000000000000, 0.9238795325112867385, 1.000000000000000000, 0.9238795325112867385, 1.000000000000000000, 0.9238795325112867385, 1.000000000000000000, 0.9238795325112867385, 1.000000000000000000, 0.9238795325112867385, 1.000000000000000000, 0.9238795325112867385, 1.000000000000000000, 0.9238795325112867385, 1.000000000000000000, 0.9238795325112867385, 1.000000000000000000, 0.9238795325112867385, 1.000000000000000000, 0.9238795325112867385, 1.000000000000000000, 0.9238795325112867385, 1.000000000000000000, 0.9238795325112867385, 1.000000000000000000, 0.9238795325112867385, 1.000000000000000000, 0.9238795325112867385, 1.000000000000000000, 0.9238795325112867385, 1.000000000000000000, 0.9238795325112867385, 1.000000000000000000, 0.9238795325112867385, 1.000000000000000000, 0.9238795325112867385, 1.000000000000000000, 0.9238795325112867385, 1.000000000000000000, 0.9238795325112867385, 1.000000000000000000, 0.9238795325112867385, 1.000000000000000000, 0.9238795325112867385, 1.000000000000000000, 0.9238795325112867385, 1.000000000000000000, 0.9238795325112867385, 1.000000000000000000, 0.9238795325112867385, 1.000000000000000000, 0.9238795325112867385, 1.000000000000000000, 0.9238795325112867385, 1.000000000000000000, 0.9238795325112867385, 1.000000000000000000, 0.9238795325112867385, 1.000000000000000000, 0.9238795325112867385, 1.000000000000000000, 0.9238795325112867385, 1.000000000000000000, 0.9238795325112867385, 1.000000000000000000, 0.9238795325112867385, 1.000000000000000000, 0.9238795325112867385, 1.000000000000000000, 0.9238795325112867385, 1.000000000000000000, 0.9238795325112867385, 1.000000000000000000, 0.9238795325112867385, 1.000000000000000000, 0.9238795325112867385, 1.000000000000000000, 0.9238795325112867385, 1.000000000000000000, 0.9238795325112867385, 1.000000000000000000, 0.9238795325112867385, 1.000000000000000000, 0.9238795325112867385, 1.000000000000000000, 0.9238795325112867385, 1.000000000000000000, 0.9238795325112867385, 1.000000000000000000, 0.9238795325112867385, 1.000000000000000000, 0.9238795325112867385, 1.000000000000000000, 0.9238795325112867385, 1.000000000000000000, 0.9238795325112867385, 1.000000000000000000, 0.9238795325112867385, 1.000000000000000000, 0.9238795325112867385, 1.000000000000000000, 0.9238795325112867385, 1.000000000000000000, 0.9238795325112867385, 1.000000000000000000, 0.9238795325112867385, 1.000000000000000000, 0.9238795325112867385, 1.000000000000000000, 0.9238795325112867385, 1.000000000000000000, 0.9238795325112867385, 1.000000000000000000, 0.9238795325112867385, 1.000000000000000000, 0.9238795325112867385, 1.000000000000000000, 0.9238795325112867385, 1.000000000000000000, 0.9238795325112867385, 1.000000000000000000, 0.9238795325112867385, 1.000000000000000000, 0.9238795325112867385, 1.000000000000000000, 0.9238795325112867385, 1.000000000000000000, 0.9238795325112867385, 1.000000000000000000, 0.9238795325112867385, 1.000000000000000000, 0.9238795325112867385, 1.000000000000000000, 0.9238795325112867385, 1.000000000000000000, 0.9238795325112867385, 1.000000000000000000, 0.9238795325112867385, 1.000000000000000000, 0.9238795325112867385, 1.000000000000000000, 0.9238795325112867385, 1.000000000000000000, 0.9238795325112867385, 1.000000000000000000, 0.9238795325112867385, 1.000000000000000000, 0.9238795325112867385, 1.000000000000000000, 0.9238795325112867385, 1.000000000000000000, 0.9238795325112867385, 1.000000000000000000, 0.9238795325112867385, 1.000000000000000000, 0.9238795325112867385, 1.000000000000000000, 0.9238795325112867385, 1.000000000000000000, 0.9238795325112867385, 1.000000000000000000, 0.9238795325112867385, 1.000000000000000000, 0.9238795325112867385, 1.000000000000000000, 0.9238795325112867385, 1.000000000000000000, 0.9238795325112867385, 1.000000000000000000, 0.9238795325112867385, 1.000000000000000000, 0.9238795325112867385, 1.000000000000000000, 0.9238795325112867385, 1.000000000000000000, 0.9238795325112867385, 1.000000000000000000, 0.9238795325112867385, 1.000000000000000000, 0.9238795325112867385, 1.000000000000000000, 0.9238795325112867385, 1.000000000000000000, 0.9238795325112867385, 1.000000000000000000, 0.9238795325112867385, 1.000000000000000000, 0.9238795325112867385, 1.000000000000000000, 0.9238795325112867385, 1.000000000000000000, 0.9238795325112867385, 1.000000000000000000, 0.9238795325112867385, 1.000000000000000000, 0.9238795325112867385, 1.000000000000000000, 0.9238795325112867385, 1.000000000000000000, 0.9238795325112867385, 1.000000000000000000, 0.9238795325112867385, 1.000000000000000000, 0.9238795325112867385, 1.000000000000000000, 0.9238795325112867385, 1.000000000000000000 ) ) 
 REPRESENTATION_ITEM ( '' )  );
#26713 = CIRCLE ( 'NONE', #23976, 5.000000000000004441 ) ;
#26714 = DIRECTION ( 'NONE',  ( -0.000000000000000000, 1.000000000000000000, -0.000000000000000000 ) ) ;
#26715 = CARTESIAN_POINT ( 'NONE',  ( 0.000000000000000000, -7.395377635281828788, 0.000000000000000000 ) ) ;
#26716 = DIRECTION ( 'NONE',  ( 1.040834085586084257E-15, 0.000000000000000000, 1.000000000000000000 ) ) ;
#26717 = CARTESIAN_POINT ( 'NONE',  ( -5.444914386472299306, 36.13828125108393152, 13.14518615778179722 ) ) ;
#26718 = AXIS2_PLACEMENT_3D ( 'NONE', #16624, #23190, #7927 ) ;
#26719 = CARTESIAN_POINT ( 'NONE',  ( 98.15313185440923860, 90.87499999863439371, -4.458734124999994997 ) ) ;
#26720 = CARTESIAN_POINT ( 'NONE',  ( 195.0000000000000000, 38.17226562608394147, -13.14518615778179544 ) ) ;
#26721 = CARTESIAN_POINT ( 'NONE',  ( 108.0825317499999869, 112.6261737610028320, -50.77499999726882152 ) ) ;
#26722 = AXIS2_PLACEMENT_3D ( 'NONE', #12964, #13102, #19549 ) ;
#26723 = VERTEX_POINT ( 'NONE', #17138 ) ;
#26724 = CARTESIAN_POINT ( 'NONE',  ( 9.598844408820456309, 34.35234374999999574, -9.598844408820458085 ) ) ;
#26725 = CARTESIAN_POINT ( 'NONE',  ( 13.14518615778179544, 33.01289062608393010, -1.609821015232357215E-15 ) ) ;
#26726 = ORIENTED_EDGE ( 'NONE', *, *, #5269, .F. ) ;
#26727 = CARTESIAN_POINT ( 'NONE',  ( 130.0000000000000000, 33.40976562608393863, -13.14518615778179544 ) ) ;
#26728 = CARTESIAN_POINT ( 'NONE',  ( 189.3771271284220177, 37.27929687716785878, 13.57481594606295161 ) ) ;
#26729 = CARTESIAN_POINT ( 'NONE',  ( 181.8548138422181921, 32.76484375108393010, -5.444914386472297529 ) ) ;
#26730 = VERTEX_POINT ( 'NONE', #1774 ) ;
#26731 = CARTESIAN_POINT ( 'NONE',  ( 99.99999999999998579, 124.3500000010924822, -2.066987299999998751 ) ) ;
#26732 = CARTESIAN_POINT ( 'NONE',  ( 96.46446609406721961, -3.535533905932727539, 5.250000002731184168 ) ) ;
#26733 = AXIS2_PLACEMENT_3D ( 'NONE', #15824, #15536, #13537 ) ;
#26734 = ADVANCED_FACE ( 'NONE', ( #10294, #27851 ), #16997, .T. ) ;
#26735 = CARTESIAN_POINT ( 'NONE',  ( 65.00000000000000000, 36.53515625216787299, 13.57481594606304576 ) ) ;
#26736 = CARTESIAN_POINT ( 'NONE',  ( 91.91746824999999887, 110.0000000000000000, -49.12500000273119838 ) ) ;
#26737 = ADVANCED_FACE ( 'NONE', ( #10024 ), #18733, .F. ) ;
#26738 = CARTESIAN_POINT ( 'NONE',  ( 94.99999999999995737, 1.387778780781445676E-14, 2.125000002731185056 ) ) ;
#26739 = CARTESIAN_POINT ( 'NONE',  ( 195.0000000000000000, 50.00000000000000000, -13.57481594606306707 ) ) ;
#26740 = CARTESIAN_POINT ( 'NONE',  ( 189.5550856135277229, 40.10703125108393152, 13.14518615778179722 ) ) ;
#26741 = ORIENTED_EDGE ( 'NONE', *, *, #17674, .F. ) ;
#26742 = CARTESIAN_POINT ( 'NONE',  ( 98.15313185440925281, 4.458734125000016313, 5.250000001365592972 ) ) ;
#26743 = ORIENTED_EDGE ( 'NONE', *, *, #1669, .F. ) ;
#26744 = CARTESIAN_POINT ( 'NONE',  ( -0.1722897647759079331, 36.00000000000000000, -13.51468191220838122 ) ) ;
#26745 = CARTESIAN_POINT ( 'NONE',  ( 95.54126587499996504, 1.387778780781445676E-14, 8.437500001365592084 ) ) ;
#26746 = CARTESIAN_POINT ( 'NONE',  ( 143.5748159460630688, 38.32109375216786873, -1.662435489736055892E-15 ) ) ;
#26747 = EDGE_CURVE ( 'NONE', #15111, #18823, #14438, .T. ) ;
#26748 = CARTESIAN_POINT ( 'NONE',  ( 2.414731522848535132E-15, 34.40195312608393152, 13.14518615778179544 ) ) ;
#26749 = CARTESIAN_POINT ( 'NONE',  ( -2.297960586008104045, 36.00000000000001421, 12.97104423350682900 ) ) ;
#26750 = CARTESIAN_POINT ( 'NONE',  ( 74.29505027212704249, 32.31835937608393294, 9.295050272127046043 ) ) ;
#26751 = CARTESIAN_POINT ( 'NONE',  ( 98.15313185440925281, 91.99999999863439371, 4.458734124999979898 ) ) ;
#26752 = CARTESIAN_POINT ( 'NONE',  ( -13.14518615778179544, 40.75195312608393294, 0.000000000000000000 ) ) ;
#26753 = CARTESIAN_POINT ( 'NONE',  ( -13.14518615778179189, 39.01562500108393294, 5.444914386472304635 ) ) ;
#26754 = AXIS2_PLACEMENT_3D ( 'NONE', #2683, #13192, #2818 ) ;
#26755 = CARTESIAN_POINT ( 'NONE',  ( 95.67376207875072680, 115.9545556584642867, -48.80000000546237260 ) ) ;
#26756 = CARTESIAN_POINT ( 'NONE',  ( -9.180175813647990068, 50.00000000000000000, 9.999999999999998224 ) ) ;
#26757 = CARTESIAN_POINT ( 'NONE',  ( 0.000000000000000000, 40.99999999999999289, -13.57481594606304576 ) ) ;
#26758 = CARTESIAN_POINT ( 'NONE',  ( 116.4251840539369454, 34.60039062499999574, -5.622872871577873077 ) ) ;
#26759 = ORIENTED_EDGE ( 'NONE', *, *, #6735, .F. ) ;
#26760 = CARTESIAN_POINT ( 'NONE',  ( 94.99999999999997158, -2.071067811865486608, 8.062500000000000000 ) ) ;
#26761 = CARTESIAN_POINT ( 'NONE',  ( -9.295050272127046043, 35.09648437608393579, -9.295050272127046043 ) ) ;
#26762 = CARTESIAN_POINT ( 'NONE',  ( 9.598844408820459861, 35.04687500216787299, 9.598844408820456309 ) ) ;
#26763 = CARTESIAN_POINT ( 'NONE',  ( 102.0710678118654329, 5.000000000000018652, 9.812500002731184168 ) ) ;
#26764 = CARTESIAN_POINT ( 'NONE',  ( 120.7049497278729575, 34.89804687608393152, -9.295050272127046043 ) ) ;
#26765 = CARTESIAN_POINT ( 'NONE',  ( 55.40115559117954547, 31.67343750216787512, 9.598844408820459861 ) ) ;
#26766 = EDGE_CURVE ( 'NONE', #467, #5516, #3630, .T. ) ;
#26767 = ORIENTED_EDGE ( 'NONE', *, *, #24509, .F. ) ;
#26768 =( BOUNDED_CURVE ( )  B_SPLINE_CURVE ( 2, ( #15401, #13250, #21982, #2458, #10703, #19409, #13396, #11120, #6574, #23975, #19834 ),
 .UNSPECIFIED., .F., .F. ) 
 B_SPLINE_CURVE_WITH_KNOTS ( ( 3, 2, 2, 2, 2, 3 ),
 ( 0.2000000000000001776, 0.2200000000000001676, 0.2400000000000001854, 0.2600000000000002309, 0.2800000000000002487, 0.3000000000000002109 ),
 .UNSPECIFIED. ) 
 CURVE ( )  GEOMETRIC_REPRESENTATION_ITEM ( )  RATIONAL_B_SPLINE_CURVE ( ( 0.9999999999999995559, 0.9510565162951539753, 1.000000000000000000, 0.9510565162951535312, 1.000000000000000000, 0.9510565162951535312, 1.000000000000000000, 0.9510565162951535312, 1.000000000000000000, 0.9510565162951529761, 1.000000000000000444 ) ) 
 REPRESENTATION_ITEM ( '' )  );
#26769 = CARTESIAN_POINT ( 'NONE',  ( 51.42518405393695957, 37.13046875216787868, 0.000000000000000000 ) ) ;
#26770 = CARTESIAN_POINT ( 'NONE',  ( -5.444914386472299306, 39.90859375108393436, 13.14518615778179722 ) ) ;
#26771 = CARTESIAN_POINT ( 'NONE',  ( 102.4999999999999858, 123.8500000021849416, 1.035533905932722876 ) ) ;
#26772 = CARTESIAN_POINT ( 'NONE',  ( 104.9952793366501567, 116.8754121666685393, -50.57499999726882578 ) ) ;
#26773 = CARTESIAN_POINT ( 'NONE',  ( -5.622872871577873077, 39.66054687716786731, 13.57481594606304753 ) ) ;
#26774 = CARTESIAN_POINT ( 'NONE',  ( 204.2950502721270425, 33.70742187608393436, 9.295050272127046043 ) ) ;
#26775 = DIRECTION ( 'NONE',  ( -5.551115123125783491E-15, 0.000000000000000000, -1.000000000000000000 ) ) ;
#26776 = CARTESIAN_POINT ( 'NONE',  ( -9.598844408820458085, 33.06250000216787299, -9.598844408820458085 ) ) ;
#26777 = EDGE_CURVE ( 'NONE', #11583, #18595, #13101, .T. ) ;
#26778 = CARTESIAN_POINT ( 'NONE',  ( 102.0669872999999797, 124.1500000010924794, -9.794112055954760458E-15 ) ) ;
#26779 = DIRECTION ( 'NONE',  ( -0.000000000000000000, -1.000000000000000000, -0.000000000000000000 ) ) ;
#26780 = CARTESIAN_POINT ( 'NONE',  ( -8.312177448680279460E-16, 36.83281249999999574, -13.57481594606304576 ) ) ;
#26781 = PLANE ( 'NONE',  #11475 ) ;
#26782 = CARTESIAN_POINT ( 'NONE',  ( -13.57481594606304576, 33.85624999999999574, 0.000000000000000000 ) ) ;
#26783 = CARTESIAN_POINT ( 'NONE',  ( 135.6228728715777834, 38.37070312499999858, -13.57481594606313990 ) ) ;
#26784 = CARTESIAN_POINT ( 'NONE',  ( -8.049105076161786076E-16, 35.79101562608394005, -13.14518615778179544 ) ) ;
#26785 = CARTESIAN_POINT ( 'NONE',  ( -9.295050272127044266, 36.68398437608392726, 9.295050272127047819 ) ) ;
#26786 = CARTESIAN_POINT ( 'NONE',  ( -5.444914386472299306, 35.14609375108393152, 13.14518615778179722 ) ) ;
#26787 = CARTESIAN_POINT ( 'NONE',  ( -13.57481594606304576, 34.79882812716787299, 5.622872871577880183 ) ) ;
#26788 = CARTESIAN_POINT ( 'NONE',  ( 104.9999999999999716, 1.449011120738813565E-14, 4.625000002731185944 ) ) ;
#26789 = CARTESIAN_POINT ( 'NONE',  ( 103.1528011352953342, 83.06250000136560629, -3.152801135295383084 ) ) ;
#26790 = CARTESIAN_POINT ( 'NONE',  ( 74.29505027212704249, 32.31835937608393294, -9.295050272127046043 ) ) ;
#26791 = CARTESIAN_POINT ( 'NONE',  ( 108.0825317500000011, 112.6261737610028320, -52.27500000273118985 ) ) ;
#26792 = CARTESIAN_POINT ( 'NONE',  ( 99.53100023034451738, 122.9999999999999716, 2.460289198665830401 ) ) ;
#26793 = CARTESIAN_POINT ( 'NONE',  ( 98.53841926354351699, 124.4500000010924765, -1.461580736456474794 ) ) ;
#26794 = CARTESIAN_POINT ( 'NONE',  ( -5.622872871577873077, 32.11992187499999574, -13.57481594606304753 ) ) ;
#26795 = CARTESIAN_POINT ( 'NONE',  ( 120.7049497278729575, 36.68398437608393436, -9.295050272127046043 ) ) ;
#26796 = ORIENTED_EDGE ( 'NONE', *, *, #5823, .T. ) ;
#26797 = FACE_OUTER_BOUND ( 'NONE', #19034, .T. ) ;
#26798 = CARTESIAN_POINT ( 'NONE',  ( 104.4587341249999781, 83.87500000136560629, 1.846868145590721655 ) ) ;
#26799 = CARTESIAN_POINT ( 'NONE',  ( 104.9999999999999716, 93.93749999999998579, 2.071067811865467956 ) ) ;
#26800 = CARTESIAN_POINT ( 'NONE',  ( 51.42518405393695957, 39.51171875216787299, 0.000000000000000000 ) ) ;
#26801 = AXIS2_PLACEMENT_3D ( 'NONE', #4231, #25748, #6230 ) ;
#26802 = CARTESIAN_POINT ( 'NONE',  ( 93.46109445667489979, 114.7507929638356785, -49.82499999726882578 ) ) ;
#26803 = CARTESIAN_POINT ( 'NONE',  ( 65.00000000000000000, 32.21914062608393436, 13.14518615778179544 ) ) ;
#26804 = PRODUCT_DEFINITION_FORMATION_WITH_SPECIFIED_SOURCE ( 'ANY', '', #7403, .NOT_KNOWN. ) ;
#26805 = ORIENTED_EDGE ( 'NONE', *, *, #23587, .T. ) ;
#26806 =( BOUNDED_CURVE ( )  B_SPLINE_CURVE ( 2, ( #27022, #22878, #25013, #11590, #1082, #7177, #3205, #14298, #796 ),
 .UNSPECIFIED., .F., .F. ) 
 B_SPLINE_CURVE_WITH_KNOTS ( ( 3, 2, 2, 2, 3 ),
 ( 0.05000000000000004441, 0.07500000000000006661, 0.1000000000000000888, 0.1250000000000001110, 0.1500000000000001332 ),
 .UNSPECIFIED. ) 
 CURVE ( )  GEOMETRIC_REPRESENTATION_ITEM ( )  RATIONAL_B_SPLINE_CURVE ( ( 0.9999999999999998890, 0.9238795325112868495, 1.000000000000000000, 0.9238795325112867385, 1.000000000000000000, 0.9238795325112867385, 1.000000000000000000, 0.9238795325112862944, 1.000000000000000444 ) ) 
 REPRESENTATION_ITEM ( '' )  );
#26807 = DIRECTION ( 'NONE',  ( -0.000000000000000000, 1.000000000000000000, -0.000000000000000000 ) ) ;
#26808 = CARTESIAN_POINT ( 'NONE',  ( 97.92893218813451028, -4.999999999999989342, 14.18749999999999822 ) ) ;
#26809 = ORIENTED_EDGE ( 'NONE', *, *, #11267, .F. ) ;
#26810 = SHAPE_REPRESENTATION ( 'vaccum generator', ( #26844 ), #4064 ) ;
#26811 = CARTESIAN_POINT ( 'NONE',  ( 9.295050272127046043, 35.69179687608394147, -9.295050272127046043 ) ) ;
#26812 = CARTESIAN_POINT ( 'NONE',  ( 200.6228728715778686, 34.20351562716788862, 13.57481594606304576 ) ) ;
#26813 = VERTEX_POINT ( 'NONE', #22133 ) ;
#26814 = CARTESIAN_POINT ( 'NONE',  ( -13.14518615778179544, 32.61601562608393579, 0.000000000000000000 ) ) ;
#26815 = EDGE_CURVE ( 'NONE', #17847, #3914, #16034, .T. ) ;
#26816 = CARTESIAN_POINT ( 'NONE',  ( 0.000000000000000000, 0.000000000000000000, 0.000000000000000000 ) ) ;
#26817 = CARTESIAN_POINT ( 'NONE',  ( 99.99999999999998579, 138.0000000000000000, -10.50000000000002132 ) ) ;
#26818 = CARTESIAN_POINT ( 'NONE',  ( 13.14518615778179900, 34.84843750108393579, -5.444914386472297529 ) ) ;
#26819 = CARTESIAN_POINT ( 'NONE',  ( 99.99999999999998579, 102.6397644303321215, -50.00000000546236834 ) ) ;
#26820 = CARTESIAN_POINT ( 'NONE',  ( 65.00000000000000000, 32.86406249999999574, -13.57481594606304576 ) ) ;
#26821 = CARTESIAN_POINT ( 'NONE',  ( 100.0000000000000000, 110.0000000000000000, -55.00000000000000711 ) ) ;
#26822 = AXIS2_PLACEMENT_3D ( 'NONE', #21820, #11381, #19808 ) ;
#26823 = DIRECTION ( 'NONE',  ( 0.000000000000000000, 0.000000000000000000, 1.000000000000000000 ) ) ;
#26824 = CARTESIAN_POINT ( 'NONE',  ( 92.45873412499997812, 110.0000000000000000, -56.18749999590323796 ) ) ;
#26825 = CARTESIAN_POINT ( 'NONE',  ( 96.84719886470459471, 3.152801135295383084, 7.562500001365592084 ) ) ;
#26826 = LINE ( 'NONE', #2313, #27194 ) ;
#26827 = CARTESIAN_POINT ( 'NONE',  ( 96.84719886470459471, -3.152801135295355994, 9.562500001365593860 ) ) ;
#26828 = CARTESIAN_POINT ( 'NONE',  ( 94.33688103937537051, 105.8855032339526758, -52.30000000546237970 ) ) ;
#26829 = VECTOR ( 'NONE', #17787, 1000.000000000000000 ) ;
#26830 = CARTESIAN_POINT ( 'NONE',  ( 101.8468681455907330, 90.74999999863439371, -4.458734124999994997 ) ) ;
#26831 = CARTESIAN_POINT ( 'NONE',  ( 99.99999999999998579, 95.00000000000000000, -6.938893903907228378E-15 ) ) ;
#26832 = CARTESIAN_POINT ( 'NONE',  ( 93.46109445667489979, 105.2492070361643215, -53.42499999726882720 ) ) ;
#26833 = CARTESIAN_POINT ( 'NONE',  ( -13.14518615778179900, 31.97109375108393436, -5.444914386472297529 ) ) ;
#26834 = EDGE_LOOP ( 'NONE', ( #17821, #27127, #9710, #1870 ) ) ;
#26835 = CARTESIAN_POINT ( 'NONE',  ( -5.622872871577965448, 37.97382812499999716, 13.57481594606295161 ) ) ;
#26836 = CARTESIAN_POINT ( 'NONE',  ( -5.622872871577920151, 36.08867187500000284, -13.57481594606300135 ) ) ;
#26837 = CARTESIAN_POINT ( 'NONE',  ( 195.0000000000000000, 36.78320312608393294, 13.14518615778179544 ) ) ;
#26838 = ORIENTED_EDGE ( 'NONE', *, *, #5660, .F. ) ;
#26839 = CARTESIAN_POINT ( 'NONE',  ( 194.2802394038907323, 53.51499872091920906, -14.99999999999999645 ) ) ;
#26840 = CARTESIAN_POINT ( 'NONE',  ( 99.99999999999995737, -4.458734124999988779, 9.937500001365593860 ) ) ;
#26841 = ORIENTED_EDGE ( 'NONE', *, *, #21090, .T. ) ;
#26842 = CARTESIAN_POINT ( 'NONE',  ( 102.4976396683250925, 102.3130555110000159, -50.77500000273119696 ) ) ;
#26843 = CARTESIAN_POINT ( 'NONE',  ( 13.14518615778179900, 36.93203125108394147, 5.444914386472293977 ) ) ;
#26844 = AXIS2_PLACEMENT_3D ( 'NONE', #8635, #24028, #23608 ) ;
#26845 = CARTESIAN_POINT ( 'NONE',  ( 97.50000000000000000, 123.4500000000000028, 1.035533905932725096 ) ) ;
#26846 = CARTESIAN_POINT ( 'NONE',  ( 130.0000000000000000, 40.00781250000000000, -13.57481594606304576 ) ) ;
#26847 = STYLED_ITEM ( 'NONE', ( #5508 ), #7448 ) ;
#26848 = CARTESIAN_POINT ( 'NONE',  ( 116.8548138422182205, 36.58476562608393579, 0.000000000000000000 ) ) ;
#26849 = CARTESIAN_POINT ( 'NONE',  ( -13.14518615778179189, 39.21406250108392300, 5.444914386472304635 ) ) ;
#26850 = CARTESIAN_POINT ( 'NONE',  ( -13.14518615778179544, 34.20351562608393436, 0.000000000000000000 ) ) ;
#26851 =( BOUNDED_CURVE ( )  B_SPLINE_CURVE ( 2, ( #21871, #19301, #11004, #17151, #21584, #28000, #26281, #17576, #21731 ),
 .UNSPECIFIED., .F., .F. ) 
 B_SPLINE_CURVE_WITH_KNOTS ( ( 3, 2, 2, 2, 3 ),
 ( 0.2708333333333330928, 0.2812499999999998890, 0.2916666666666666852, 0.3020833333333334259, 0.3125000000000002220 ),
 .UNSPECIFIED. ) 
 CURVE ( )  GEOMETRIC_REPRESENTATION_ITEM ( )  RATIONAL_B_SPLINE_CURVE ( ( 1.000000000000001554, 0.9238795325112850731, 1.000000000000000000, 0.9238795325112867385, 1.000000000000000000, 0.9238795325112867385, 1.000000000000000000, 0.9238795325112850731, 1.000000000000001554 ) ) 
 REPRESENTATION_ITEM ( '' )  );
#26852 = CARTESIAN_POINT ( 'NONE',  ( 103.1528011352953484, 91.68749999863440792, -3.152801135295366208 ) ) ;
#26853 = CARTESIAN_POINT ( 'NONE',  ( -5.622872871577804688, 36.48554687716787726, 13.57481594606311504 ) ) ;
#26854 = CARTESIAN_POINT ( 'NONE',  ( 102.4976396683250925, 102.3130555110000159, -52.77500000273119696 ) ) ;
#26855 = CARTESIAN_POINT ( 'NONE',  ( 181.4251840539369596, 39.46210937499999005, 5.622872871577880183 ) ) ;
#26856 = ORIENTED_EDGE ( 'NONE', *, *, #9121, .T. ) ;
#26857 = CARTESIAN_POINT ( 'NONE',  ( 74.43200616963319760, 36.00000000000000000, 9.391769196591081226 ) ) ;
#26858 = EDGE_LOOP ( 'NONE', ( #3282, #13467, #16952, #8102 ) ) ;
#26859 = CARTESIAN_POINT ( 'NONE',  ( -8.049105076161786076E-16, 34.99726562608393721, -13.14518615778179544 ) ) ;
#26860 = CARTESIAN_POINT ( 'NONE',  ( 98.15313185440923860, -4.458734124999987891, 5.875000001365592084 ) ) ;
#26861 = CARTESIAN_POINT ( 'NONE',  ( 70.44491438647229131, 36.33671875108393579, -13.14518615778179722 ) ) ;
#26862 = CARTESIAN_POINT ( 'NONE',  ( 101.0355339059327378, 124.7500000000000284, -2.499999999999988010 ) ) ;
#26863 = CARTESIAN_POINT ( 'NONE',  ( 195.0000000000000000, 36.38632812608393152, -13.14518615778179544 ) ) ;
#26864 = CARTESIAN_POINT ( 'NONE',  ( 5.444914386472297529, 34.15390625108393863, -13.14518615778179722 ) ) ;
#26865 = ADVANCED_FACE ( 'NONE', ( #9157 ), #21885, .T. ) ;
#26866 = CARTESIAN_POINT ( 'NONE',  ( 101.7677669529663547, 122.4000000021849530, -1.767766952966370209 ) ) ;
#26867 = CARTESIAN_POINT ( 'NONE',  ( -5.622872871577920151, 36.38632812499999858, 13.57481594606300135 ) ) ;
#26868 = CARTESIAN_POINT ( 'NONE',  ( 200.4449143864723055, 37.32890625108393579, -13.14518615778179722 ) ) ;
#26869 = CARTESIAN_POINT ( 'NONE',  ( 91.91746824999997045, 107.3738262389971538, -51.77499999726881441 ) ) ;
#26870 = ORIENTED_EDGE ( 'NONE', *, *, #20317, .F. ) ;
#26871 = CARTESIAN_POINT ( 'NONE',  ( 13.57481594606304576, 35.04687499999999289, -1.662435489736055892E-15 ) ) ;
#26872 = CARTESIAN_POINT ( 'NONE',  ( 5.444914386472302859, 35.24531250108393010, 13.14518615778179189 ) ) ;
#26873 = EDGE_LOOP ( 'NONE', ( #11722, #7751, #10589, #23390 ) ) ;
#26874 = CARTESIAN_POINT ( 'NONE',  ( 133.7556399192858976, 31.78804746655075419, -13.14518615778179544 ) ) ;
#26875 = CARTESIAN_POINT ( 'NONE',  ( 6.944423797152706079, 31.55306878032414986, -11.16113333171310451 ) ) ;
#26876 = ORIENTED_EDGE ( 'NONE', *, *, #18574, .T. ) ;
#26877 = CARTESIAN_POINT ( 'NONE',  ( 185.7049497278729575, 32.91367187608393152, 9.295050272127047819 ) ) ;
#26878 = ORIENTED_EDGE ( 'NONE', *, *, #9818, .T. ) ;
#26879 = CARTESIAN_POINT ( 'NONE',  ( 102.0669872999999797, 123.3500000010924680, -9.794112055954760458E-15 ) ) ;
#26880 = CARTESIAN_POINT ( 'NONE',  ( 9.180175813647991845, 55.00000000000000000, -15.00000000000000000 ) ) ;
#26881 = CARTESIAN_POINT ( 'NONE',  ( 102.4999999999999858, 123.8500000021849416, 1.035533905932722876 ) ) ;
#26882 = CARTESIAN_POINT ( 'NONE',  ( 135.6228728715778971, 38.96601562716787015, 13.57481594606304576 ) ) ;
#26883 = CARTESIAN_POINT ( 'NONE',  ( 95.00472066334981491, 116.8754121666685393, -49.42500000273118843 ) ) ;
#26884 =( BOUNDED_CURVE ( )  B_SPLINE_CURVE ( 2, ( #17882, #24297, #651, #20028, #11306, #18020, #2918, #14015, #24583 ),
 .UNSPECIFIED., .F., .T. ) 
 B_SPLINE_CURVE_WITH_KNOTS ( ( 3, 2, 2, 2, 3 ),
 ( 0.2142857142857142183, 0.2232142857142856707, 0.2321428571428570953, 0.2410714285714285199, 0.2499999999999999445 ),
 .UNSPECIFIED. ) 
 CURVE ( )  GEOMETRIC_REPRESENTATION_ITEM ( )  RATIONAL_B_SPLINE_CURVE ( ( 1.000000000000000444, 0.9238795325112862944, 1.000000000000000000, 0.9238795325112867385, 1.000000000000000000, 0.9238795325112867385, 1.000000000000000000, 0.9238795325112871826, 0.9999999999999995559 ) ) 
 REPRESENTATION_ITEM ( '' )  );
#26885 = LINE ( 'NONE', #16019, #21500 ) ;
#26886 = DIRECTION ( 'NONE',  ( -1.000000000000000000, 0.000000000000000000, 0.000000000000000000 ) ) ;
#26887 = CARTESIAN_POINT ( 'NONE',  ( 208.1451861577817795, 40.30546875108393579, 5.444914386472293977 ) ) ;
#26888 = CARTESIAN_POINT ( 'NONE',  ( 98.15313185440925281, -4.458734124999987891, 6.625000001365592084 ) ) ;
#26889 = ORIENTED_EDGE ( 'NONE', *, *, #14429, .T. ) ;
#26890 = CARTESIAN_POINT ( 'NONE',  ( -9.078091922698781957, 36.00000000000000711, -9.794392408849049048 ) ) ;
#26891 = CARTESIAN_POINT ( 'NONE',  ( 95.54126587499995082, -1.846868145590724986, 7.500000001365592084 ) ) ;
#26892 = CARTESIAN_POINT ( 'NONE',  ( 5.444914386472302859, 36.83281250108392868, 13.14518615778179189 ) ) ;
#26893 = CARTESIAN_POINT ( 'NONE',  ( -9.713547494049105779, 35.99999999999998579, 8.898183052316493757 ) ) ;
#26894 = DIRECTION ( 'NONE',  ( -2.385244779468110248E-16, 0.000000000000000000, -1.000000000000000000 ) ) ;
#26895 = CARTESIAN_POINT ( 'NONE',  ( 97.92893218813451028, -4.999999999999989342, 5.187500000000000000 ) ) ;
#26896 = CARTESIAN_POINT ( 'NONE',  ( 97.50236033167492167, 102.3130555110000159, -44.72500000273119980 ) ) ;
#26897 = LINE ( 'NONE', #1239, #15936 ) ;
#26898 = CARTESIAN_POINT ( 'NONE',  ( 104.3262379212492448, 115.9545556584642867, -53.19999999453762740 ) ) ;
#26899 = PLANE ( 'NONE',  #18610 ) ;
#26900 = CARTESIAN_POINT ( 'NONE',  ( 143.5748159460630688, 40.55351562499999574, 5.622872871577868636 ) ) ;
#26901 = CARTESIAN_POINT ( 'NONE',  ( 143.5748159460630404, 33.40976562499999858, 5.622872871577869525 ) ) ;
#26902 = VERTEX_POINT ( 'NONE', #18672 ) ;
#26903 = CYLINDRICAL_SURFACE ( 'NONE', #18134, 4.999999999999999112 ) ;
#26904 = EDGE_CURVE ( 'NONE', #15733, #26226, #18161, .T. ) ;
#26905 = CARTESIAN_POINT ( 'NONE',  ( -13.14518615778179544, 34.40195312608393152, 0.000000000000000000 ) ) ;
#26906 = CARTESIAN_POINT ( 'NONE',  ( -9.598844408820458085, 34.65000000216787868, -9.598844408820458085 ) ) ;
#26907 = CARTESIAN_POINT ( 'NONE',  ( 103.5355339059327093, 3.535533905932755072, 8.750000002731184168 ) ) ;
#26908 = CARTESIAN_POINT ( 'NONE',  ( 135.4449143864723055, 32.86406250108392868, 13.14518615778179189 ) ) ;
#26909 = CARTESIAN_POINT ( 'NONE',  ( 78.14518615778179367, 38.51953125108393294, 5.444914386472293977 ) ) ;
#26910 = ORIENTED_EDGE ( 'NONE', *, *, #8481, .F. ) ;
#26911 = LINE ( 'NONE', #542, #9768 ) ;
#26912 = CARTESIAN_POINT ( 'NONE',  ( 13.14518615778179900, 38.61875000108393152, -5.444914386472297529 ) ) ;
#26913 = CARTESIAN_POINT ( 'NONE',  ( 9.295050272127047819, 33.11210937608393579, 9.295050272127046043 ) ) ;
#26914 = CARTESIAN_POINT ( 'NONE',  ( 101.0355339059327093, 124.0500000021849445, -2.500000000000002665 ) ) ;
#26915 = CARTESIAN_POINT ( 'NONE',  ( 106.5389055433250860, 114.7507929638356785, -54.67499999726882720 ) ) ;
#26916 = AXIS2_PLACEMENT_3D ( 'NONE', #19741, #11031, #13446 ) ;
#26917 = CARTESIAN_POINT ( 'NONE',  ( -13.57481594606304576, 39.56132812716787583, 5.622872871577880183 ) ) ;
#26918 = CARTESIAN_POINT ( 'NONE',  ( 103.5355339059327093, 82.50000000273119838, 3.535533905932726206 ) ) ;
#26919 = CARTESIAN_POINT ( 'NONE',  ( 195.0000000000000000, -7.395377635281828788, -2.255140518769849538E-14 ) ) ;
#26920 = CARTESIAN_POINT ( 'NONE',  ( 92.99999999999998579, 110.0000000000000000, -53.00000000000001421 ) ) ;
#26921 = CARTESIAN_POINT ( 'NONE',  ( 116.9040934463640156, 36.00000000000000000, 1.137167824541468031 ) ) ;
#26922 = CARTESIAN_POINT ( 'NONE',  ( 133.6286142932849259, 36.00000000000002132, -13.08307257738123219 ) ) ;
#26923 = EDGE_CURVE ( 'NONE', #13869, #18001, #14944, .T. ) ;
#26924 = FACE_OUTER_BOUND ( 'NONE', #11566, .T. ) ;
#26925 = CARTESIAN_POINT ( 'NONE',  ( 102.4999999999999858, 123.1500000021849672, -1.035533905932742638 ) ) ;
#26926 = CARTESIAN_POINT ( 'NONE',  ( -9.598844408820454532, 33.95546874999999432, 9.598844408820459861 ) ) ;
#26927 = CARTESIAN_POINT ( 'NONE',  ( 99.99999999999998579, 128.0000000000000000, -2.500000000000013767 ) ) ;
#26928 = CARTESIAN_POINT ( 'NONE',  ( -9.295050272127046043, 33.50898437608393010, -9.295050272127046043 ) ) ;
#26929 = CARTESIAN_POINT ( 'NONE',  ( -13.14518615778179900, 34.15390625108393863, -5.444914386472297529 ) ) ;
#26930 = CARTESIAN_POINT ( 'NONE',  ( -8.312177448680279460E-16, 33.75703125216787726, -13.57481594606304576 ) ) ;
#26931 = CARTESIAN_POINT ( 'NONE',  ( -13.57481594606304576, 37.18007812716787441, 5.622872871577880183 ) ) ;
#26932 = EDGE_CURVE ( 'NONE', #23574, #12833, #4928, .T. ) ;
#26933 = CARTESIAN_POINT ( 'NONE',  ( 94.99999999999997158, -2.071067811865486608, 4.187500002731185944 ) ) ;
#26934 = CARTESIAN_POINT ( 'NONE',  ( 99.99999999999995737, 82.18750000136559208, -4.458734125000016313 ) ) ;
#26935 = CARTESIAN_POINT ( 'NONE',  ( 51.85481384221819923, 32.56640625108394005, -5.444914386472297529 ) ) ;
#26936 = CARTESIAN_POINT ( 'NONE',  ( 95.00000000000000000, 90.43750000000000000, -2.071067811865479058 ) ) ;
#26937 = CARTESIAN_POINT ( 'NONE',  ( 98.38094258238263023, 122.9999999999999716, 1.910582039389197684 ) ) ;
#26938 = EDGE_CURVE ( 'NONE', #10403, #26695, #22215, .T. ) ;
#26939 = CARTESIAN_POINT ( 'NONE',  ( 2.493653234604083739E-15, 37.22968749999999716, 13.57481594606304576 ) ) ;
#26940 = CARTESIAN_POINT ( 'NONE',  ( 130.0000000000000000, 34.60039062608393579, 13.14518615778179544 ) ) ;
#26941 = ORIENTED_EDGE ( 'NONE', *, *, #1016, .T. ) ;
#26942 = CARTESIAN_POINT ( 'NONE',  ( 99.99999999999995737, 80.75000000000000000, -5.000000000000018652 ) ) ;
#26943 = EDGE_CURVE ( 'NONE', #24277, #17678, #25123, .T. ) ;
#26944 = CARTESIAN_POINT ( 'NONE',  ( 104.3262379212492448, 115.9545556584642867, -47.70000000000000995 ) ) ;
#26945 = CARTESIAN_POINT ( 'NONE',  ( 96.84719886470459471, 84.31250000136560629, -3.152801135295383084 ) ) ;
#26946 = CARTESIAN_POINT ( 'NONE',  ( 102.0710678118654613, 93.81250000000000000, 4.999999999999983125 ) ) ;
#26947 = CARTESIAN_POINT ( 'NONE',  ( 116.4251840539369738, 38.66835937499999432, 5.622872871577880183 ) ) ;
#26948 = EDGE_CURVE ( 'NONE', #12117, #1457, #17745, .T. ) ;
#26949 = CARTESIAN_POINT ( 'NONE',  ( 93.46109445667489979, 105.2492070361643215, -47.42499999726882720 ) ) ;
#26950 = CARTESIAN_POINT ( 'NONE',  ( 74.59884440882045453, 39.71015624999999716, 9.598844408820456309 ) ) ;
#26951 = CARTESIAN_POINT ( 'NONE',  ( 13.57481594606304931, 37.47773437716787726, 5.622872871577869525 ) ) ;
#26952 = EDGE_LOOP ( 'NONE', ( #3145, #26127, #22976, #14296, #9774, #1208, #21630, #1454, #24447, #22984, #17881, #9756, #4225, #9958 ) ) ;
#26953 = CARTESIAN_POINT ( 'NONE',  ( 184.4540428948961335, 35.99999999999997868, -8.172591786207139108 ) ) ;
#26954 = CARTESIAN_POINT ( 'NONE',  ( 97.92893218813451028, 5.000000000000018652, 14.81249999999999822 ) ) ;
#26955 = EDGE_CURVE ( 'NONE', #13505, #11663, #23609, .T. ) ;
#26956 = ORIENTED_EDGE ( 'NONE', *, *, #2185, .T. ) ;
#26957 = CARTESIAN_POINT ( 'NONE',  ( 9.295050272127047819, 37.08085937608393579, 9.295050272127046043 ) ) ;
#26958 = CARTESIAN_POINT ( 'NONE',  ( 195.0000000000000000, 39.95820312608393010, 13.14518615778179544 ) ) ;
#26959 = CARTESIAN_POINT ( 'NONE',  ( -13.14518615778179544, 33.40976562608393863, 0.000000000000000000 ) ) ;
#26960 = CARTESIAN_POINT ( 'NONE',  ( 104.9999999999999574, 2.071067811865491937, 12.68750000273118772 ) ) ;
#26961 = DIRECTION ( 'NONE',  ( 0.000000000000000000, 0.000000000000000000, 1.000000000000000000 ) ) ;
#26962 = CARTESIAN_POINT ( 'NONE',  ( -8.049105076161786076E-16, 34.20351562608394147, -13.14518615778179544 ) ) ;
#26963 = CARTESIAN_POINT ( 'NONE',  ( 135.4449143864723055, 33.16171875108393152, -13.14518615778179900 ) ) ;
#26964 = CARTESIAN_POINT ( 'NONE',  ( 98.15313185440923860, 90.62499999863439371, -4.458734124999994997 ) ) ;
#26965 = DIRECTION ( 'NONE',  ( -1.000000000000000000, 0.000000000000000000, 0.000000000000000000 ) ) ;
#26966 = DIRECTION ( 'NONE',  ( 0.000000000000000000, 0.000000000000000000, 1.000000000000000000 ) ) ;
#26967 = CARTESIAN_POINT ( 'NONE',  ( 78.57481594606305464, 36.73359375216787015, -1.662435489736055892E-15 ) ) ;
#26968 = CARTESIAN_POINT ( 'NONE',  ( 104.4587341249999781, -1.846868145590721655, 5.125000001365592972 ) ) ;
#26969 = CARTESIAN_POINT ( 'NONE',  ( 94.33688103937537051, 114.1144967660473242, -52.70000000546237828 ) ) ;
#26970 = CARTESIAN_POINT ( 'NONE',  ( 103.1528011352953342, -3.152801135295355106, 11.81250000136559208 ) ) ;
#26971 = CARTESIAN_POINT ( 'NONE',  ( 95.00472066334982912, 116.8754121666685393, -47.42500000273118843 ) ) ;
#26972 = CARTESIAN_POINT ( 'NONE',  ( 104.9999999999999716, 1.449011120738813565E-14, 3.499999999999999556 ) ) ;
#26973 = FACE_OUTER_BOUND ( 'NONE', #7310, .T. ) ;
#26974 = CARTESIAN_POINT ( 'NONE',  ( 13.14518615778179544, 32.41757812608393863, -1.609821015232357215E-15 ) ) ;
#26975 = VERTEX_POINT ( 'NONE', #4783 ) ;
#26976 = CARTESIAN_POINT ( 'NONE',  ( 195.0000000000000000, -7.395377635281828788, -13.57481594606306707 ) ) ;
#26977 =( BOUNDED_CURVE ( )  B_SPLINE_CURVE ( 2, ( #3571, #27380, #20819, #8246, #23233, #5577, #16934, #1578, #25634 ),
 .UNSPECIFIED., .F., .F. ) 
 B_SPLINE_CURVE_WITH_KNOTS ( ( 3, 2, 2, 2, 3 ),
 ( 0.2499999999999999445, 0.2589285714285713969, 0.2678571428571427937, 0.2767857142857143016, 0.2857142857142856984 ),
 .UNSPECIFIED. ) 
 CURVE ( )  GEOMETRIC_REPRESENTATION_ITEM ( )  RATIONAL_B_SPLINE_CURVE ( ( 1.000000000000000444, 0.9238795325112862944, 1.000000000000000000, 0.9238795325112867385, 1.000000000000000000, 0.9238795325112867385, 1.000000000000000000, 0.9238795325112867385, 1.000000000000000000 ) ) 
 REPRESENTATION_ITEM ( '' )  );
#26978 = CARTESIAN_POINT ( 'NONE',  ( 13.57481594606304576, 39.90859375216787441, -1.662435489736055892E-15 ) ) ;
#26979 = DIRECTION ( 'NONE',  ( -0.000000000000000000, -1.000000000000000000, -0.000000000000000000 ) ) ;
#26980 = ADVANCED_FACE ( 'NONE', ( #26154 ), #23878, .T. ) ;
#26981 = CARTESIAN_POINT ( 'NONE',  ( 204.2950502721270425, 37.08085937608393579, -9.295050272127046043 ) ) ;
#26982 = ORIENTED_EDGE ( 'NONE', *, *, #12095, .F. ) ;
#26983 = CARTESIAN_POINT ( 'NONE',  ( -5.622872871577804688, 37.18007812499999432, 13.57481594606311504 ) ) ;
#26984 = CARTESIAN_POINT ( 'NONE',  ( 95.54126587499996504, 1.387778780781445676E-14, 9.687500001365593860 ) ) ;
#26985 = ORIENTED_EDGE ( 'NONE', *, *, #14200, .F. ) ;
#26986 = CARTESIAN_POINT ( 'NONE',  ( 94.33688103937537051, 105.8855032339526758, -45.80000000000000426 ) ) ;
#26987 = CARTESIAN_POINT ( 'NONE',  ( 13.14518615778179900, 37.03125000108393294, -5.444914386472297529 ) ) ;
#26988 = CARTESIAN_POINT ( 'NONE',  ( 99.99999999999998579, 123.6000000000000085, 2.499999999999978684 ) ) ;
#26989 = CARTESIAN_POINT ( 'NONE',  ( 98.96446609406724804, 123.2499999999999716, -2.499999999999993339 ) ) ;
#26990 = CARTESIAN_POINT ( 'NONE',  ( 130.0000000000000000, 38.37070312608393152, 13.14518615778179544 ) ) ;
#26991 = CARTESIAN_POINT ( 'NONE',  ( 9.295050272127046043, 38.07304687608393579, -9.295050272127046043 ) ) ;
#26992 = CARTESIAN_POINT ( 'NONE',  ( -5.444914386472299306, 36.73359375108393010, 13.14518615778179722 ) ) ;
#26993 = CARTESIAN_POINT ( 'NONE',  ( 96.84719886470463734, 90.93749999863440792, -3.152801135295366208 ) ) ;
#26994 = CARTESIAN_POINT ( 'NONE',  ( 64.27612806197501527, 53.51529642094997996, -14.99999999999999822 ) ) ;
#26995 = CARTESIAN_POINT ( 'NONE',  ( 102.4976396683250925, 102.3130555110000159, -48.77500000273119696 ) ) ;
#26996 = AXIS2_PLACEMENT_3D ( 'NONE', #9329, #9194, #17888 ) ;
#26997 = CARTESIAN_POINT ( 'NONE',  ( -13.57481594606304398, 37.18007812716787441, 5.622872871577880183 ) ) ;
#26998 = CARTESIAN_POINT ( 'NONE',  ( -13.14518615778179544, 35.98945312608393721, 0.000000000000000000 ) ) ;
#26999 = CARTESIAN_POINT ( 'NONE',  ( 101.8468681455907046, -4.458734124999987891, 6.000000001365592084 ) ) ;
#27000 = CARTESIAN_POINT ( 'NONE',  ( 78.14518615778179367, 36.98164062608393010, -1.609821015232357215E-15 ) ) ;
#27001 = PRODUCT_DEFINITION_SHAPE ( 'NONE', 'NONE',  #28207 ) ;
#27002 = CARTESIAN_POINT ( 'NONE',  ( 101.7677669529663547, 124.7000000000000028, -1.767766952966370209 ) ) ;
#27003 = CARTESIAN_POINT ( 'NONE',  ( -15.00000000000000355, 75.00000000000000000, -9.999999999999998224 ) ) ;
#27004 = ORIENTED_EDGE ( 'NONE', *, *, #3075, .F. ) ;
#27005 = CARTESIAN_POINT ( 'NONE',  ( 9.295050272127046043, 34.10429687608393579, -9.295050272127046043 ) ) ;
#27006 = CARTESIAN_POINT ( 'NONE',  ( 102.0669872999999939, 122.6000000010924964, -0.8561741729129507261 ) ) ;
#27007 = CARTESIAN_POINT ( 'NONE',  ( 103.1528011352953484, 92.43749999863440792, 3.152801135295352886 ) ) ;
#27008 = CARTESIAN_POINT ( 'NONE',  ( 208.1451861577818079, 37.13046875108393863, 5.444914386472293977 ) ) ;
#27009 = CARTESIAN_POINT ( 'NONE',  ( 93.46109445667489979, 114.7507929638356785, -52.07499999726881867 ) ) ;
#27010 = VERTEX_POINT ( 'NONE', #4356 ) ;
#27011 = CARTESIAN_POINT ( 'NONE',  ( 5.622872871577871301, 32.81445312499999289, -13.57481594606304753 ) ) ;
#27012 = CARTESIAN_POINT ( 'NONE',  ( -13.14518615778179544, 34.99726562608393721, 0.000000000000000000 ) ) ;
#27013 = ORIENTED_EDGE ( 'NONE', *, *, #19102, .F. ) ;
#27014 = CARTESIAN_POINT ( 'NONE',  ( 120.7049497278729575, 31.92148437608393508, -9.295050272127046043 ) ) ;
#27015 = CARTESIAN_POINT ( 'NONE',  ( 78.14518615778180788, 40.30546875108393579, 5.444914386472293977 ) ) ;
#27016 = CYLINDRICAL_SURFACE ( 'NONE', #19152, 11.57481594606304398 ) ;
#27017 = VECTOR ( 'NONE', #8443, 1000.000000000000000 ) ;
#27018 = CARTESIAN_POINT ( 'NONE',  ( 181.8548138422181921, 34.45156250108394147, 5.444914386472304635 ) ) ;
#27019 =( BOUNDED_CURVE ( )  B_SPLINE_CURVE ( 2, ( #6694, #24376, #2727, #10821, #26092, #4293, #161, #6557, #13530 ),
 .UNSPECIFIED., .F., .F. ) 
 B_SPLINE_CURVE_WITH_KNOTS ( ( 3, 2, 2, 2, 3 ),
 ( 0.02083333333333358892, 0.03125000000000020123, 0.04166666666666681007, 0.05208333333333342585, 0.06250000000000004163 ),
 .UNSPECIFIED. ) 
 CURVE ( )  GEOMETRIC_REPRESENTATION_ITEM ( )  RATIONAL_B_SPLINE_CURVE ( ( 0.9999999999999981126, 0.9238795325112886259, 1.000000000000000000, 0.9238795325112867385, 1.000000000000000000, 0.9238795325112867385, 1.000000000000000000, 0.9238795325112864054, 1.000000000000000222 ) ) 
 REPRESENTATION_ITEM ( '' )  );
#27020 = VERTEX_POINT ( 'NONE', #26735 ) ;
#27021 = CARTESIAN_POINT ( 'NONE',  ( 65.00000000000000000, 37.62656249999999858, -13.57481594606304576 ) ) ;
#27022 = CARTESIAN_POINT ( 'NONE',  ( 99.99999999999998579, 91.12499999726880162, -4.999999999999997335 ) ) ;
#27023 = DIRECTION ( 'NONE',  ( -0.000000000000000000, -0.000000000000000000, -1.000000000000000000 ) ) ;
#27024 = CARTESIAN_POINT ( 'NONE',  ( 139.5988444088204403, 38.42031250216787441, -9.598844408820458085 ) ) ;
#27025 = CARTESIAN_POINT ( 'NONE',  ( 102.4976396683250925, 117.6869444889999841, -45.72500000273119269 ) ) ;
#27026 = CARTESIAN_POINT ( 'NONE',  ( 84.99999999999998579, 95.00000000000000000, 14.99999999999999467 ) ) ;
#27027 = CARTESIAN_POINT ( 'NONE',  ( 71.41286667625729478, 50.00000000108468612, 11.99502265407483570 ) ) ;
#27028 = ORIENTED_EDGE ( 'NONE', *, *, #8879, .F. ) ;
#27029 = VERTEX_POINT ( 'NONE', #82 ) ;
#27030 = SURFACE_SIDE_STYLE ('',( #14169 ) ) ;
#27031 = CARTESIAN_POINT ( 'NONE',  ( 96.84719886470459471, -3.152801135295355994, 4.562500001365592084 ) ) ;
#27032 = ORIENTED_EDGE ( 'NONE', *, *, #23377, .F. ) ;
#27033 = CARTESIAN_POINT ( 'NONE',  ( 3.628614293284873948, 36.00000000000000711, -13.08307257738123219 ) ) ;
#27034 = CARTESIAN_POINT ( 'NONE',  ( 95.54126587499996504, 1.387778780781445676E-14, 9.437500001365593860 ) ) ;
#27035 = DIRECTION ( 'NONE',  ( 5.782411586589357392E-17, -0.000000000000000000, 1.000000000000000000 ) ) ;
#27036 = CARTESIAN_POINT ( 'NONE',  ( 181.4251840539369596, 40.25585937716787299, -5.622872871577872189 ) ) ;
#27037 = AXIS2_PLACEMENT_3D ( 'NONE', #7080, #15776, #24482 ) ;
#27038 = CARTESIAN_POINT ( 'NONE',  ( 104.9999999999999716, 91.81249999726880162, 2.071067811865467956 ) ) ;
#27039 = CARTESIAN_POINT ( 'NONE',  ( 104.9952793366501851, 103.1245878333314323, -48.42500000273120264 ) ) ;
#27040 = CARTESIAN_POINT ( 'NONE',  ( -13.57481594606304576, 38.61874999999999147, 0.000000000000000000 ) ) ;
#27041 = FACE_OUTER_BOUND ( 'NONE', #8508, .T. ) ;
#27042 = CARTESIAN_POINT ( 'NONE',  ( 2.276146844546785175, 51.46995505939283788, 15.00000000000000178 ) ) ;
#27043 = SPHERICAL_SURFACE ( 'NONE', #1956, 5.000000000000000000 ) ;
#27044 = CARTESIAN_POINT ( 'NONE',  ( 139.5988444088204687, 33.36015624999999574, 9.598844408820456309 ) ) ;
#27045 = ORIENTED_EDGE ( 'NONE', *, *, #18240, .T. ) ;
#27046 = CARTESIAN_POINT ( 'NONE',  ( 2.414731522848535132E-15, 33.80664062608393294, 13.14518615778179544 ) ) ;
#27047 = CARTESIAN_POINT ( 'NONE',  ( 13.57481594606304753, 32.81445312716787299, -5.622872871577873077 ) ) ;
#27048 = CARTESIAN_POINT ( 'NONE',  ( 97.92893218813451028, 5.000000000000018652, 4.937500002731185056 ) ) ;
#27049 = CARTESIAN_POINT ( 'NONE',  ( 143.1451861577818079, 32.26875000108393721, -5.444914386472297529 ) ) ;
#27050 = CARTESIAN_POINT ( 'NONE',  ( 78.14518615778179367, 39.41250000108393436, -5.444914386472297529 ) ) ;
#27051 = DIRECTION ( 'NONE',  ( 0.000000000000000000, 0.000000000000000000, 1.000000000000000000 ) ) ;
#27052 = CARTESIAN_POINT ( 'NONE',  ( -9.295050272127046043, 38.07304687608393579, -9.295050272127046043 ) ) ;
#27053 = CARTESIAN_POINT ( 'NONE',  ( -5.444914386472297529, 31.87187500108393223, -13.14518615778179722 ) ) ;
#27054 = CARTESIAN_POINT ( 'NONE',  ( 2.493653234604083739E-15, 36.53515625216787299, 13.57481594606304576 ) ) ;
#27055 = PRODUCT_DEFINITION ( 'UNKNOWN', '', #19955, #3511 ) ;
#27056 = CARTESIAN_POINT ( 'NONE',  ( 97.50236033167490746, 102.3130555110000159, -55.47499999726881725 ) ) ;
#27057 = EDGE_CURVE ( 'NONE', #25242, #20160, #21752, .T. ) ;
#27058 = CARTESIAN_POINT ( 'NONE',  ( -5.622872871577873077, 39.36289062716787157, -13.57481594606304753 ) ) ;
#27059 = CARTESIAN_POINT ( 'NONE',  ( 208.1451861577818079, 32.21914062608393436, -1.609821015232357215E-15 ) ) ;
#27060 = FACE_OUTER_BOUND ( 'NONE', #21739, .T. ) ;
#27061 = CARTESIAN_POINT ( 'NONE',  ( 102.4999999999999716, 123.8569999999781572, -1.035533905932742638 ) ) ;
#27062 = DIRECTION ( 'NONE',  ( 0.000000000000000000, 0.000000000000000000, -1.000000000000000000 ) ) ;
#27063 = CARTESIAN_POINT ( 'NONE',  ( 181.4251840539369596, 39.41249999999999432, 0.000000000000000000 ) ) ;
#27064 = CARTESIAN_POINT ( 'NONE',  ( 7.171391216998964424, 31.99955315621561525, -11.52591757658528948 ) ) ;
#27065 = CARTESIAN_POINT ( 'NONE',  ( 200.6228728715777549, 38.96601562716787015, 13.57481594606318076 ) ) ;
#27066 = CARTESIAN_POINT ( 'NONE',  ( -5.622872871577873077, 34.50117187499999005, -13.57481594606304753 ) ) ;
#27067 = CARTESIAN_POINT ( 'NONE',  ( -2.892062521303301548, 36.00000000000000711, -13.15766692561478024 ) ) ;
#27068 = CARTESIAN_POINT ( 'NONE',  ( 9.295050272127047819, 34.69960937608393436, 9.295050272127046043 ) ) ;
#27069 = CARTESIAN_POINT ( 'NONE',  ( 9.295050272127047819, 33.70742187608393436, 9.295050272127046043 ) ) ;
#27070 = CARTESIAN_POINT ( 'NONE',  ( 5.444914386472302859, 34.45156250108392726, 13.14518615778179189 ) ) ;
#27071 = CARTESIAN_POINT ( 'NONE',  ( 13.57481594606304753, 35.98945312716787015, -5.622872871577873077 ) ) ;
#27072 = CARTESIAN_POINT ( 'NONE',  ( 0.000000000000000000, 36.00000000000000000, -13.57481594606304576 ) ) ;
#27073 = CARTESIAN_POINT ( 'NONE',  ( 59.55508561352770158, 33.26093750108393721, -13.14518615778179900 ) ) ;
#27074 = DIRECTION ( 'NONE',  ( -0.000000000000000000, 1.000000000000000000, -0.000000000000000000 ) ) ;
#27075 = DIRECTION ( 'NONE',  ( 0.000000000000000000, 0.000000000000000000, -1.000000000000000000 ) ) ;
#27076 = FACE_OUTER_BOUND ( 'NONE', #21524, .T. ) ;
#27077 = CARTESIAN_POINT ( 'NONE',  ( 3.878385297391210518, 32.03609435653363136, -13.57481594606304576 ) ) ;
#27078 = CARTESIAN_POINT ( 'NONE',  ( 99.99999999999997158, 101.5015231886685854, -53.37499999726883004 ) ) ;
#27079 = CARTESIAN_POINT ( 'NONE',  ( 135.4449143864723055, 34.65000000108393863, 13.14518615778179189 ) ) ;
#27080 = VERTEX_POINT ( 'NONE', #2504 ) ;
#27081 = CARTESIAN_POINT ( 'NONE',  ( 104.9999999999999574, 80.43750000000001421, 2.071067811865462627 ) ) ;
#27082 = CARTESIAN_POINT ( 'NONE',  ( 92.99999999999998579, 110.0000000000000000, -47.00000000000001421 ) ) ;
#27083 = CARTESIAN_POINT ( 'NONE',  ( 104.9999999999999716, 79.62500000273119838, -1.449011120738813565E-14 ) ) ;
#27084 = CARTESIAN_POINT ( 'NONE',  ( 95.00000000000000000, 90.56250000000000000, 2.071067811865463959 ) ) ;
#27085 = CARTESIAN_POINT ( 'NONE',  ( 59.37712712842213136, 39.66054687716786731, 13.57481594606304753 ) ) ;
#27086 = ADVANCED_FACE ( 'NONE', ( #2227 ), #12368, .T. ) ;
#27087 = AXIS2_PLACEMENT_3D ( 'NONE', #897, #22407, #15832 ) ;
#27088 = CARTESIAN_POINT ( 'NONE',  ( 108.0825317499999869, 107.3738262389971538, -48.72499999726881015 ) ) ;
#27089 = CARTESIAN_POINT ( 'NONE',  ( 185.7049497278729575, 31.72304687608393081, -9.295050272127046043 ) ) ;
#27090 = DIRECTION ( 'NONE',  ( -0.000000000000000000, -1.000000000000000000, -0.000000000000000000 ) ) ;
#27091 = ORIENTED_EDGE ( 'NONE', *, *, #27721, .T. ) ;
#27092 = FACE_OUTER_BOUND ( 'NONE', #11052, .T. ) ;
#27093 = CARTESIAN_POINT ( 'NONE',  ( 97.92893218813451028, 5.000000000000018652, 8.812499999999998224 ) ) ;
#27094 = ORIENTED_EDGE ( 'NONE', *, *, #22226, .T. ) ;
#27095 = CARTESIAN_POINT ( 'NONE',  ( -8.049105076161786076E-16, 36.58476562608393579, -13.14518615778179544 ) ) ;
#27096 = CARTESIAN_POINT ( 'NONE',  ( 189.3771271284221314, 32.21914062716787441, -13.57481594606304753 ) ) ;
#27097 = ADVANCED_FACE ( 'NONE', ( #9130 ), #13532, .F. ) ;
#27098 = CARTESIAN_POINT ( 'NONE',  ( 2.414731522848535132E-15, 33.60820312608392868, 13.14518615778179544 ) ) ;
#27099 = CARTESIAN_POINT ( 'NONE',  ( 96.46446609406721961, 3.535533905932755072, 12.00000000273118594 ) ) ;
#27100 = CARTESIAN_POINT ( 'NONE',  ( 143.1451861577818079, 40.15664062608393436, -1.609821015232357215E-15 ) ) ;
#27101 = CARTESIAN_POINT ( 'NONE',  ( 98.96446609406724804, 123.3500000021849274, -2.499999999999996447 ) ) ;
#27102 = EDGE_CURVE ( 'NONE', #14776, #19120, #24040, .T. ) ;
#27103 = CARTESIAN_POINT ( 'NONE',  ( 130.0000000000000000, 31.62382812608393579, -13.14518615778179544 ) ) ;
#27104 = CARTESIAN_POINT ( 'NONE',  ( 101.8468681455907330, 92.49999999863440792, -4.458734124999994997 ) ) ;
#27105 = CARTESIAN_POINT ( 'NONE',  ( 97.50000000000000000, 124.9500000000000028, -1.035533905932742416 ) ) ;
#27106 = SHAPE_DEFINITION_REPRESENTATION ( #13044, #2411 ) ;
#27107 = CARTESIAN_POINT ( 'NONE',  ( 13.57481594606304576, 35.93984375216787441, -1.662435489736055892E-15 ) ) ;
#27108 = CARTESIAN_POINT ( 'NONE',  ( 95.54126587499996504, 1.387778780781445676E-14, 5.687500001365591196 ) ) ;
#27109 = CARTESIAN_POINT ( 'NONE',  ( -13.57481594606304398, 37.97382812716787726, 5.622872871577880183 ) ) ;
#27110 = AXIS2_PLACEMENT_3D ( 'NONE', #13762, #24477, #22485 ) ;
#27111 = CARTESIAN_POINT ( 'NONE',  ( 101.8468681455907046, 4.458734125000016313, 12.12500000136559208 ) ) ;
#27112 = CARTESIAN_POINT ( 'NONE',  ( 107.0000000000000142, 112.2744378736303332, -51.40000000546237402 ) ) ;
#27113 = CARTESIAN_POINT ( 'NONE',  ( 99.99999999999998579, 90.81249999863440792, -4.458734124999994997 ) ) ;
#27114 = CARTESIAN_POINT ( 'NONE',  ( 102.0710678118654329, -4.999999999999989342, 4.312499999999999112 ) ) ;
#27115 = CARTESIAN_POINT ( 'NONE',  ( 102.4976396683250783, 117.6869444889999841, -54.22499999726881725 ) ) ;
#27116 = CARTESIAN_POINT ( 'NONE',  ( 5.444914386472297529, 34.15390625108393863, -13.14518615778179900 ) ) ;
#27117 = ADVANCED_FACE ( 'NONE', ( #11394 ), #7407, .F. ) ;
#27118 = ORIENTED_EDGE ( 'NONE', *, *, #1638, .T. ) ;
#27119 = FACE_OUTER_BOUND ( 'NONE', #20376, .T. ) ;
#27120 = PLANE ( 'NONE',  #27087 ) ;
#27121 = LINE ( 'NONE', #9284, #7487 ) ;
#27122 = CARTESIAN_POINT ( 'NONE',  ( 181.8548138422181921, 35.74140625108393721, -5.444914386472297529 ) ) ;
#27123 = ORIENTED_EDGE ( 'NONE', *, *, #3260, .F. ) ;
#27124 = CARTESIAN_POINT ( 'NONE',  ( 198.8639252651224467, 54.10645156200647676, -14.99999999999999645 ) ) ;
#27125 = CARTESIAN_POINT ( 'NONE',  ( 104.4587341249999639, 1.442382525525748735E-14, 10.18750000136559208 ) ) ;
#27126 = ADVANCED_FACE ( 'NONE', ( #18106, #7266 ), #15956, .T. ) ;
#27127 = ORIENTED_EDGE ( 'NONE', *, *, #18490, .T. ) ;
#27128 = CARTESIAN_POINT ( 'NONE',  ( 99.99999999999998579, 118.4984768113314004, -45.87500000273118417 ) ) ;
#27129 = AXIS2_PLACEMENT_3D ( 'NONE', #8980, #26378, #2952 ) ;
#27130 = CARTESIAN_POINT ( 'NONE',  ( -13.14518615778179189, 35.84062500108394289, 5.444914386472304635 ) ) ;
#27131 = DIRECTION ( 'NONE',  ( -0.000000000000000000, 1.000000000000000000, -0.000000000000000000 ) ) ;
#27132 = CARTESIAN_POINT ( 'NONE',  ( 100.0000000000000000, 110.0000000000000000, -55.00000000000000711 ) ) ;
#27133 = CARTESIAN_POINT ( 'NONE',  ( 124.5550856135277087, 36.73359375108393010, 13.14518615778179722 ) ) ;
#27134 = CARTESIAN_POINT ( 'NONE',  ( -9.295050272127046043, 38.27148437608393294, -9.295050272127046043 ) ) ;
#27135 = CARTESIAN_POINT ( 'NONE',  ( 2.414731522848535132E-15, 33.60820312608392868, 13.14518615778179544 ) ) ;
#27136 = EDGE_CURVE ( 'NONE', #18595, #16904, #28040, .T. ) ;
#27137 = CARTESIAN_POINT ( 'NONE',  ( 95.54126587500000767, 94.06249999863440792, -7.484931351350258973E-15 ) ) ;
#27138 = LINE ( 'NONE', #1199, #22831 ) ;
#27139 = CARTESIAN_POINT ( 'NONE',  ( 108.0825317500000011, 112.6261737610028320, -50.27500000273119696 ) ) ;
#27140 = EDGE_CURVE ( 'NONE', #949, #5414, #26977, .T. ) ;
#27141 = ORIENTED_EDGE ( 'NONE', *, *, #2547, .T. ) ;
#27142 = CARTESIAN_POINT ( 'NONE',  ( 5.622872871577928144, 38.46992187716787726, -13.57481594606299247 ) ) ;
#27143 = CARTESIAN_POINT ( 'NONE',  ( -13.14518615778179544, 36.78320312608393294, 0.000000000000000000 ) ) ;
#27144 = CARTESIAN_POINT ( 'NONE',  ( 104.4587341249999639, 1.442382525525748735E-14, 5.187500001365592972 ) ) ;
#27145 =( BOUNDED_CURVE ( )  B_SPLINE_CURVE ( 2, ( #12700, #26656, #4992, #23558, #25828, #4035, #21425, #10570, #21563 ),
 .UNSPECIFIED., .F., .F. ) 
 B_SPLINE_CURVE_WITH_KNOTS ( ( 3, 2, 2, 2, 3 ),
 ( 0.6428571428571427937, 0.6517857142857141906, 0.6607142857142855874, 0.6696428571428569843, 0.6785714285714284921 ),
 .UNSPECIFIED. ) 
 CURVE ( )  GEOMETRIC_REPRESENTATION_ITEM ( )  RATIONAL_B_SPLINE_CURVE ( ( 1.000000000000000888, 0.9238795325112857393, 1.000000000000000000, 0.9238795325112867385, 1.000000000000000000, 0.9238795325112867385, 1.000000000000000000, 0.9238795325112877377, 0.9999999999999990008 ) ) 
 REPRESENTATION_ITEM ( '' )  );
#27146 = CARTESIAN_POINT ( 'NONE',  ( 55.70494972787295751, 38.07304687608393579, -9.295050272127046043 ) ) ;
#27147 = CARTESIAN_POINT ( 'NONE',  ( -13.57481594606304753, 38.66835937716787441, -5.622872871577872189 ) ) ;
#27148 = CARTESIAN_POINT ( 'NONE',  ( 4.157286354961724939, 36.00000000000000000, -12.92256159328856135 ) ) ;
#27149 = CARTESIAN_POINT ( 'NONE',  ( 189.5550856135277229, 36.43593750108394147, -13.14518615778179722 ) ) ;
#27150 = ORIENTED_EDGE ( 'NONE', *, *, #17356, .F. ) ;
#27151 = CARTESIAN_POINT ( 'NONE',  ( 9.295050272127047819, 33.90585937608393863, 9.295050272127046043 ) ) ;
#27152 = CARTESIAN_POINT ( 'NONE',  ( 101.4615807364564546, 123.4500000010924765, -1.461580736456474794 ) ) ;
#27153 = CARTESIAN_POINT ( 'NONE',  ( 101.8468681455907330, 93.74999999863439371, -4.458734124999994997 ) ) ;
#27154 = DIRECTION ( 'NONE',  ( 5.782411586589358625E-17, -0.000000000000000000, 1.000000000000000000 ) ) ;
#27155 = CARTESIAN_POINT ( 'NONE',  ( 99.99999999999997158, 101.5015231886685854, -47.37499999726882294 ) ) ;
#27156 = CARTESIAN_POINT ( 'NONE',  ( -5.622872871577873077, 34.00507812499999716, 13.57481594606304753 ) ) ;
#27157 = CARTESIAN_POINT ( 'NONE',  ( -9.295050272127046043, 34.10429687608393579, -9.295050272127046043 ) ) ;
#27158 = VECTOR ( 'NONE', #926, 1000.000000000000000 ) ;
#27159 = VERTEX_POINT ( 'NONE', #19081 ) ;
#27160 = DIRECTION ( 'NONE',  ( 0.000000000000000000, 0.000000000000000000, 1.000000000000000000 ) ) ;
#27161 = CARTESIAN_POINT ( 'NONE',  ( 65.00000000000000000, 40.15664062608393436, 13.14518615778179544 ) ) ;
#27162 = CYLINDRICAL_SURFACE ( 'NONE', #510, 4.999999999999989342 ) ;
#27163 = CARTESIAN_POINT ( 'NONE',  ( 185.7049497278729575, 34.50117187608393721, 9.295050272127047819 ) ) ;
#27164 = ORIENTED_EDGE ( 'NONE', *, *, #1041, .T. ) ;
#27165 = DIRECTION ( 'NONE',  ( 0.000000000000000000, 1.000000000000000000, 0.000000000000000000 ) ) ;
#27166 = CARTESIAN_POINT ( 'NONE',  ( 6.902378573780021398, 51.13402819307184188, -15.00000000000129141 ) ) ;
#27167 = CARTESIAN_POINT ( 'NONE',  ( -13.57481594606304398, 33.90585937499999858, 5.622872871577880183 ) ) ;
#27168 = EDGE_CURVE ( 'NONE', #12136, #13023, #27729, .T. ) ;
#27169 = CARTESIAN_POINT ( 'NONE',  ( 116.4251840539369596, 37.92421875216787441, 0.000000000000000000 ) ) ;
#27170 = VECTOR ( 'NONE', #18291, 1000.000000000000000 ) ;
#27171 = CARTESIAN_POINT ( 'NONE',  ( 98.89130886013153088, 116.9999999812857112, -44.94874572125286250 ) ) ;
#27172 = PLANE ( 'NONE',  #3698 ) ;
#27173 = CARTESIAN_POINT ( 'NONE',  ( 181.8548138422182205, 39.16445312608393436, 0.000000000000000000 ) ) ;
#27174 = ORIENTED_EDGE ( 'NONE', *, *, #18883, .T. ) ;
#27175 = PRESENTATION_STYLE_ASSIGNMENT (( #11742 ) ) ;
#27176 = CARTESIAN_POINT ( 'NONE',  ( 99.99999999999995737, 4.458734125000016313, 13.43750000136559386 ) ) ;
#27177 = AXIS2_PLACEMENT_3D ( 'NONE', #27500, #21213, #25905 ) ;
#27178 = CARTESIAN_POINT ( 'NONE',  ( 104.9999999999999716, 1.449011120738813565E-14, 12.62500000273118594 ) ) ;
#27179 = CARTESIAN_POINT ( 'NONE',  ( 208.5748159460630688, 38.17226562499999432, 5.622872871577868636 ) ) ;
#27180 = CARTESIAN_POINT ( 'NONE',  ( 181.4251840539369596, 40.30546875216787583, 0.000000000000000000 ) ) ;
#27181 = CARTESIAN_POINT ( 'NONE',  ( 65.00000000000000000, 32.21914062608393436, 13.14518615778179544 ) ) ;
#27182 = CARTESIAN_POINT ( 'NONE',  ( 103.5355339059327235, 91.99999999726880162, -3.535533905932738197 ) ) ;
#27183 = CARTESIAN_POINT ( 'NONE',  ( 97.50236033167492167, 117.6869444889999841, -45.52500000273119696 ) ) ;
#27184 = CARTESIAN_POINT ( 'NONE',  ( 13.57481594606304753, 40.65273437499999432, -5.622872871577873966 ) ) ;
#27185 = CARTESIAN_POINT ( 'NONE',  ( 107.0000000000000000, 110.0000000000000000, -50.00000000000000711 ) ) ;
#27186 = CARTESIAN_POINT ( 'NONE',  ( 7.171390501253594785, 31.30502191632583830, -11.52591802191987114 ) ) ;
#27187 = CARTESIAN_POINT ( 'NONE',  ( 95.00000000000000000, 91.31249999726878741, -2.071067811865479058 ) ) ;
#27188 = CARTESIAN_POINT ( 'NONE',  ( 143.5748159460630688, 34.25312499999999716, -1.662435489736055892E-15 ) ) ;
#27189 = ORIENTED_EDGE ( 'NONE', *, *, #19777, .F. ) ;
#27190 = DIRECTION ( 'NONE',  ( 0.000000000000000000, 1.000000000000000000, 0.000000000000000000 ) ) ;
#27191 =( BOUNDED_CURVE ( )  B_SPLINE_CURVE ( 2, ( #8500, #19472, #8776, #6360, #19610, #2659, #15034, #8640, #17758 ),
 .UNSPECIFIED., .F., .F. ) 
 B_SPLINE_CURVE_WITH_KNOTS ( ( 3, 2, 2, 2, 3 ),
 ( 0.2291666666666665741, 0.2395833333333332316, 0.2499999999999998335, 0.2604166666666665186, 0.2708333333333330928 ),
 .UNSPECIFIED. ) 
 CURVE ( )  GEOMETRIC_REPRESENTATION_ITEM ( )  RATIONAL_B_SPLINE_CURVE ( ( 1.000000000000000666, 0.9238795325112861834, 1.000000000000000000, 0.9238795325112867385, 1.000000000000000000, 0.9238795325112867385, 1.000000000000000000, 0.9238795325112884038, 0.9999999999999983347 ) ) 
 REPRESENTATION_ITEM ( '' )  );
#27192 = CARTESIAN_POINT ( 'NONE',  ( -5.444914386472297529, 34.25312500108393010, -13.14518615778179900 ) ) ;
#27193 = CARTESIAN_POINT ( 'NONE',  ( 9.598844408820456309, 34.45156250216787441, -9.598844408820458085 ) ) ;
#27194 = VECTOR ( 'NONE', #4444, 1000.000000000000000 ) ;
#27195 = CARTESIAN_POINT ( 'NONE',  ( 96.46446609406721961, 3.535533905932755072, 5.000000002731185944 ) ) ;
#27196 = CARTESIAN_POINT ( 'NONE',  ( 124.5550856135277087, 38.22187500108393010, -13.14518615778179900 ) ) ;
#27197 = CARTESIAN_POINT ( 'NONE',  ( 78.57481594606305464, 31.97109375216787441, -1.662435489736055892E-15 ) ) ;
#27198 = CARTESIAN_POINT ( 'NONE',  ( 5.622872871577780707, 37.67617187716787441, -13.57481594606313990 ) ) ;
#27199 = CARTESIAN_POINT ( 'NONE',  ( 5.444914386472302859, 39.21406250108392300, 13.14518615778179189 ) ) ;
#27200 = CARTESIAN_POINT ( 'NONE',  ( 106.9999999999999716, 1.473504056721760595E-14, 34.79898987322334136 ) ) ;
#27201 = CARTESIAN_POINT ( 'NONE',  ( 59.37712712842213136, 37.67617187499999432, -13.57481594606304753 ) ) ;
#27202 = CARTESIAN_POINT ( 'NONE',  ( 108.0825317500000011, 110.0000000000000000, -54.87499999726882294 ) ) ;
#27203 = CARTESIAN_POINT ( 'NONE',  ( 200.6228728715779823, 40.75195312499999289, -13.57481594606294095 ) ) ;
#27204 = FACE_OUTER_BOUND ( 'NONE', #9030, .T. ) ;
#27205 = CARTESIAN_POINT ( 'NONE',  ( 137.0656349887609053, 35.99999999999999289, 11.21307450592200539 ) ) ;
#27206 = DIRECTION ( 'NONE',  ( 0.000000000000000000, -1.000000000000000000, 0.000000000000000000 ) ) ;
#27207 = CARTESIAN_POINT ( 'NONE',  ( 0.000000000000000000, 36.00000000000000000, 0.000000000000000000 ) ) ;
#27208 = CARTESIAN_POINT ( 'NONE',  ( 181.4251840539369596, 39.36289062499999858, -5.622872871577872189 ) ) ;
#27209 = DIRECTION ( 'NONE',  ( -0.000000000000000000, 1.000000000000000000, -0.000000000000000000 ) ) ;
#27210 = CARTESIAN_POINT ( 'NONE',  ( 5.622872871577878406, 34.89804687499999147, 13.57481594606304576 ) ) ;
#27211 = CARTESIAN_POINT ( 'NONE',  ( 5.622872871577871301, 39.95820312499999716, -13.57481594606304753 ) ) ;
#27212 = CARTESIAN_POINT ( 'NONE',  ( 9.295050272127047819, 32.11992187608393579, 9.295050272127046043 ) ) ;
#27213 = CARTESIAN_POINT ( 'NONE',  ( 189.3771271284221314, 32.91367187499999858, -13.57481594606304753 ) ) ;
#27214 = CARTESIAN_POINT ( 'NONE',  ( 13.57481594606304931, 35.09648437716787583, 5.622872871577869525 ) ) ;
#27215 = DIRECTION ( 'NONE',  ( -1.000000000000000000, 0.000000000000000000, 0.000000000000000000 ) ) ;
#27216 = CARTESIAN_POINT ( 'NONE',  ( 96.84719886470459471, 84.31250000136560629, -3.152801135295383084 ) ) ;
#27217 = CARTESIAN_POINT ( 'NONE',  ( 65.00000000000000000, 31.62382812608393579, -13.14518615778179544 ) ) ;
#27218 = CARTESIAN_POINT ( 'NONE',  ( 96.46446609406726225, 90.37500000000000000, -3.535533905932738197 ) ) ;
#27219 = CARTESIAN_POINT ( 'NONE',  ( 92.99999999999998579, 107.7255621263696952, -46.90000000000002700 ) ) ;
#27220 = VERTEX_POINT ( 'NONE', #25090 ) ;
#27221 = CARTESIAN_POINT ( 'NONE',  ( 9.598844408820459861, 33.36015624999999574, 9.598844408820456309 ) ) ;
#27222 = CARTESIAN_POINT ( 'NONE',  ( 97.50236033167490746, 102.3130555110000159, -55.47499999726881725 ) ) ;
#27223 = CARTESIAN_POINT ( 'NONE',  ( 135.4449143864723055, 33.85625000108393579, 13.14518615778179189 ) ) ;
#27224 = EDGE_LOOP ( 'NONE', ( #22901, #2974, #1289, #3026 ) ) ;
#27225 = CARTESIAN_POINT ( 'NONE',  ( 92.99999999999998579, 110.0000000000000000, -52.49999999453763877 ) ) ;
#27226 = EDGE_CURVE ( 'NONE', #18595, #11873, #18678, .T. ) ;
#27227 = CARTESIAN_POINT ( 'NONE',  ( 130.0000000000000000, -7.395377635281828788, -1.503427012513233026E-14 ) ) ;
#27228 = CARTESIAN_POINT ( 'NONE',  ( 99.99999999999995737, 81.68750000136559208, 4.458734124999988779 ) ) ;
#27229 = CARTESIAN_POINT ( 'NONE',  ( 95.00000000000000000, 92.43750000000001421, -2.071067811865479058 ) ) ;
#27230 = CARTESIAN_POINT ( 'NONE',  ( 195.0000000000000000, 37.62656249999999858, -13.57481594606304576 ) ) ;
#27231 = CARTESIAN_POINT ( 'NONE',  ( 91.91746824999997045, 112.6261737610028320, -47.72499999726881725 ) ) ;
#27232 = CARTESIAN_POINT ( 'NONE',  ( 195.0000000000000000, 39.75976562608394005, -13.14518615778179544 ) ) ;
#27233 = CARTESIAN_POINT ( 'NONE',  ( -5.622872871577873077, 38.86679687716788578, 13.57481594606304753 ) ) ;
#27234 = ORIENTED_EDGE ( 'NONE', *, *, #8452, .T. ) ;
#27235 = CARTESIAN_POINT ( 'NONE',  ( 97.92893218813451028, 5.000000000000018652, 10.81250000000000000 ) ) ;
#27236 = VERTEX_POINT ( 'NONE', #25368 ) ;
#27237 = CARTESIAN_POINT ( 'NONE',  ( 13.14518615778179544, 32.41757812608393863, -1.609821015232357215E-15 ) ) ;
#27238 = CARTESIAN_POINT ( 'NONE',  ( 181.8548138422182205, 40.55351562608393579, 0.000000000000000000 ) ) ;
#27239 = CARTESIAN_POINT ( 'NONE',  ( 5.622872871577832221, 35.79101562716787299, 13.57481594606309194 ) ) ;
#27240 = CARTESIAN_POINT ( 'NONE',  ( 94.99999999999995737, 2.071067811865491048, 12.06250000273118772 ) ) ;
#27241 = CARTESIAN_POINT ( 'NONE',  ( 94.99999999999995737, 1.387778780781445676E-14, 2.999999999999999112 ) ) ;
#27242 = CARTESIAN_POINT ( 'NONE',  ( -5.444914386472299306, 32.16953125108393152, 13.14518615778179722 ) ) ;
#27243 = CARTESIAN_POINT ( 'NONE',  ( 104.9999999999999858, 2.071067811865486608, 11.68750000273118417 ) ) ;
#27244 = CARTESIAN_POINT ( 'NONE',  ( 59.37712712842213136, 32.41757812499999858, 13.57481594606304753 ) ) ;
#27245 = CARTESIAN_POINT ( 'NONE',  ( 101.4615807364564546, 122.8500000010924680, -1.461580736456474794 ) ) ;
#27246 = CARTESIAN_POINT ( 'NONE',  ( 0.000000000000000000, 80.00000000000000000, 0.000000000000000000 ) ) ;
#27247 = LINE ( 'NONE', #26824, #23666 ) ;
#27248 = CARTESIAN_POINT ( 'NONE',  ( 98.15313185440925281, -4.458734124999987891, 5.875000001365591196 ) ) ;
#27249 = CARTESIAN_POINT ( 'NONE',  ( 2.493653234604083739E-15, 38.12265625216787157, 13.57481594606304576 ) ) ;
#27250 = CARTESIAN_POINT ( 'NONE',  ( 99.99999999999995737, -4.458734124999988779, 10.68750000136559208 ) ) ;
#27251 = CARTESIAN_POINT ( 'NONE',  ( 94.33688103937537051, 114.1144967660473242, -46.70000000546237828 ) ) ;
#27252 = CARTESIAN_POINT ( 'NONE',  ( 103.1528011352953484, 94.43749999863440792, 3.152801135295352886 ) ) ;
#27253 = CARTESIAN_POINT ( 'NONE',  ( 104.9999999999999716, 1.449011120738813565E-14, 9.500000000000000000 ) ) ;
#27254 = CARTESIAN_POINT ( 'NONE',  ( 108.0825317499999869, 107.3738262389971680, -54.72499999726881015 ) ) ;
#27255 = CARTESIAN_POINT ( 'NONE',  ( -9.295050272127044266, 33.70742187608393436, 9.295050272127047819 ) ) ;
#27256 = AXIS2_PLACEMENT_3D ( 'NONE', #9065, #9204, #14279 ) ;
#27257 = ORIENTED_EDGE ( 'NONE', *, *, #7391, .T. ) ;
#27258 = DIRECTION ( 'NONE',  ( 0.000000000000000000, 0.000000000000000000, 1.000000000000000000 ) ) ;
#27259 = PRODUCT_DEFINITION_FORMATION_WITH_SPECIFIED_SOURCE ( 'ANY', '', #16047, .NOT_KNOWN. ) ;
#27260 = CARTESIAN_POINT ( 'NONE',  ( 2.493653234604083739E-15, 37.22968749999999716, 13.57481594606304576 ) ) ;
#27261 = ADVANCED_FACE ( 'NONE', ( #1439 ), #10097, .T. ) ;
#27262 = CARTESIAN_POINT ( 'NONE',  ( 189.5550856135277229, 34.05468750108393294, -13.14518615778179900 ) ) ;
#27263 = VERTEX_POINT ( 'NONE', #16671 ) ;
#27264 = CARTESIAN_POINT ( 'NONE',  ( 202.1154903918443608, 49.99999999945652718, -11.58166858714790592 ) ) ;
#27265 = CARTESIAN_POINT ( 'NONE',  ( 104.4587341249999639, 1.442382525525748735E-14, 6.187500001365592084 ) ) ;
#27266 = EDGE_LOOP ( 'NONE', ( #11139, #8268, #16984, #22322 ) ) ;
#27267 = CARTESIAN_POINT ( 'NONE',  ( 102.4976396683250925, 117.6869444889999841, -45.97500000273119269 ) ) ;
#27268 = CARTESIAN_POINT ( 'NONE',  ( 5.444914386472297529, 34.74921875108394431, -13.14518615778179900 ) ) ;
#27269 = CARTESIAN_POINT ( 'NONE',  ( 189.3771271284221314, 39.36289062716787157, -13.57481594606304753 ) ) ;
#27270 = CARTESIAN_POINT ( 'NONE',  ( 2.414731522848535132E-15, 39.16445312608392726, 13.14518615778179544 ) ) ;
#27271 = AXIS2_PLACEMENT_3D ( 'NONE', #14904, #23625, #16648 ) ;
#27272 = VECTOR ( 'NONE', #22490, 999.9999999999998863 ) ;
#27273 = CARTESIAN_POINT ( 'NONE',  ( 13.14518615778179544, 36.38632812608393863, -1.609821015232357215E-15 ) ) ;
#27274 = CARTESIAN_POINT ( 'NONE',  ( -8.049105076161786076E-16, 31.62382812608393579, -13.14518615778179544 ) ) ;
#27275 = CARTESIAN_POINT ( 'NONE',  ( 104.4587341249999923, 90.62499999863439371, -1.846868145590737198 ) ) ;
#27276 = CARTESIAN_POINT ( 'NONE',  ( 104.9999999999999858, 90.00000000000000000, -6.938893903907228378E-15 ) ) ;
#27277 = ORIENTED_EDGE ( 'NONE', *, *, #1683, .T. ) ;
#27278 = CARTESIAN_POINT ( 'NONE',  ( -9.598844408820458085, 37.03125000216787299, -9.598844408820458085 ) ) ;
#27279 = CARTESIAN_POINT ( 'NONE',  ( -13.14518615778179544, 33.60820312608393579, 0.000000000000000000 ) ) ;
#27280 = CARTESIAN_POINT ( 'NONE',  ( 95.54126587499996504, -1.846868145590724986, 5.750000001365591196 ) ) ;
#27281 = CARTESIAN_POINT ( 'NONE',  ( 95.54126587499996504, 82.62500000136560629, -1.846868145590750077 ) ) ;
#27282 = CARTESIAN_POINT ( 'NONE',  ( 94.99999999999995737, 1.387778780781445676E-14, 8.125000002731185944 ) ) ;
#27283 = CARTESIAN_POINT ( 'NONE',  ( 181.4251840539369596, 38.66835937499999432, 5.622872871577880183 ) ) ;
#27284 = ORIENTED_EDGE ( 'NONE', *, *, #14023, .F. ) ;
#27285 = CARTESIAN_POINT ( 'NONE',  ( -13.14518615778179189, 34.45156250108394147, 5.444914386472304635 ) ) ;
#27287 = EDGE_CURVE ( 'NONE', #22301, #20134, #14783, .T. ) ;
#27286 = CARTESIAN_POINT ( 'NONE',  ( 98.23223304703363112, 122.6000000021849559, -1.767766952966370209 ) ) ;
#27288 = CARTESIAN_POINT ( 'NONE',  ( 95.54126587499999346, 94.99999999863439371, -1.846868145590737864 ) ) ;
#27289 = EDGE_CURVE ( 'NONE', #16160, #18726, #25874, .T. ) ;
#27290 = CARTESIAN_POINT ( 'NONE',  ( 200.4449143864723055, 36.23750000108393721, 13.14518615778179189 ) ) ;
#27291 = CARTESIAN_POINT ( 'NONE',  ( 102.4976396683250783, 102.3130555110000159, -49.27499999726882152 ) ) ;
#27292 = CARTESIAN_POINT ( 'NONE',  ( 97.92893218813455292, 93.68749999999998579, 5.000000000000023981 ) ) ;
#27293 = CARTESIAN_POINT ( 'NONE',  ( 5.444914386472302859, 32.07031250108393294, 13.14518615778179189 ) ) ;
#27294 = VERTEX_POINT ( 'NONE', #16533 ) ;
#27295 = CARTESIAN_POINT ( 'NONE',  ( 92.99999999999998579, 110.0000000000000000, -45.00000000000001421 ) ) ;
#27296 = CARTESIAN_POINT ( 'NONE',  ( 78.14518615778180788, 37.92421875108393436, 5.444914386472293977 ) ) ;
#27297 = ADVANCED_FACE ( 'NONE', ( #7699 ), #16392, .T. ) ;
#27298 = CARTESIAN_POINT ( 'NONE',  ( 99.99999999999995737, 1.387778780781445676E-14, 34.79898987322334136 ) ) ;
#27299 = CARTESIAN_POINT ( 'NONE',  ( 201.9444263933115167, 31.75150625057403175, -11.16113171639042356 ) ) ;
#27300 = ORIENTED_EDGE ( 'NONE', *, *, #4279, .F. ) ;
#27301 = CARTESIAN_POINT ( 'NONE',  ( 78.57481594606305464, 37.42812499999999432, -1.662435489736055892E-15 ) ) ;
#27302 = CARTESIAN_POINT ( 'NONE',  ( 1.138768117104975941, 50.00000000043849013, -13.56816686242529357 ) ) ;
#27303 = CARTESIAN_POINT ( 'NONE',  ( 114.9999999999999858, 0.000000000000000000, -8.673617379884035472E-16 ) ) ;
#27304 = EDGE_CURVE ( 'NONE', #15088, #11263, #15493, .T. ) ;
#27305 = CARTESIAN_POINT ( 'NONE',  ( 130.0000000000000000, 38.91640625216786731, 13.57481594606304576 ) ) ;
#27306 =( BOUNDED_CURVE ( )  B_SPLINE_CURVE ( 2, ( #27253, #7983, #21102, #12104, #14111, #20694, #27527, #14392, #3301 ),
 .UNSPECIFIED., .F., .F. ) 
 B_SPLINE_CURVE_WITH_KNOTS ( ( 3, 2, 2, 2, 3 ),
 ( 0.3928571428571428492, 0.4017857142857143016, 0.4107142857142856984, 0.4196428571428571508, 0.4285714285714285476 ),
 .UNSPECIFIED. ) 
 CURVE ( )  GEOMETRIC_REPRESENTATION_ITEM ( )  RATIONAL_B_SPLINE_CURVE ( ( 1.000000000000000000, 0.9238795325112867385, 1.000000000000000000, 0.9238795325112867385, 1.000000000000000000, 0.9238795325112867385, 1.000000000000000000, 0.9238795325112867385, 1.000000000000000000 ) ) 
 REPRESENTATION_ITEM ( '' )  );
#27307 = CARTESIAN_POINT ( 'NONE',  ( 99.99999999999998579, 90.00000000000000000, -6.938893903907228378E-15 ) ) ;
#27308 = DIRECTION ( 'NONE',  ( 0.000000000000000000, 0.000000000000000000, 1.000000000000000000 ) ) ;
#27309 = CARTESIAN_POINT ( 'NONE',  ( 200.4449143864723055, 37.82500000108392868, 13.14518615778179189 ) ) ;
#27310 = VERTEX_POINT ( 'NONE', #14518 ) ;
#27311 = FILL_AREA_STYLE ('',( #18323 ) ) ;
#27312 = CARTESIAN_POINT ( 'NONE',  ( 95.54126587499995082, 1.846868145590750077, 1.375000001365592972 ) ) ;
#27313 = CARTESIAN_POINT ( 'NONE',  ( 4.157286354961724939, 36.00000000000000000, -12.92256159328856135 ) ) ;
#27314 = CARTESIAN_POINT ( 'NONE',  ( 9.598844408820459861, 39.71015624999999716, 9.598844408820456309 ) ) ;
#27315 = AXIS2_PLACEMENT_3D ( 'NONE', #11834, #11407, #5305 ) ;
#27316 = CARTESIAN_POINT ( 'NONE',  ( 99.99999999999995737, 84.18750000136560629, -4.458734125000016313 ) ) ;
#27317 = CARTESIAN_POINT ( 'NONE',  ( 78.14518615778179367, 32.36796875108393579, 5.444914386472293977 ) ) ;
#27318 = LINE ( 'NONE', #5647, #2714 ) ;
#27319 = CARTESIAN_POINT ( 'NONE',  ( 5.444914386472302859, 40.20625000108394431, 13.14518615778179189 ) ) ;
#27320 = CARTESIAN_POINT ( 'NONE',  ( -8.312177448680279460E-16, 38.42031249999999432, -13.57481594606304576 ) ) ;
#27321 = CARTESIAN_POINT ( 'NONE',  ( 93.00000000000000000, 110.0000000000000000, -48.50000000546238255 ) ) ;
#27322 = CYLINDRICAL_SURFACE ( 'NONE', #15911, 13.57481594606304398 ) ;
#27323 = CARTESIAN_POINT ( 'NONE',  ( 143.5748159460630404, 34.20351562499999432, 5.622872871577869525 ) ) ;
#27324 = EDGE_LOOP ( 'NONE', ( #11272, #19433, #15979, #27123 ) ) ;
#27325 = CARTESIAN_POINT ( 'NONE',  ( 99.99999999999995737, 78.00000000000000000, 2.999999999999990674 ) ) ;
#27326 = CARTESIAN_POINT ( 'NONE',  ( -9.598844408820454532, 38.71796874999999716, 9.598844408820459861 ) ) ;
#27327 = CARTESIAN_POINT ( 'NONE',  ( -13.57481594606304576, 32.36796875216787583, 0.000000000000000000 ) ) ;
#27328 = CARTESIAN_POINT ( 'NONE',  ( 94.99999999999995737, -2.071067811865466624, 7.187500002731185944 ) ) ;
#27329 = CARTESIAN_POINT ( 'NONE',  ( 135.4449143864723055, 39.71015625108393010, -13.14518615778179900 ) ) ;
#27330 = CARTESIAN_POINT ( 'NONE',  ( 65.00000000000000000, 39.56132812608393579, -13.14518615778179544 ) ) ;
#27331 = ADVANCED_FACE ( 'NONE', ( #14242 ), #5714, .F. ) ;
#27332 = CARTESIAN_POINT ( 'NONE',  ( 99.99999999999998579, 91.25000000000000000, -4.999999999999997335 ) ) ;
#27333 = CARTESIAN_POINT ( 'NONE',  ( -13.14518615778179544, 39.75976562608393294, 0.000000000000000000 ) ) ;
#27334 = DIRECTION ( 'NONE',  ( 0.000000000000000000, 0.000000000000000000, -1.000000000000000000 ) ) ;
#27335 = DIRECTION ( 'NONE',  ( -0.000000000000000000, 1.000000000000000000, -0.000000000000000000 ) ) ;
#27336 = CARTESIAN_POINT ( 'NONE',  ( 104.9952793366501567, 103.1245878333314465, -51.17499999726881299 ) ) ;
#27337 = CIRCLE ( 'NONE', #7289, 13.57481594606304398 ) ;
#27338 = FACE_OUTER_BOUND ( 'NONE', #15934, .T. ) ;
#27339 = CARTESIAN_POINT ( 'NONE',  ( 102.0710678118654329, 82.81250000273118417, -5.000000000000004441 ) ) ;
#27340 = DIRECTION ( 'NONE',  ( -0.000000000000000000, 1.000000000000000000, -0.000000000000000000 ) ) ;
#27341 = CARTESIAN_POINT ( 'NONE',  ( 101.0355339059327378, 123.1499999999999915, -2.499999999999997780 ) ) ;
#27342 = CARTESIAN_POINT ( 'NONE',  ( 98.53841926354351699, 124.0500000010924708, 1.461580736456455920 ) ) ;
#27343 = CARTESIAN_POINT ( 'NONE',  ( 129.0044387749465216, 36.00000000000000000, -13.45766439703019302 ) ) ;
#27344 = VECTOR ( 'NONE', #18501, 1000.000000000000000 ) ;
#27345 = CARTESIAN_POINT ( 'NONE',  ( 99.99999999999995737, 85.00000000000000000, 4.999999999999990230 ) ) ;
#27346 = CARTESIAN_POINT ( 'NONE',  ( 95.54126587499996504, 1.387778780781445676E-14, 13.43750000136559386 ) ) ;
#27347 = CARTESIAN_POINT ( 'NONE',  ( 5.622872871577878406, 32.51679687499999716, 13.57481594606304576 ) ) ;
#27348 = ORIENTED_EDGE ( 'NONE', *, *, #4251, .F. ) ;
#27349 = DIRECTION ( 'NONE',  ( -0.000000000000000000, 1.000000000000000000, -0.000000000000000000 ) ) ;
#27350 = CARTESIAN_POINT ( 'NONE',  ( 9.598844408820456309, 39.90859374999999432, -9.598844408820458085 ) ) ;
#27351 = CARTESIAN_POINT ( 'NONE',  ( -8.049105076161786076E-16, 31.62382812608393579, -13.14518615778179544 ) ) ;
#27352 = CARTESIAN_POINT ( 'NONE',  ( 5.444914386472297529, 35.54296875108393294, -13.14518615778179722 ) ) ;
#27353 = CARTESIAN_POINT ( 'NONE',  ( -5.622872871577873077, 33.31054687716787299, 13.57481594606304753 ) ) ;
#27354 = CARTESIAN_POINT ( 'NONE',  ( 96.46446609406721961, 3.535533905932755072, 3.000000002731185944 ) ) ;
#27355 = CARTESIAN_POINT ( 'NONE',  ( 96.84719886470459471, 79.56250000136559208, 3.152801135295355994 ) ) ;
#27356 = CARTESIAN_POINT ( 'NONE',  ( 59.55508561352770158, 31.97109375108393436, 13.14518615778179722 ) ) ;
#27357 =( BOUNDED_CURVE ( )  B_SPLINE_CURVE ( 2, ( #12007, #1215, #9880, #18588, #9411, #16397, #24675, #1029, #9700 ),
 .UNSPECIFIED., .F., .F. ) 
 B_SPLINE_CURVE_WITH_KNOTS ( ( 3, 2, 2, 2, 3 ),
 ( 0.8124999999999998890, 0.8229166666666665186, 0.8333333333333331483, 0.8437499999999997780, 0.8541666666666662966 ),
 .UNSPECIFIED. ) 
 CURVE ( )  GEOMETRIC_REPRESENTATION_ITEM ( )  RATIONAL_B_SPLINE_CURVE ( ( 1.000000000000000888, 0.9238795325112859613, 1.000000000000000000, 0.9238795325112867385, 1.000000000000000000, 0.9238795325112867385, 1.000000000000000000, 0.9238795325112891810, 0.9999999999999975575 ) ) 
 REPRESENTATION_ITEM ( '' )  );
#27358 = CARTESIAN_POINT ( 'NONE',  ( 106.5389055433251002, 105.2492070361643215, -46.57500000273119412 ) ) ;
#27359 = CARTESIAN_POINT ( 'NONE',  ( 97.93301270000000613, 123.1500000010924651, -9.540979117872439019E-15 ) ) ;
#27360 = CARTESIAN_POINT ( 'NONE',  ( 143.5748159460630688, 38.96601562499999005, 5.622872871577868636 ) ) ;
#27361 = CARTESIAN_POINT ( 'NONE',  ( 104.9952793366501709, 103.1245878333314323, -55.17499999726882720 ) ) ;
#27362 = CARTESIAN_POINT ( 'NONE',  ( 120.7049497278729575, 35.89023437608393152, -9.295050272127046043 ) ) ;
#27363 = ORIENTED_EDGE ( 'NONE', *, *, #8596, .T. ) ;
#27364 = CARTESIAN_POINT ( 'NONE',  ( 3.865414375413191106, 54.10683252460150783, -15.00000000000000533 ) ) ;
#27365 = CYLINDRICAL_SURFACE ( 'NONE', #7123, 13.57481594606304398 ) ;
#27366 = CARTESIAN_POINT ( 'NONE',  ( 98.15313185440925281, 82.62500000136560629, 4.458734124999987891 ) ) ;
#27367 = CARTESIAN_POINT ( 'NONE',  ( 124.3771271284221598, 38.76757812499998579, 13.57481594606308128 ) ) ;
#27368 = CARTESIAN_POINT ( 'NONE',  ( 108.0825317500000011, 110.0000000000000000, -50.62499999726882294 ) ) ;
#27369 = CARTESIAN_POINT ( 'NONE',  ( 2.493653234604083739E-15, 38.12265625216787157, 13.57481594606304576 ) ) ;
#27370 = ORIENTED_EDGE ( 'NONE', *, *, #24954, .T. ) ;
#27371 = CARTESIAN_POINT ( 'NONE',  ( 102.0710678118654329, 5.000000000000018652, 8.687499999999998224 ) ) ;
#27372 = ORIENTED_EDGE ( 'NONE', *, *, #4038, .F. ) ;
#27373 = CARTESIAN_POINT ( 'NONE',  ( 5.444914386472297529, 33.36015625108393579, -13.14518615778179900 ) ) ;
#27374 = CARTESIAN_POINT ( 'NONE',  ( 204.2950502721270425, 40.05742187608392868, 9.295050272127046043 ) ) ;
#27375 = DIRECTION ( 'NONE',  ( -0.8660254037844392627, 0.000000000000000000, 0.4999999999999987788 ) ) ;
#27376 = CARTESIAN_POINT ( 'NONE',  ( 102.0710678118654329, 5.000000000000018652, 0.8125000027311859441 ) ) ;
#27377 = CARTESIAN_POINT ( 'NONE',  ( 139.2950502721270425, 37.67617187608393436, 9.295050272127046043 ) ) ;
#27378 = LINE ( 'NONE', #5713, #3602 ) ;
#27379 = EDGE_CURVE ( 'NONE', #20261, #15363, #122, .T. ) ;
#27380 = CARTESIAN_POINT ( 'NONE',  ( 104.9999999999999716, -2.071067811865452857, 11.43749999999999822 ) ) ;
#27381 = CARTESIAN_POINT ( 'NONE',  ( 104.4587341249999781, 95.31249999863440792, -6.938893903907228378E-15 ) ) ;
#27382 = CARTESIAN_POINT ( 'NONE',  ( 101.7677669529663547, 123.7000000000000028, 1.767766952966350891 ) ) ;
#27383 = CARTESIAN_POINT ( 'NONE',  ( 195.0000000000000000, 40.40468749999999432, 13.57481594606304576 ) ) ;
#27384 = APPLICATION_PROTOCOL_DEFINITION ( 'draft international standard', 'automotive_design', 1998, #3147 ) ;
#27385 = CARTESIAN_POINT ( 'NONE',  ( 131.1371678245417627, 36.00000000000000000, 13.09590655363595602 ) ) ;
#27386 = CARTESIAN_POINT ( 'NONE',  ( 101.8468681455906903, 4.458734125000016313, 7.375000001365592084 ) ) ;
#27387 = CARTESIAN_POINT ( 'NONE',  ( 97.83688103937538472, 116.6573956140660897, -52.90000000546237402 ) ) ;
#27388 = CARTESIAN_POINT ( 'NONE',  ( 104.4587341249999781, 1.846868145590750521, 9.000000001365592084 ) ) ;
#27389 = CARTESIAN_POINT ( 'NONE',  ( 107.0000000000000142, 112.2744378736303332, -47.40000000546237402 ) ) ;
#27390 = CARTESIAN_POINT ( 'NONE',  ( 99.99999999999998579, 93.31249999863440792, 4.458734124999981674 ) ) ;
#27391 = CARTESIAN_POINT ( 'NONE',  ( 104.9999999999999716, -2.071067811865462627, 4.437500000000000000 ) ) ;
#27392 = CARTESIAN_POINT ( 'NONE',  ( 102.0669872999999797, 122.5500000010924850, -9.794112055954760458E-15 ) ) ;
#27393 = CARTESIAN_POINT ( 'NONE',  ( -13.14518615778179189, 32.07031250108393294, 5.444914386472304635 ) ) ;
#27394 = EDGE_LOOP ( 'NONE', ( #6659, #11525, #19416, #20707, #6334, #19816 ) ) ;
#27395 = CARTESIAN_POINT ( 'NONE',  ( 104.4587341249999781, 83.25000000136560629, -1.846868145590750299 ) ) ;
#27396 = FACE_OUTER_BOUND ( 'NONE', #26952, .T. ) ;
#27397 = CARTESIAN_POINT ( 'NONE',  ( 189.5550856135277229, 33.55859375108393294, 13.14518615778179722 ) ) ;
#27398 = ORIENTED_EDGE ( 'NONE', *, *, #9167, .F. ) ;
#27399 = CARTESIAN_POINT ( 'NONE',  ( -13.57481594606304398, 37.08085937499999574, 5.622872871577880183 ) ) ;
#27400 = CARTESIAN_POINT ( 'NONE',  ( 98.15313185440925281, 4.458734125000016313, 5.500000001365592972 ) ) ;
#27401 = VERTEX_POINT ( 'NONE', #17497 ) ;
#27402 = CARTESIAN_POINT ( 'NONE',  ( 95.00472066334982912, 103.1245878333314323, -47.07500000273119412 ) ) ;
#27403 = CARTESIAN_POINT ( 'NONE',  ( -9.295050272127044266, 31.92148437608393508, 9.295050272127047819 ) ) ;
#27404 = CARTESIAN_POINT ( 'NONE',  ( 99.99999999999995737, 85.00000000000000000, -1.387778780781445676E-14 ) ) ;
#27405 = CARTESIAN_POINT ( 'NONE',  ( -9.295050272127044266, 39.06523437608392868, 9.295050272127047819 ) ) ;
#27406 = CARTESIAN_POINT ( 'NONE',  ( 13.14518615778179722, 37.13046875108393863, 5.444914386472293977 ) ) ;
#27407 = CARTESIAN_POINT ( 'NONE',  ( 13.14518615778179900, 33.75703125108393010, 5.444914386472293977 ) ) ;
#27408 = CARTESIAN_POINT ( 'NONE',  ( 103.1528011352953484, 92.43749999863440792, 3.152801135295352886 ) ) ;
#27409 = CARTESIAN_POINT ( 'NONE',  ( 107.0000000000000142, 107.7255621263696952, -50.10000000000000853 ) ) ;
#27410 = CARTESIAN_POINT ( 'NONE',  ( 13.14518615778179900, 32.36796875108393579, 5.444914386472293977 ) ) ;
#27411 = CARTESIAN_POINT ( 'NONE',  ( 95.54126587499996504, 1.387778780781445676E-14, 3.687500001365593416 ) ) ;
#27412 = CARTESIAN_POINT ( 'NONE',  ( 98.15313185440923860, 81.50000000136560629, -4.458734125000016313 ) ) ;
#27413 = CARTESIAN_POINT ( 'NONE',  ( -13.14518615778179544, 34.99726562608393721, 0.000000000000000000 ) ) ;
#27414 = CARTESIAN_POINT ( 'NONE',  ( 74.59884440882045453, 39.21406250216787015, -9.598844408820458085 ) ) ;
#27415 = CARTESIAN_POINT ( 'NONE',  ( -8.312177448680279460E-16, 39.31328125216787583, -13.57481594606304576 ) ) ;
#27416 = ORIENTED_EDGE ( 'NONE', *, *, #11740, .F. ) ;
#27417 = SURFACE_STYLE_USAGE ( .BOTH. , #5897 ) ;
#27418 = CARTESIAN_POINT ( 'NONE',  ( 97.93301269999999192, 123.8000000010924850, 0.8561741729129329626 ) ) ;
#27419 = CARTESIAN_POINT ( 'NONE',  ( 103.1528011352953484, 94.43749999863440792, 3.152801135295352886 ) ) ;
#27420 = CARTESIAN_POINT ( 'NONE',  ( 102.0710678118654329, -4.999999999999989342, 3.437500002731184612 ) ) ;
#27421 = CARTESIAN_POINT ( 'NONE',  ( 108.0825317499999869, 107.3738262389971538, -54.97499999726881015 ) ) ;
#27422 = CARTESIAN_POINT ( 'NONE',  ( 95.00000000000000000, 93.50000000000000000, -7.551217303480904118E-15 ) ) ;
#27423 = CARTESIAN_POINT ( 'NONE',  ( -13.14518615778179900, 31.77265625108393365, -5.444914386472297529 ) ) ;
#27424 = VERTEX_POINT ( 'NONE', #24061 ) ;
#27425 = CARTESIAN_POINT ( 'NONE',  ( 55.70494972787295751, 36.68398437608393436, -9.295050272127046043 ) ) ;
#27426 = CARTESIAN_POINT ( 'NONE',  ( 99.99999999999998579, 138.0000000000000000, -5.204170427930421283E-15 ) ) ;
#27427 = DIRECTION ( 'NONE',  ( -0.000000000000000000, -0.000000000000000000, -1.000000000000000000 ) ) ;
#27428 = EDGE_CURVE ( 'NONE', #138, #2116, #23921, .T. ) ;
#27429 = VERTEX_POINT ( 'NONE', #17070 ) ;
#27430 = CARTESIAN_POINT ( 'NONE',  ( 102.1631189606246295, 116.6573956140660897, -54.60000000000000853 ) ) ;
#27431 = CARTESIAN_POINT ( 'NONE',  ( -7.089417272331180797, 49.99999999943663909, -11.59823041029098256 ) ) ;
#27432 = CARTESIAN_POINT ( 'NONE',  ( 143.5748159460630688, 36.78320312716788010, -5.622872871577873966 ) ) ;
#27433 = CARTESIAN_POINT ( 'NONE',  ( 130.0000000000000000, 37.32890625216786873, 13.57481594606304576 ) ) ;
#27434 = CARTESIAN_POINT ( 'NONE',  ( 94.33688103937537051, 114.1144967660473242, -44.70000000546237828 ) ) ;
#27435 = EDGE_CURVE ( 'NONE', #1080, #20134, #27712, .T. ) ;
#27436 = LINE ( 'NONE', #23434, #12309 ) ;
#27437 = CARTESIAN_POINT ( 'NONE',  ( 195.0000000000000000, 37.37851562608393863, -13.14518615778179544 ) ) ;
#27438 = ORIENTED_EDGE ( 'NONE', *, *, #27513, .F. ) ;
#27439 = EDGE_CURVE ( 'NONE', #21288, #439, #4399, .T. ) ;
#27440 = ORIENTED_EDGE ( 'NONE', *, *, #20510, .F. ) ;
#27441 =( NAMED_UNIT ( * ) SI_UNIT ( $, .STERADIAN. ) SOLID_ANGLE_UNIT ( ) );
#27442 = CARTESIAN_POINT ( 'NONE',  ( 104.4587341249999781, 1.846868145590750299, 2.000000001365591640 ) ) ;
#27443 = CARTESIAN_POINT ( 'NONE',  ( 96.46446609406721961, 83.87500000000000000, -3.535533905932755072 ) ) ;
#27444 = CARTESIAN_POINT ( 'NONE',  ( -13.57481594606304753, 40.15664062499999432, -5.622872871577872189 ) ) ;
#27445 = EDGE_CURVE ( 'NONE', #5424, #5694, #25773, .T. ) ;
#27446 = CARTESIAN_POINT ( 'NONE',  ( 98.15313185440923860, 83.25000000136559208, -4.458734125000016313 ) ) ;
#27447 = DIRECTION ( 'NONE',  ( 0.000000000000000000, 0.000000000000000000, 1.000000000000000000 ) ) ;
#27448 = CARTESIAN_POINT ( 'NONE',  ( 94.99999999999995737, 79.12500000273118417, -1.387778780781445676E-14 ) ) ;
#27449 = CARTESIAN_POINT ( 'NONE',  ( -8.049105076161786076E-16, 40.55351562608393579, -13.14518615778179544 ) ) ;
#27450 = CARTESIAN_POINT ( 'NONE',  ( 94.99999999999995737, 81.00000000000000000, -1.387778780781445676E-14 ) ) ;
#27451 = CARTESIAN_POINT ( 'NONE',  ( 6.351932228771040023, 35.99999999999999289, 11.61660627739524543 ) ) ;
#27452 = CARTESIAN_POINT ( 'NONE',  ( 104.9999999999999716, 93.93749999726880162, -2.071067811865478170 ) ) ;
#27453 = CARTESIAN_POINT ( 'NONE',  ( 106.5389055433250860, 105.2492070361643215, -48.82499999726882578 ) ) ;
#27454 = ORIENTED_EDGE ( 'NONE', *, *, #18072, .T. ) ;
#27455 = AXIS2_PLACEMENT_3D ( 'NONE', #13366, #22374, #19950 ) ;
#27456 = EDGE_CURVE ( 'NONE', #24582, #7335, #12647, .T. ) ;
#27457 = EDGE_LOOP ( 'NONE', ( #15400, #2034, #15133, #9354 ) ) ;
#27458 = CARTESIAN_POINT ( 'NONE',  ( 74.59884440882045453, 36.53515624999999289, 9.598844408820456309 ) ) ;
#27459 = PRODUCT_DEFINITION_CONTEXT ( 'detailed design', #12763, 'design' ) ;
#27460 = CARTESIAN_POINT ( 'NONE',  ( 13.57481594606304931, 38.96601562499999005, 5.622872871577869525 ) ) ;
#27461 = CARTESIAN_POINT ( 'NONE',  ( 9.598844408820459861, 31.87187500216787228, 9.598844408820456309 ) ) ;
#27462 =( BOUNDED_CURVE ( )  B_SPLINE_CURVE ( 2, ( #25296, #1375, #11752, #27038, #22471, #16462, #27182, #16327, #3223 ),
 .UNSPECIFIED., .F., .T. ) 
 B_SPLINE_CURVE_WITH_KNOTS ( ( 3, 2, 2, 2, 3 ),
 ( 0.1500000000000001332, 0.1750000000000001554, 0.2000000000000001776, 0.2250000000000001998, 0.2500000000000002220 ),
 .UNSPECIFIED. ) 
 CURVE ( )  GEOMETRIC_REPRESENTATION_ITEM ( )  RATIONAL_B_SPLINE_CURVE ( ( 0.9999999999999995559, 0.9238795325112871826, 1.000000000000000000, 0.9238795325112867385, 1.000000000000000000, 0.9238795325112867385, 1.000000000000000000, 0.9238795325112860723, 1.000000000000000666 ) ) 
 REPRESENTATION_ITEM ( '' )  );
#27463 = CARTESIAN_POINT ( 'NONE',  ( 102.0710678118654329, -4.999999999999989342, 7.437500002731186832 ) ) ;
#27464 = CARTESIAN_POINT ( 'NONE',  ( 124.5550856135277087, 39.31328125108394289, 13.14518615778179722 ) ) ;
#27465 = CARTESIAN_POINT ( 'NONE',  ( 65.00000000000000000, 35.98945312608393010, 13.14518615778179544 ) ) ;
#27466 = CARTESIAN_POINT ( 'NONE',  ( 99.99999999999998579, 137.0000000000000000, 12.50000000000001066 ) ) ;
#27467 = CARTESIAN_POINT ( 'NONE',  ( 13.14518615778179544, 36.18789062608393436, -1.609821015232357215E-15 ) ) ;
#27468 =( BOUNDED_CURVE ( )  B_SPLINE_CURVE ( 2, ( #14252, #16545, #24958, #5443, #9706, #3722, #12384, #22973, #20830 ),
 .UNSPECIFIED., .F., .F. ) 
 B_SPLINE_CURVE_WITH_KNOTS ( ( 3, 2, 2, 2, 3 ),
 ( 0.1041666666666664909, 0.1145833333333332732, 0.1250000000000000833, 0.1354166666666668517, 0.1458333333333336757 ),
 .UNSPECIFIED. ) 
 CURVE ( )  GEOMETRIC_REPRESENTATION_ITEM ( )  RATIONAL_B_SPLINE_CURVE ( ( 1.000000000000001332, 0.9238795325112854062, 1.000000000000000000, 0.9238795325112867385, 1.000000000000000000, 0.9238795325112867385, 1.000000000000000000, 0.9238795325112842960, 1.000000000000002442 ) ) 
 REPRESENTATION_ITEM ( '' )  );
#27469 = CARTESIAN_POINT ( 'NONE',  ( 99.99999999999998579, 124.1000000021849416, -2.499999999999997780 ) ) ;
#27470 = DIRECTION ( 'NONE',  ( 0.000000000000000000, 0.000000000000000000, 1.000000000000000000 ) ) ;
#27471 = ADVANCED_FACE ( 'NONE', ( #21373 ), #12786, .T. ) ;
#27472 = DIRECTION ( 'NONE',  ( -0.000000000000000000, 1.000000000000000000, -0.000000000000000000 ) ) ;
#27473 = DIRECTION ( 'NONE',  ( 0.000000000000000000, 0.000000000000000000, 1.000000000000000000 ) ) ;
#27474 = CARTESIAN_POINT ( 'NONE',  ( 104.9999999999999716, 82.56250000273119838, 2.071067811865462627 ) ) ;
#27475 = CARTESIAN_POINT ( 'NONE',  ( 0.000000000000000000, 36.00000000000000000, 0.000000000000000000 ) ) ;
#27476 = CARTESIAN_POINT ( 'NONE',  ( 102.4999999999999858, 122.9883376334214091, 0.3865102666887284544 ) ) ;
#27477 = CARTESIAN_POINT ( 'NONE',  ( 99.14382582708707048, 123.8000000010924850, -2.066987299999999195 ) ) ;
#27478 = B_SPLINE_CURVE_WITH_KNOTS ( 'NONE', 3,
 ( #12596, #10467, #19175, #6210, #25312, #23322, #27878, #12042, #8339, #17024, #5802, #12455, #21180, #25727, #9913, #18629, #7792, #16478, #25174, #22023, #8621, #19734, #21463, #6618, #218 ),
 .UNSPECIFIED., .F., .F.,
 ( 4, 2, 2, 2, 2, 2, 2, 1, 2, 2, 2, 2, 4 ),
 ( 0.000000000000000000, 0.001301161269048799847, 0.002602322538097599693, 0.005204645076195206325, 0.007806967614292812524, 0.01040929015239041959, 0.01171045142143921532, 0.01301161269048801104, 0.01431277395953680504, 0.01561393522858560076, 0.01821625776668319222, 0.01951741903573200876, 0.02081858030478082183 ),
 .UNSPECIFIED. ) ;
#27479 = CARTESIAN_POINT ( 'NONE',  ( 133.0892609137966360, 35.99999999999997158, -13.21136010216379297 ) ) ;
#27480 = EDGE_CURVE ( 'NONE', #18468, #19839, #28167, .T. ) ;
#27481 = CARTESIAN_POINT ( 'NONE',  ( 2.493653234604083739E-15, 32.56640625216787299, 13.57481594606304576 ) ) ;
#27482 = CARTESIAN_POINT ( 'NONE',  ( 99.99999999999995737, -4.458734124999988779, 12.68750000136559208 ) ) ;
#27483 = CARTESIAN_POINT ( 'NONE',  ( 7.171391216998965312, 31.99955315621561525, -11.52591757658528948 ) ) ;
#27484 = ORIENTED_EDGE ( 'NONE', *, *, #8613, .T. ) ;
#27485 = DIRECTION ( 'NONE',  ( 0.000000000000000000, 0.000000000000000000, 1.000000000000000000 ) ) ;
#27486 = CARTESIAN_POINT ( 'NONE',  ( -13.14518615778179189, 32.07031250108393294, 5.444914386472304635 ) ) ;
#27487 = EDGE_CURVE ( 'NONE', #11744, #14666, #1501, .T. ) ;
#27488 = CARTESIAN_POINT ( 'NONE',  ( -13.57481594606304576, 31.57421875216786944, 0.000000000000000000 ) ) ;
#27489 = FACE_OUTER_BOUND ( 'NONE', #2654, .T. ) ;
#27490 = CARTESIAN_POINT ( 'NONE',  ( 96.84719886470459471, 81.56250000136559208, 3.152801135295355994 ) ) ;
#27491 = CARTESIAN_POINT ( 'NONE',  ( 74.29505027212704249, 39.66054687608393436, -9.295050272127046043 ) ) ;
#27492 = CARTESIAN_POINT ( 'NONE',  ( 99.99999999999998579, 101.5015231886685854, -50.87500000273119127 ) ) ;
#27493 = CARTESIAN_POINT ( 'NONE',  ( 103.5355339059327235, 93.87500000000000000, 3.535533905932724874 ) ) ;
#27494 = CARTESIAN_POINT ( 'NONE',  ( 101.4615807364564546, 124.4500000010924765, -1.461580736456474794 ) ) ;
#27495 = CYLINDRICAL_SURFACE ( 'NONE', #7683, 7.000000000000006217 ) ;
#27496 = CARTESIAN_POINT ( 'NONE',  ( 94.33688103937535629, 105.8855032339526758, -54.29999999453764303 ) ) ;
#27497 = CARTESIAN_POINT ( 'NONE',  ( 130.0000000000000000, 33.40976562608393863, -13.14518615778179544 ) ) ;
#27498 = EDGE_LOOP ( 'NONE', ( #3691, #3952 ) ) ;
#27499 = CARTESIAN_POINT ( 'NONE',  ( -3.797451868958014565, 54.08938259242987812, -15.00000000000000178 ) ) ;
#27500 = CARTESIAN_POINT ( 'NONE',  ( 195.0000000000000000, -7.395377635281828788, -2.255140518769849538E-14 ) ) ;
#27501 = CARTESIAN_POINT ( 'NONE',  ( 9.598844408820456309, 39.21406250216787015, -9.598844408820458085 ) ) ;
#27502 = CARTESIAN_POINT ( 'NONE',  ( 124.5550856135277087, 38.32109375108394289, 13.14518615778179722 ) ) ;
#27503 = CARTESIAN_POINT ( 'NONE',  ( 70.62287287157786864, 36.88242187716787157, -13.57481594606304753 ) ) ;
#27504 = CARTESIAN_POINT ( 'NONE',  ( 104.9952793366501709, 103.1245878333314323, -50.92499999726882010 ) ) ;
#27505 = CARTESIAN_POINT ( 'NONE',  ( 9.598844408820459861, 39.01562500216787299, 9.598844408820456309 ) ) ;
#27506 = ORIENTED_EDGE ( 'NONE', *, *, #24474, .T. ) ;
#27507 = CARTESIAN_POINT ( 'NONE',  ( 103.5355339059327093, -3.535533905932726206, 7.375000000000000000 ) ) ;
#27508 = EDGE_LOOP ( 'NONE', ( #25388, #16796, #5905, #22381 ) ) ;
#27509 = CARTESIAN_POINT ( 'NONE',  ( -13.14518615778179189, 34.45156250108394147, 5.444914386472304635 ) ) ;
#27510 = CARTESIAN_POINT ( 'NONE',  ( 200.6228728715778686, 31.82226562716787654, 13.57481594606304576 ) ) ;
#27511 = LINE ( 'NONE', #25365, #3806 ) ;
#27512 = CARTESIAN_POINT ( 'NONE',  ( 143.1451861577818079, 36.98164062608393010, -1.609821015232357215E-15 ) ) ;
#27513 = EDGE_CURVE ( 'NONE', #2259, #3615, #1775, .T. ) ;
#27514 = CYLINDRICAL_SURFACE ( 'NONE', #9952, 5.000000000000004441 ) ;
#27515 =( BOUNDED_CURVE ( )  B_SPLINE_CURVE ( 2, ( #19059, #27767, #12625, #8225, #1831, #27360, #16915, #23484, #5690 ),
 .UNSPECIFIED., .F., .F. ) 
 B_SPLINE_CURVE_WITH_KNOTS ( ( 3, 2, 2, 2, 3 ),
 ( 0.1875000000000001388, 0.1979166666666667407, 0.2083333333333333703, 0.2187499999999999722, 0.2291666666666665741 ),
 .UNSPECIFIED. ) 
 CURVE ( )  GEOMETRIC_REPRESENTATION_ITEM ( )  RATIONAL_B_SPLINE_CURVE ( ( 0.9999999999999990008, 0.9238795325112877377, 1.000000000000000000, 0.9238795325112867385, 1.000000000000000000, 0.9238795325112867385, 1.000000000000000000, 0.9238795325112872936, 0.9999999999999994449 ) ) 
 REPRESENTATION_ITEM ( '' )  );
#27516 = CARTESIAN_POINT ( 'NONE',  ( 6.944423442990538931, 31.61921458391298856, -11.16113355206744195 ) ) ;
#27517 = CARTESIAN_POINT ( 'NONE',  ( 99.99999999999998579, 94.06249999863440792, 4.458734124999981674 ) ) ;
#27518 = CARTESIAN_POINT ( 'NONE',  ( 102.0669872999999939, 123.5000000010924595, 0.8561741729129311862 ) ) ;
#27519 = CARTESIAN_POINT ( 'NONE',  ( 204.5988444088204403, 39.11484374999999858, -9.598844408820458085 ) ) ;
#27520 = EDGE_CURVE ( 'NONE', #18580, #1596, #4967, .T. ) ;
#27521 = CARTESIAN_POINT ( 'NONE',  ( 2.493653234604083739E-15, 35.64218749999999147, 13.57481594606304576 ) ) ;
#27522 = CARTESIAN_POINT ( 'NONE',  ( 95.54126587499996504, 1.387778780781445676E-14, 3.687500001365593416 ) ) ;
#27523 = CARTESIAN_POINT ( 'NONE',  ( 97.50000000000000000, 123.3499999999999943, -1.035533905932742416 ) ) ;
#27524 = CARTESIAN_POINT ( 'NONE',  ( 104.4587341249999781, 1.846868145590750521, 5.000000001365592972 ) ) ;
#27525 = CARTESIAN_POINT ( 'NONE',  ( 102.1631189606246295, 103.3426043859339103, -47.90000000546238113 ) ) ;
#27526 = CARTESIAN_POINT ( 'NONE',  ( 96.84719886470463734, 92.93749999863440792, -3.152801135295366208 ) ) ;
#27527 = CARTESIAN_POINT ( 'NONE',  ( 96.46446609406721961, -3.535533905932727539, 9.125000000000000000 ) ) ;
#27528 = CARTESIAN_POINT ( 'NONE',  ( -13.05838185645087357, 36.00000000000000711, 1.569311539113942500 ) ) ;
#27529 = CARTESIAN_POINT ( 'NONE',  ( 13.57481594606304753, 39.85898437499999858, -5.622872871577873077 ) ) ;
#27530 = EDGE_LOOP ( 'NONE', ( #4423, #22430, #15590, #1159 ) ) ;
#27531 = CARTESIAN_POINT ( 'NONE',  ( 104.4587341249999639, 81.18750000136559208, -1.442382525525748735E-14 ) ) ;
#27532 = CIRCLE ( 'NONE', #13843, 11.57481594606304398 ) ;
#27533 = CARTESIAN_POINT ( 'NONE',  ( 103.1528011352953484, 91.18749999863440792, 3.152801135295352886 ) ) ;
#27534 = ORIENTED_EDGE ( 'NONE', *, *, #2626, .T. ) ;
#27535 = VERTEX_POINT ( 'NONE', #8948 ) ;
#27536 = CARTESIAN_POINT ( 'NONE',  ( 186.2451010467579522, 50.00000000000000000, -10.39041163856320793 ) ) ;
#27537 = CARTESIAN_POINT ( 'NONE',  ( 104.4587341249999781, 1.846868145590750299, 8.250000001365592084 ) ) ;
#27538 = ORIENTED_EDGE ( 'NONE', *, *, #15207, .T. ) ;
#27539 = CARTESIAN_POINT ( 'NONE',  ( 93.46109445667491400, 114.7507929638356785, -49.57500000273120122 ) ) ;
#27540 = CARTESIAN_POINT ( 'NONE',  ( 5.444914386472297529, 33.16171875108393152, -13.14518615778179900 ) ) ;
#27541 = CARTESIAN_POINT ( 'NONE',  ( 200.6228728715778686, 39.75976562716787299, 13.57481594606304576 ) ) ;
#27542 = CARTESIAN_POINT ( 'NONE',  ( 102.1631189606246153, 116.6573956140660897, -53.60000000000000853 ) ) ;
#27543 = CARTESIAN_POINT ( 'NONE',  ( 108.0825317500000153, 110.0000000000000000, -48.12500000273119838 ) ) ;
#27544 = CARTESIAN_POINT ( 'NONE',  ( 124.5550856135277087, 38.22187500108393721, -13.14518615778179722 ) ) ;
#27545 = CARTESIAN_POINT ( 'NONE',  ( -13.14518615778179900, 39.90859375108394147, -5.444914386472297529 ) ) ;
#27546 = AXIS2_PLACEMENT_3D ( 'NONE', #16864, #27165, #1223 ) ;
#27547 = ORIENTED_EDGE ( 'NONE', *, *, #23487, .T. ) ;
#27548 = CARTESIAN_POINT ( 'NONE',  ( 74.59884440882045453, 38.91640624999999432, 9.598844408820456309 ) ) ;
#27549 = CARTESIAN_POINT ( 'NONE',  ( 51.42518405393695957, 39.56132812716787583, 5.622872871577880183 ) ) ;
#27550 = DIRECTION ( 'NONE',  ( 0.000000000000000000, 0.000000000000000000, -1.000000000000000000 ) ) ;
#27551 = CARTESIAN_POINT ( 'NONE',  ( 95.54126587499995082, -1.846868145590724986, 2.500000001365592084 ) ) ;
#27552 = CARTESIAN_POINT ( 'NONE',  ( 99.99999999999995737, 1.387778780781445676E-14, 34.79898987322334136 ) ) ;
#27553 = CARTESIAN_POINT ( 'NONE',  ( 103.1528011352953342, 3.152801135295383084, 1.312500001365592750 ) ) ;
#27554 = CARTESIAN_POINT ( 'NONE',  ( 104.4587341249999781, 81.25000000136559208, -1.846868145590750521 ) ) ;
#27555 = CARTESIAN_POINT ( 'NONE',  ( 2.414731522848535132E-15, 33.60820312608392868, 13.14518615778179544 ) ) ;
#27556 = CARTESIAN_POINT ( 'NONE',  ( 104.9999999999999716, 1.449011120738813565E-14, 7.625000002731185056 ) ) ;
#27557 = ORIENTED_EDGE ( 'NONE', *, *, #12380, .T. ) ;
#27558 = CARTESIAN_POINT ( 'NONE',  ( 9.295050272127046043, 32.51679687608393721, -9.295050272127046043 ) ) ;
#27559 = CYLINDRICAL_SURFACE ( 'NONE', #17059, 13.57481594606304576 ) ;
#27560 = CARTESIAN_POINT ( 'NONE',  ( 104.4587341249999781, 94.56249999863440792, -6.938893903907228378E-15 ) ) ;
#27561 = CARTESIAN_POINT ( 'NONE',  ( 96.46446609406721961, -3.535533905932727539, 3.250000002731184612 ) ) ;
#27562 = CARTESIAN_POINT ( 'NONE',  ( 102.4842213106612547, 122.9999999999999716, -0.1886707679707059215 ) ) ;
#27563 = EDGE_CURVE ( 'NONE', #12843, #25242, #17639, .T. ) ;
#27564 = VECTOR ( 'NONE', #25506, 1000.000000000000000 ) ;
#27565 = CARTESIAN_POINT ( 'NONE',  ( 104.9999999999999716, 1.449011120738813565E-14, 6.625000002731185944 ) ) ;
#27566 = EDGE_LOOP ( 'NONE', ( #2149, #25990 ) ) ;
#27567 = CARTESIAN_POINT ( 'NONE',  ( 51.85481384221820633, 39.11484375108393863, -5.444914386472297529 ) ) ;
#27568 = FACE_OUTER_BOUND ( 'NONE', #12391, .T. ) ;
#27569 = CARTESIAN_POINT ( 'NONE',  ( 99.99999999999995737, 1.387778780781445676E-14, 34.79898987322334136 ) ) ;
#27570 = ORIENTED_EDGE ( 'NONE', *, *, #10878, .T. ) ;
#27571 = CARTESIAN_POINT ( 'NONE',  ( 99.99999999999998579, 117.3602355696678501, -54.50000000000000000 ) ) ;
#27572 = CARTESIAN_POINT ( 'NONE',  ( -2.024627725537266443, 50.00000000051014126, -13.43320860980949227 ) ) ;
#27573 = VECTOR ( 'NONE', #334, 1000.000000000000000 ) ;
#27574 = CARTESIAN_POINT ( 'NONE',  ( 69.15728635496172672, 36.00000000000000000, -12.92256159328856135 ) ) ;
#27575 = B_SPLINE_CURVE_WITH_KNOTS ( 'NONE', 3,
 ( #2283, #11366, #10941, #20088, #566, #22085, #4414, #19653, #9248, #25931, #135, #8821, #16075, #9530 ),
 .UNSPECIFIED., .F., .F.,
 ( 4, 2, 2, 2, 2, 2, 4 ),
 ( 1.718536712070695008E-16, 0.0008152643689839393290, 0.001222896553475838087, 0.001630528737967736628, 0.002038160922459635385, 0.002445793106951534360, 0.003261057475935332309 ),
 .UNSPECIFIED. ) ;
#27576 = CARTESIAN_POINT ( 'NONE',  ( 143.5748159460630404, 33.60820312716787583, -5.622872871577873077 ) ) ;
#27577 = CARTESIAN_POINT ( 'NONE',  ( 65.00000000000000000, 40.10703125216787157, -13.57481594606304576 ) ) ;
#27578 = DIRECTION ( 'NONE',  ( -0.000000000000000000, -0.000000000000000000, -1.000000000000000000 ) ) ;
#27579 = CARTESIAN_POINT ( 'NONE',  ( 185.7049497278729575, 38.27148437608393294, -9.295050272127046043 ) ) ;
#27580 = ORIENTED_EDGE ( 'NONE', *, *, #5382, .T. ) ;
#27581 = VERTEX_POINT ( 'NONE', #2270 ) ;
#27582 = FILL_AREA_STYLE_COLOUR ( '', #23193 ) ;
#27583 = CARTESIAN_POINT ( 'NONE',  ( 101.8468681455907046, 4.458734125000016313, 13.37500000136559386 ) ) ;
#27584 = CARTESIAN_POINT ( 'NONE',  ( 9.598844408820459861, 38.12265624999999858, 9.598844408820456309 ) ) ;
#27585 = CARTESIAN_POINT ( 'NONE',  ( 74.59884440882045453, 39.80937500216786873, 9.598844408820456309 ) ) ;
#27586 = CARTESIAN_POINT ( 'NONE',  ( -8.049105076161786076E-16, 39.75976562608394005, -13.14518615778179544 ) ) ;
#27587 = CARTESIAN_POINT ( 'NONE',  ( 0.000000000000000000, 21.36169591142201440, 0.000000000000000000 ) ) ;
#27588 = AXIS2_PLACEMENT_3D ( 'NONE', #12032, #27867, #8327 ) ;
#27589 = CARTESIAN_POINT ( 'NONE',  ( 96.46446609406721961, -3.535533905932727539, 6.124999999999998224 ) ) ;
#27590 = CARTESIAN_POINT ( 'NONE',  ( 104.9999999999999716, 1.449011120738813565E-14, 34.79898987322334136 ) ) ;
#27591 = CARTESIAN_POINT ( 'NONE',  ( 106.5389055433250860, 105.2492070361643215, -46.82499999726881867 ) ) ;
#27592 = VERTEX_POINT ( 'NONE', #21790 ) ;
#27593 = CARTESIAN_POINT ( 'NONE',  ( 13.57481594606304931, 40.55351562499998863, 5.622872871577869525 ) ) ;
#27594 = CARTESIAN_POINT ( 'NONE',  ( -9.295050272127046043, 39.66054687608393436, -9.295050272127046043 ) ) ;
#27595 = CARTESIAN_POINT ( 'NONE',  ( 103.5355339059327093, 3.535533905932755072, 6.750000002731185056 ) ) ;
#27596 = CARTESIAN_POINT ( 'NONE',  ( 116.8548138422182063, 38.42031250108393436, 5.444914386472304635 ) ) ;
#27597 = EDGE_CURVE ( 'NONE', #15231, #162, #11875, .T. ) ;
#27598 = CARTESIAN_POINT ( 'NONE',  ( 70.44491438647230552, 35.54296875108393294, -13.14518615778179900 ) ) ;
#27599 = EDGE_CURVE ( 'NONE', #13106, #27745, #27716, .T. ) ;
#27600 = LINE ( 'NONE', #3795, #7959 ) ;
#27601 = CARTESIAN_POINT ( 'NONE',  ( -9.295050272127046043, 34.10429687608393579, -9.295050272127046043 ) ) ;
#27602 = CARTESIAN_POINT ( 'NONE',  ( 191.5797791878283647, 36.00000000000000711, -13.02105590829173565 ) ) ;
#27603 = VECTOR ( 'NONE', #24922, 1000.000000000000000 ) ;
#27604 = CARTESIAN_POINT ( 'NONE',  ( 98.96446609406727646, 124.1500000021849672, -2.499999999999997780 ) ) ;
#27605 = CARTESIAN_POINT ( 'NONE',  ( 104.3262379212492590, 115.9545556584642867, -48.70000000000000284 ) ) ;
#27606 = CARTESIAN_POINT ( 'NONE',  ( 116.4251840539369738, 40.25585937499999289, 5.622872871577880183 ) ) ;
#27607 = ORIENTED_EDGE ( 'NONE', *, *, #24837, .T. ) ;
#27608 = DIRECTION ( 'NONE',  ( -0.000000000000000000, -1.000000000000000000, -0.000000000000000000 ) ) ;
#27609 = CARTESIAN_POINT ( 'NONE',  ( 9.295050272127047819, 40.05742187608392868, 9.295050272127046043 ) ) ;
#27610 = VECTOR ( 'NONE', #1214, 1000.000000000000000 ) ;
#27611 = FACE_BOUND ( 'NONE', #5883, .T. ) ;
#27612 = CARTESIAN_POINT ( 'NONE',  ( 99.99999999999998579, 123.2069999999781515, -2.499999999999997780 ) ) ;
#27613 = EDGE_CURVE ( 'NONE', #3340, #1089, #16794, .T. ) ;
#27614 = CARTESIAN_POINT ( 'NONE',  ( 97.93301270000000613, 123.1500000010924651, -9.540979117872439019E-15 ) ) ;
#27615 = CARTESIAN_POINT ( 'NONE',  ( 97.93301270000000613, 123.9500000010924765, -9.540979117872439019E-15 ) ) ;
#27616 = CARTESIAN_POINT ( 'NONE',  ( 181.4251840539369596, 39.46210937716787726, -5.622872871577872189 ) ) ;
#27617 = CARTESIAN_POINT ( 'NONE',  ( 101.8468681455906903, -4.458734124999987891, 11.75000000136559208 ) ) ;
#27618 = CARTESIAN_POINT ( 'NONE',  ( -9.598844408820454532, 32.46718750216787441, 9.598844408820459861 ) ) ;
#27619 = EDGE_LOOP ( 'NONE', ( #6677, #10507, #20285, #8317, #22622, #583, #19780, #22587, #15700, #2201, #8405, #26129, #9716 ) ) ;
#27620 = CARTESIAN_POINT ( 'NONE',  ( 99.99999999999998579, 124.1000000021849416, -2.499999999999997780 ) ) ;
#27621 = CARTESIAN_POINT ( 'NONE',  ( 6.944423624769117787, 31.75150628229955529, -11.16113343896966370 ) ) ;
#27622 = CARTESIAN_POINT ( 'NONE',  ( 94.99999999999995737, 1.387778780781445676E-14, 9.000000000000000000 ) ) ;
#27623 = CARTESIAN_POINT ( 'NONE',  ( -5.622872871577873077, 31.42539062716787157, -13.57481594606304753 ) ) ;
#27624 = CARTESIAN_POINT ( 'NONE',  ( 195.0000000000000000, 36.53515625216787299, 13.57481594606304576 ) ) ;
#27625 = CARTESIAN_POINT ( 'NONE',  ( 95.54126587499995082, 81.37500000136563472, -1.846868145590750077 ) ) ;
#27626 = CARTESIAN_POINT ( 'NONE',  ( 70.44491438647230552, 37.03125000108393294, 13.14518615778179189 ) ) ;
#27627 = CARTESIAN_POINT ( 'NONE',  ( 95.00472066334982912, 116.8754121666685393, -47.67500000273120264 ) ) ;
#27628 =( BOUNDED_CURVE ( )  B_SPLINE_CURVE ( 2, ( #20576, #27142, #7594, #24985, #5466, #14135, #22856, #21414, #19267 ),
 .UNSPECIFIED., .F., .F. ) 
 B_SPLINE_CURVE_WITH_KNOTS ( ( 3, 2, 2, 2, 3 ),
 ( 0.1875000000000001388, 0.1979166666666667407, 0.2083333333333333703, 0.2187499999999999722, 0.2291666666666665741 ),
 .UNSPECIFIED. ) 
 CURVE ( )  GEOMETRIC_REPRESENTATION_ITEM ( )  RATIONAL_B_SPLINE_CURVE ( ( 0.9999999999999990008, 0.9238795325112877377, 1.000000000000000000, 0.9238795325112867385, 1.000000000000000000, 0.9238795325112867385, 1.000000000000000000, 0.9238795325112872936, 0.9999999999999994449 ) ) 
 REPRESENTATION_ITEM ( '' )  );
#27629 = CARTESIAN_POINT ( 'NONE',  ( 100.8561741729129153, 123.7000000010924765, -2.066987299999999195 ) ) ;
#27630 = CARTESIAN_POINT ( 'NONE',  ( 97.83688103937535629, 116.6573956140660897, -52.89999999453764445 ) ) ;
#27631 = CARTESIAN_POINT ( 'NONE',  ( 124.3771271284221314, 39.56132812499999574, 13.57481594606304753 ) ) ;
#27632 = ADVANCED_FACE ( 'NONE', ( #13636 ), #5251, .F. ) ;
#27633 = ORIENTED_EDGE ( 'NONE', *, *, #10878, .F. ) ;
#27634 = CARTESIAN_POINT ( 'NONE',  ( 107.0000000000000000, 110.0000000000000000, -51.49999999453763877 ) ) ;
#27635 = CARTESIAN_POINT ( 'NONE',  ( -9.295050272127044266, 40.05742187608393579, 9.295050272127047819 ) ) ;
#27636 = CARTESIAN_POINT ( 'NONE',  ( 95.54126587499996504, 80.43750000136559208, -1.387778780781445676E-14 ) ) ;
#27637 = CARTESIAN_POINT ( 'NONE',  ( 135.4449143864723055, 39.21406250108392300, 13.14518615778179189 ) ) ;
#27638 = CARTESIAN_POINT ( 'NONE',  ( 65.00000000000000000, 35.74140625216787015, 13.57481594606304576 ) ) ;
#27639 = CARTESIAN_POINT ( 'NONE',  ( 97.50236033167490746, 117.6869444889999841, -52.02499999726882862 ) ) ;
#27640 = CARTESIAN_POINT ( 'NONE',  ( 2.493653234604083739E-15, 37.32890625216786873, 13.57481594606304576 ) ) ;
#27641 = ORIENTED_EDGE ( 'NONE', *, *, #23271, .T. ) ;
#27642 = EDGE_CURVE ( 'NONE', #15131, #25968, #19707, .T. ) ;
#27643 = CARTESIAN_POINT ( 'NONE',  ( 104.9999999999999574, -2.071067811865462627, 10.43749999999999822 ) ) ;
#27644 = EDGE_LOOP ( 'NONE', ( #12851, #6596, #15799, #7962 ) ) ;
#27645 = CARTESIAN_POINT ( 'NONE',  ( -5.444914386472297529, 32.66562500108393863, -13.14518615778179900 ) ) ;
#27646 = CARTESIAN_POINT ( 'NONE',  ( 185.7049497278729575, 36.48554687608393721, -9.295050272127046043 ) ) ;
#27647 = AXIS2_PLACEMENT_3D ( 'NONE', #18747, #16603, #6060 ) ;
#27648 = DIRECTION ( 'NONE',  ( 0.000000000000000000, 1.000000000000000000, 0.000000000000000000 ) ) ;
#27649 = CARTESIAN_POINT ( 'NONE',  ( 116.8548138422182205, 38.12265625108393863, -5.444914386472297529 ) ) ;
#27650 = CARTESIAN_POINT ( 'NONE',  ( 99.99999999999998579, 123.7000000021849502, 2.499999999999978684 ) ) ;
#27651 = DIRECTION ( 'NONE',  ( 0.000000000000000000, 0.000000000000000000, 1.000000000000000000 ) ) ;
#27652 = CARTESIAN_POINT ( 'NONE',  ( 96.84719886470463734, 94.68749999863440792, -3.152801135295366208 ) ) ;
#27653 = CARTESIAN_POINT ( 'NONE',  ( 95.67376207875072680, 104.0454443415356991, -48.70000000000000995 ) ) ;
#27654 = CARTESIAN_POINT ( 'NONE',  ( -13.14518615778179544, 38.96601562608393721, 0.000000000000000000 ) ) ;
#27655 = CARTESIAN_POINT ( 'NONE',  ( 195.0000000000000000, 39.21406249999999716, -13.57481594606304576 ) ) ;
#27656 = PLANE ( 'NONE',  #8176 ) ;
#27657 = CARTESIAN_POINT ( 'NONE',  ( 101.8468681455906903, -4.458734124999987891, 3.000000001365592528 ) ) ;
#27658 = CARTESIAN_POINT ( 'NONE',  ( 65.00000000000000000, 39.56132812608393579, -13.14518615778179544 ) ) ;
#27659 = CARTESIAN_POINT ( 'NONE',  ( 98.15313185440923860, 4.458734125000016313, 4.250000001365592084 ) ) ;
#27660 = CARTESIAN_POINT ( 'NONE',  ( 95.67376207875072680, 104.0454443415356991, -50.20000000546238539 ) ) ;
#27661 = CARTESIAN_POINT ( 'NONE',  ( 99.99999999999998579, 94.81249999863440792, -4.458734124999994997 ) ) ;
#27662 = CARTESIAN_POINT ( 'NONE',  ( -2.297960586007286476, 36.00000000000000000, 12.97104423350697466 ) ) ;
#27663 = CARTESIAN_POINT ( 'NONE',  ( 9.598844408820456309, 39.90859374999999432, -9.598844408820458085 ) ) ;
#27664 = CARTESIAN_POINT ( 'NONE',  ( 120.7049497278729575, 40.65273437608393436, -9.295050272127046043 ) ) ;
#27665 = ORIENTED_EDGE ( 'NONE', *, *, #10172, .T. ) ;
#27666 = CARTESIAN_POINT ( 'NONE',  ( 95.54126587499995082, 83.62500000136560629, -1.846868145590750077 ) ) ;
#27667 = AXIS2_PLACEMENT_3D ( 'NONE', #1668, #7928, #6215 ) ;
#27668 = CARTESIAN_POINT ( 'NONE',  ( 97.50000000000000000, 124.2500000021849900, -1.035533905932742416 ) ) ;
#27669 = EDGE_LOOP ( 'NONE', ( #8305, #19761 ) ) ;
#27670 = ORIENTED_EDGE ( 'NONE', *, *, #2382, .F. ) ;
#27671 = CARTESIAN_POINT ( 'NONE',  ( 131.6052718765765803, 53.60388944777321996, -15.00000000000000355 ) ) ;
#27672 = EDGE_CURVE ( 'NONE', #9425, #21442, #1336, .T. ) ;
#27673 = CARTESIAN_POINT ( 'NONE',  ( 103.1528011352953342, -3.152801135295355106, 7.062500001365592972 ) ) ;
#27674 = ORIENTED_EDGE ( 'NONE', *, *, #15225, .F. ) ;
#27675 = CARTESIAN_POINT ( 'NONE',  ( 104.9952793366501851, 116.8754121666685393, -48.07500000273119412 ) ) ;
#27676 =( BOUNDED_CURVE ( )  B_SPLINE_CURVE ( 2, ( #5442, #9705, #20553, #22544, #20693 ),
 .UNSPECIFIED., .F., .T. ) 
 B_SPLINE_CURVE_WITH_KNOTS ( ( 3, 2, 3 ),
 ( 0.000000000000000000, 0.04166666666666653945, 0.08333333333333307891 ),
 .UNSPECIFIED. ) 
 CURVE ( )  GEOMETRIC_REPRESENTATION_ITEM ( )  RATIONAL_B_SPLINE_CURVE ( ( 1.000000000000000000, 0.9238795325112867385, 1.000000000000000000, 0.9238795325112871826, 0.9999999999999995559 ) ) 
 REPRESENTATION_ITEM ( '' )  );
#27677 = CARTESIAN_POINT ( 'NONE',  ( -9.295050272127044266, 34.30273437608393294, 9.295050272127047819 ) ) ;
#27678 = CARTESIAN_POINT ( 'NONE',  ( 181.4251840539369596, 38.66835937716786731, -5.622872871577873077 ) ) ;
#27679 = CARTESIAN_POINT ( 'NONE',  ( -13.14518615778179544, 39.75976562608393294, 0.000000000000000000 ) ) ;
#27680 = CARTESIAN_POINT ( 'NONE',  ( 108.0825317500000011, 107.3738262389971680, -48.22500000273118559 ) ) ;
#27681 = CARTESIAN_POINT ( 'NONE',  ( 102.1631189606246295, 103.3426043859339103, -51.40000000000000568 ) ) ;
#27682 = CARTESIAN_POINT ( 'NONE',  ( 116.8548138422182205, 39.11484375108393863, -5.444914386472297529 ) ) ;
#27683 = CARTESIAN_POINT ( 'NONE',  ( -13.14518615778179544, 33.40976562608393863, 0.000000000000000000 ) ) ;
#27684 = ORIENTED_EDGE ( 'NONE', *, *, #22737, .F. ) ;
#27685 = CARTESIAN_POINT ( 'NONE',  ( 65.00000000000000000, 39.21406249999999716, -13.57481594606304576 ) ) ;
#27686 = DIRECTION ( 'NONE',  ( 0.000000000000000000, -1.000000000000000000, 0.000000000000000000 ) ) ;
#27687 = CIRCLE ( 'NONE', #27707, 5.000000000000004441 ) ;
#27688 = CARTESIAN_POINT ( 'NONE',  ( 204.4320061696341497, 36.00000000000001421, 9.391769196590237456 ) ) ;
#27689 = CARTESIAN_POINT ( 'NONE',  ( 98.15313185440925281, -4.458734124999987891, 3.625000001365591640 ) ) ;
#27690 = CARTESIAN_POINT ( 'NONE',  ( -13.14518615778179189, 33.65781250108393152, 5.444914386472304635 ) ) ;
#27691 = AXIS2_PLACEMENT_3D ( 'NONE', #5293, #13957, #13274 ) ;
#27692 = CARTESIAN_POINT ( 'NONE',  ( 99.99999999999995737, -4.458734124999988779, 1.937500001365591640 ) ) ;
#27693 = CARTESIAN_POINT ( 'NONE',  ( 103.1528011352953342, 83.06250000136560629, 3.152801135295355106 ) ) ;
#27694 = CARTESIAN_POINT ( 'NONE',  ( 5.444914386472297529, 33.16171875108393152, -13.14518615778179900 ) ) ;
#27695 = CARTESIAN_POINT ( 'NONE',  ( -13.14518615778179544, 40.75195312608393294, 0.000000000000000000 ) ) ;
#27696 = CARTESIAN_POINT ( 'NONE',  ( 13.57481594606304753, 39.16445312716788152, -5.622872871577873966 ) ) ;
#27697 = ORIENTED_EDGE ( 'NONE', *, *, #9846, .F. ) ;
#27698 = DIRECTION ( 'NONE',  ( 0.000000000000000000, 1.000000000000000000, 0.000000000000000000 ) ) ;
#27699 = CARTESIAN_POINT ( 'NONE',  ( 98.53841926354351699, 123.6500000010924794, -1.461580736456474794 ) ) ;
#27700 = CARTESIAN_POINT ( 'NONE',  ( 99.99999999999998579, 94.81249999863440792, -4.458734124999994997 ) ) ;
#27701 = CARTESIAN_POINT ( 'NONE',  ( 181.9040934463640156, 35.99999999999999289, 1.137167824541468031 ) ) ;
#27702 = CARTESIAN_POINT ( 'NONE',  ( 101.6707202882716388, 122.9999999999999574, -1.633471722151653704 ) ) ;
#27703 = CARTESIAN_POINT ( 'NONE',  ( 95.00000000000000000, 93.43749999999998579, -2.071067811865479058 ) ) ;
#27704 = EDGE_LOOP ( 'NONE', ( #22915, #9006 ) ) ;
#27705 = CARTESIAN_POINT ( 'NONE',  ( 59.55508561352770158, 37.72578125108394431, 13.14518615778179722 ) ) ;
#27706 = CARTESIAN_POINT ( 'NONE',  ( 97.92893218813449607, 83.31250000273118417, 4.999999999999981348 ) ) ;
#27707 = AXIS2_PLACEMENT_3D ( 'NONE', #7092, #9662, #27215 ) ;
#27708 = CARTESIAN_POINT ( 'NONE',  ( 200.4449143864723055, 32.26875000108393721, 13.14518615778179189 ) ) ;
#27709 = EDGE_LOOP ( 'NONE', ( #20372, #24203, #25006, #25864 ) ) ;
#27710 = CARTESIAN_POINT ( 'NONE',  ( 104.9999999999999716, 1.449011120738813565E-14, 1.625000002731184834 ) ) ;
#27711 = CARTESIAN_POINT ( 'NONE',  ( 120.4011555911795455, 37.92421874999999432, 9.598844408820459861 ) ) ;
#27712 = CIRCLE ( 'NONE', #24080, 5.000000000000000888 ) ;
#27713 = CARTESIAN_POINT ( 'NONE',  ( 139.5988444088204687, 36.63437500216787157, 9.598844408820456309 ) ) ;
#27714 =( BOUNDED_CURVE ( )  B_SPLINE_CURVE ( 2, ( #776, #26862, #27002, #5189, #13852, #22577, #3046, #11715, #9591 ),
 .UNSPECIFIED., .F., .F. ) 
 B_SPLINE_CURVE_WITH_KNOTS ( ( 3, 2, 2, 2, 3 ),
 ( 0.08333333333333389770, 0.1250000000000003886, 0.1666666666666668517, 0.2083333333333333426, 0.2499999999999998335 ),
 .UNSPECIFIED. ) 
 CURVE ( )  GEOMETRIC_REPRESENTATION_ITEM ( )  RATIONAL_B_SPLINE_CURVE ( ( 0.9999999999999990008, 0.9238795325112877377, 1.000000000000000000, 0.9238795325112867385, 1.000000000000000000, 0.9238795325112867385, 1.000000000000000000, 0.9238795325112870716, 0.9999999999999996669 ) ) 
 REPRESENTATION_ITEM ( '' )  );
#27715 = CARTESIAN_POINT ( 'NONE',  ( 139.5988444088204403, 36.03906250216787299, -9.598844408820458085 ) ) ;
#27716 =( BOUNDED_CURVE ( )  B_SPLINE_CURVE ( 2, ( #19359, #8529, #2960, #7225, #26490, #24632, #6947, #11209, #9234 ),
 .UNSPECIFIED., .F., .F. ) 
 B_SPLINE_CURVE_WITH_KNOTS ( ( 3, 2, 2, 2, 3 ),
 ( 0.2499999999999999445, 0.2589285714285713969, 0.2678571428571427937, 0.2767857142857143016, 0.2857142857142856984 ),
 .UNSPECIFIED. ) 
 CURVE ( )  GEOMETRIC_REPRESENTATION_ITEM ( )  RATIONAL_B_SPLINE_CURVE ( ( 1.000000000000000444, 0.9238795325112862944, 1.000000000000000000, 0.9238795325112867385, 1.000000000000000000, 0.9238795325112867385, 1.000000000000000000, 0.9238795325112867385, 1.000000000000000000 ) ) 
 REPRESENTATION_ITEM ( '' )  );
#27717 = CARTESIAN_POINT ( 'NONE',  ( 55.70494972787295751, 39.26367187608393294, 9.295050272127047819 ) ) ;
#27718 = PLANE ( 'NONE',  #8687 ) ;
#27719 = CARTESIAN_POINT ( 'NONE',  ( 204.2950502721270425, 38.86679687608393863, -9.295050272127046043 ) ) ;
#27720 = ORIENTED_EDGE ( 'NONE', *, *, #21918, .F. ) ;
#27721 = EDGE_CURVE ( 'NONE', #18097, #28082, #986, .T. ) ;
#27722 = ORIENTED_EDGE ( 'NONE', *, *, #3446, .F. ) ;
#27723 = DIRECTION ( 'NONE',  ( -0.000000000000000000, -1.000000000000000000, -0.000000000000000000 ) ) ;
#27724 = CARTESIAN_POINT ( 'NONE',  ( -5.622872871577947684, 40.05742187499998863, -13.57481594606297293 ) ) ;
#27725 = FACE_OUTER_BOUND ( 'NONE', #2467, .T. ) ;
#27726 = FACE_OUTER_BOUND ( 'NONE', #22926, .T. ) ;
#27727 = CARTESIAN_POINT ( 'NONE',  ( 13.14518615778179544, 40.35507812608393863, -1.609821015232357215E-15 ) ) ;
#27728 = DIRECTION ( 'NONE',  ( -1.000000000000000000, 0.000000000000000000, 0.000000000000000000 ) ) ;
#27729 = CIRCLE ( 'NONE', #13121, 13.57481594606304576 ) ;
#27730 = CARTESIAN_POINT ( 'NONE',  ( 6.106658654947462850, 36.00000000000003553, 11.74215035806574647 ) ) ;
#27731 = FACE_OUTER_BOUND ( 'NONE', #6548, .T. ) ;
#27732 = CARTESIAN_POINT ( 'NONE',  ( 143.5748159460630688, 32.66562499999999858, -1.662435489736055892E-15 ) ) ;
#27733 = VERTEX_POINT ( 'NONE', #26636 ) ;
#27734 = CARTESIAN_POINT ( 'NONE',  ( -13.57481594606304576, 40.99999999999999289, 0.000000000000000000 ) ) ;
#27735 = CARTESIAN_POINT ( 'NONE',  ( -13.57481594606304576, 31.57421875216786944, 0.000000000000000000 ) ) ;
#27736 = CARTESIAN_POINT ( 'NONE',  ( 103.5355339059327093, -3.535533905932726206, 0.5000000027311855000 ) ) ;
#27737 = CARTESIAN_POINT ( 'NONE',  ( 139.2950502721270425, 40.25585937608393294, 9.295050272127046043 ) ) ;
#27738 = CARTESIAN_POINT ( 'NONE',  ( 59.55508561352770158, 38.32109375108394289, 13.14518615778179722 ) ) ;
#27739 = CARTESIAN_POINT ( 'NONE',  ( 181.8548138422182205, 32.61601562608393579, 0.000000000000000000 ) ) ;
#27740 = DIRECTION ( 'NONE',  ( 0.000000000000000000, -0.000000000000000000, 1.000000000000000000 ) ) ;
#27741 = CARTESIAN_POINT ( 'NONE',  ( -8.049105076161786076E-16, 34.00507812608393721, -13.14518615778179544 ) ) ;
#27742 = CARTESIAN_POINT ( 'NONE',  ( 103.5355339059327093, -3.535533905932726206, 9.500000002731184168 ) ) ;
#27743 = FACE_OUTER_BOUND ( 'NONE', #21462, .T. ) ;
#27744 = DIRECTION ( 'NONE',  ( 0.000000000000000000, 0.000000000000000000, -1.000000000000000000 ) ) ;
#27745 = VERTEX_POINT ( 'NONE', #3111 ) ;
#27746 = VECTOR ( 'NONE', #12191, 1000.000000000000000 ) ;
#27747 = CARTESIAN_POINT ( 'NONE',  ( 2.414731522848535132E-15, 38.37070312608393152, 13.14518615778179544 ) ) ;
#27748 = CARTESIAN_POINT ( 'NONE',  ( -3.865414375413190218, 54.10683252460146520, 14.99999999999999289 ) ) ;
#27749 = CARTESIAN_POINT ( 'NONE',  ( 97.50000000000000000, 125.0000000000000000, -9.540979117872439019E-15 ) ) ;
#27750 = CARTESIAN_POINT ( 'NONE',  ( 102.0669872999999797, 123.5500000010924708, -9.794112055954760458E-15 ) ) ;
#27751 = CARTESIAN_POINT ( 'NONE',  ( 99.99999999999998579, 124.1500000010924651, 2.066987299999980099 ) ) ;
#27752 = CARTESIAN_POINT ( 'NONE',  ( 101.8468681455906903, 4.458734125000016313, 11.12500000136559386 ) ) ;
#27753 = DIRECTION ( 'NONE',  ( 0.000000000000000000, 0.000000000000000000, -1.000000000000000000 ) ) ;
#27754 = ORIENTED_EDGE ( 'NONE', *, *, #17170, .T. ) ;
#27755 = CARTESIAN_POINT ( 'NONE',  ( 107.0000000000000142, 110.0000000000000000, -53.00000000000000711 ) ) ;
#27756 = CARTESIAN_POINT ( 'NONE',  ( -13.14518615778179900, 31.97109375108393436, -5.444914386472297529 ) ) ;
#27757 = CARTESIAN_POINT ( 'NONE',  ( -8.049105076161786076E-16, 32.41757812608393863, -13.14518615778179544 ) ) ;
#27758 = VECTOR ( 'NONE', #16451, 1000.000000000000000 ) ;
#27759 = CARTESIAN_POINT ( 'NONE',  ( 13.57481594606304576, 33.55859375216787299, -1.662435489736055892E-15 ) ) ;
#27760 = CARTESIAN_POINT ( 'NONE',  ( 195.0000000000000000, 36.13828125216787157, -13.57481594606304576 ) ) ;
#27761 = CARTESIAN_POINT ( 'NONE',  ( 98.15313185440925281, 79.62500000136560629, 4.458734124999987891 ) ) ;
#27762 = CARTESIAN_POINT ( 'NONE',  ( 70.44491438647230552, 38.61875000108393152, 13.14518615778179189 ) ) ;
#27763 = ADVANCED_FACE ( 'NONE', ( #20210 ), #4831, .T. ) ;
#27764 = CARTESIAN_POINT ( 'NONE',  ( 102.4976396683250925, 117.6869444889999841, -45.97500000273119269 ) ) ;
#27765 = CARTESIAN_POINT ( 'NONE',  ( 100.0000000000000000, 110.0000000000000000, -55.00000000000000711 ) ) ;
#27766 = CARTESIAN_POINT ( 'NONE',  ( 100.8561741729129295, 123.4000000010924794, 2.066987299999979211 ) ) ;
#27767 = CARTESIAN_POINT ( 'NONE',  ( 135.6228728715779255, 39.16445312500000142, -13.57481594606299247 ) ) ;
#27768 = CARTESIAN_POINT ( 'NONE',  ( 97.83688103937535629, 116.6573956140660897, -48.89999999453763735 ) ) ;
#27769 = CARTESIAN_POINT ( 'NONE',  ( 124.5550856135277087, 32.16953125108393152, 13.14518615778179722 ) ) ;
#27770 = ORIENTED_EDGE ( 'NONE', *, *, #10559, .F. ) ;
#27771 = CARTESIAN_POINT ( 'NONE',  ( 104.3262379212492448, 104.0454443415356991, -51.79999999453762882 ) ) ;
#27772 = CARTESIAN_POINT ( 'NONE',  ( 13.14518615778179544, 39.56132812608393579, -1.609821015232357215E-15 ) ) ;
#27773 = CARTESIAN_POINT ( 'NONE',  ( 103.1528011352953342, 81.06250000136559208, -3.152801135295383084 ) ) ;
#27774 = CARTESIAN_POINT ( 'NONE',  ( 95.00000000000000000, 94.56250000000000000, 2.071067811865463959 ) ) ;
#27775 = CARTESIAN_POINT ( 'NONE',  ( 74.59884440882045453, 36.63437500216787157, 9.598844408820456309 ) ) ;
#27776 = DIRECTION ( 'NONE',  ( 0.000000000000000000, -0.5735764363510443831, 0.8191520442889929088 ) ) ;
#27777 = CARTESIAN_POINT ( 'NONE',  ( -9.598844408820458085, 35.44375000216787441, -9.598844408820458085 ) ) ;
#27778 = ORIENTED_EDGE ( 'NONE', *, *, #17150, .T. ) ;
#27779 = CARTESIAN_POINT ( 'NONE',  ( 104.9999999999999574, 2.071067811865491937, 3.562500000000000000 ) ) ;
#27780 = CARTESIAN_POINT ( 'NONE',  ( 0.000000000000000000, 50.00000000000000000, 0.000000000000000000 ) ) ;
#27781 = EDGE_CURVE ( 'NONE', #25436, #9633, #8148, .T. ) ;
#27782 = CARTESIAN_POINT ( 'NONE',  ( 208.1451861577818079, 36.18789062608393436, -1.609821015232357215E-15 ) ) ;
#27783 = CARTESIAN_POINT ( 'NONE',  ( 96.46446609406721961, 3.535533905932755072, 14.00000000273118594 ) ) ;
#27784 = CARTESIAN_POINT ( 'NONE',  ( 143.1451861577818363, 39.31328125108392868, 5.444914386472293977 ) ) ;
#27785 = EDGE_CURVE ( 'NONE', #28009, #439, #19043, .T. ) ;
#27786 = DIRECTION ( 'NONE',  ( -0.000000000000000000, -1.000000000000000000, -0.000000000000000000 ) ) ;
#27787 = CARTESIAN_POINT ( 'NONE',  ( 135.6228728715779539, 37.27929687499999289, 13.57481594606297115 ) ) ;
#27788 = CARTESIAN_POINT ( 'NONE',  ( 95.54126587499999346, 94.87499999863440792, 1.846868145590722543 ) ) ;
#27789 =( BOUNDED_SURFACE ( )  B_SPLINE_SURFACE ( 1, 2, ( 
 ( #14076, #26648, #11791, #20515, #16221, #997, #9665, #18369, #4982, #9806, #22796, #25066, #7096, #15794, #22363, #24497, #11505, #20223, #706, #9380, #18077, #26791, #7236, #24646, #5119, #13784, #22506, #20370, #25201, #1414, #7815, #6094, #25610, #1555, #10208, #27492, #23621, #23069, #3546, #14493, #23481, #27901, #12349, #25338, #18785, #12621, #25751, #16645, #23345, #20930, #16781, #3818, #12203, #21205, #14900, #12478, #5824, #18918, #9937, #12068, #7948, #3961, #1688, #21347, #23210, #20792, #1273, #27627, #25480, #10073, #3685, #1825, #19198, #21067, #10491, #8085, #10347, #5687, #27358, #14626, #5958, #16912, #19054, #14761, #27764, #18652, #16507, #8361, #8222, #17047, #6233, #14353, #26320, #4516, #15466, #12761, #11045, #8924, #28038, #2521, #17612 ),
 ( #19755, #12892, #19900, #24037, #4658, #384, #9068, #6781, #24180, #15039, #13031, #13320, #25897, #21768, #19616, #8505, #22045, #11182, #26172, #21622, #6920, #21481, #17763, #26466, #15613, #26030, #2245, #10907, #6367, #1961, #4098, #237, #2098, #10630, #13173, #19336, #17190, #23756, #4234, #10766, #19477, #101, #28176, #8647, #8783, #17470, #17337, #6501, #15177, #23896, #4375, #6639, #15324, #21912, #2387, #24607, #18332, #27039, #7485, #16180, #671, #18475, #24745, #5367, #11753, #816, #9345, #9484, #26610, #5085, #11606, #11891, #24888, #22616, #14034, #957, #7195, #22759, #18186, #22330, #526, #22472, #15755, #13747, #2665, #15891, #27183, #11326, #4943, #3224, #24315, #7056, #9627, #7634, #26896, #20615, #2935, #20187, #22185, #9766, #20329 ) ),
 .UNSPECIFIED., .F., .F., .F. ) 
 B_SPLINE_SURFACE_WITH_KNOTS ( ( 2, 2 ),
 ( 3, 2, 2, 2, 2, 2, 2, 2, 2, 2, 2, 2, 2, 2, 2, 2, 2, 2, 2, 2, 2, 2, 2, 2, 2, 2, 2, 2, 2, 2, 2, 2, 2, 2, 2, 2, 2, 2, 2, 2, 2, 2, 2, 2, 2, 2, 2, 2, 2, 2, 3 ),
 ( 0.000000000000000000, 1.000000000000000000 ),
 ( 0.000000000000000000, 0.02000000000000000042, 0.04000000000000000083, 0.05999999999999999778, 0.08000000000000000167, 0.1000000000000000056, 0.1199999999999999956, 0.1400000000000000133, 0.1600000000000000033, 0.1799999999999999933, 0.2000000000000000111, 0.2200000000000000011, 0.2399999999999999911, 0.2600000000000000089, 0.2800000000000000266, 0.2999999999999999889, 0.3200000000000000067, 0.3400000000000000244, 0.3599999999999999867, 0.3800000000000000044, 0.4000000000000000222, 0.4199999999999999845, 0.4400000000000000022, 0.4600000000000000200, 0.4799999999999999822, 0.5000000000000000000, 0.5200000000000000178, 0.5400000000000000355, 0.5600000000000000533, 0.5799999999999999600, 0.5999999999999999778, 0.6199999999999999956, 0.6400000000000000133, 0.6600000000000000311, 0.6800000000000000488, 0.6999999999999999556, 0.7199999999999999734, 0.7399999999999999911, 0.7600000000000000089, 0.7800000000000000266, 0.8000000000000000444, 0.8199999999999999512, 0.8399999999999999689, 0.8599999999999999867, 0.8800000000000000044, 0.9000000000000000222, 0.9200000000000000400, 0.9399999999999999467, 0.9599999999999999645, 0.9799999999999999822, 1.000000000000000000 ),
 .UNSPECIFIED. ) 
 GEOMETRIC_REPRESENTATION_ITEM ( )  RATIONAL_B_SPLINE_SURFACE ( (
 ( 1.000000000000000000, 0.9510565162951535312, 1.000000000000000000, 0.9510565162951535312, 1.000000000000000000, 0.9510565162951535312, 1.000000000000000000, 0.9510565162951535312, 1.000000000000000000, 0.9510565162951535312, 1.000000000000000000, 0.9510565162951535312, 1.000000000000000000, 0.9510565162951535312, 1.000000000000000000, 0.9510565162951535312, 1.000000000000000000, 0.9510565162951535312, 1.000000000000000000, 0.9510565162951535312, 1.000000000000000000, 0.9510565162951535312, 1.000000000000000000, 0.9510565162951535312, 1.000000000000000000, 0.9510565162951535312, 1.000000000000000000, 0.9510565162951535312, 1.000000000000000000, 0.9510565162951535312, 1.000000000000000000, 0.9510565162951535312, 1.000000000000000000, 0.9510565162951535312, 1.000000000000000000, 0.9510565162951535312, 1.000000000000000000, 0.9510565162951535312, 1.000000000000000000, 0.9510565162951535312, 1.000000000000000000, 0.9510565162951535312, 1.000000000000000000, 0.9510565162951535312, 1.000000000000000000, 0.9510565162951535312, 1.000000000000000000, 0.9510565162951535312, 1.000000000000000000, 0.9510565162951535312, 1.000000000000000000, 0.9510565162951535312, 1.000000000000000000, 0.9510565162951535312, 1.000000000000000000, 0.9510565162951535312, 1.000000000000000000, 0.9510565162951535312, 1.000000000000000000, 0.9510565162951535312, 1.000000000000000000, 0.9510565162951535312, 1.000000000000000000, 0.9510565162951535312, 1.000000000000000000, 0.9510565162951535312, 1.000000000000000000, 0.9510565162951535312, 1.000000000000000000, 0.9510565162951535312, 1.000000000000000000, 0.9510565162951535312, 1.000000000000000000, 0.9510565162951535312, 1.000000000000000000, 0.9510565162951535312, 1.000000000000000000, 0.9510565162951535312, 1.000000000000000000, 0.9510565162951535312, 1.000000000000000000, 0.9510565162951535312, 1.000000000000000000, 0.9510565162951535312, 1.000000000000000000, 0.9510565162951535312, 1.000000000000000000, 0.9510565162951535312, 1.000000000000000000, 0.9510565162951535312, 1.000000000000000000, 0.9510565162951535312, 1.000000000000000000, 0.9510565162951535312, 1.000000000000000000, 0.9510565162951535312, 1.000000000000000000, 0.9510565162951535312, 1.000000000000000000, 0.9510565162951535312, 1.000000000000000000),
 ( 1.000000000000000000, 0.9510565162951535312, 1.000000000000000000, 0.9510565162951535312, 1.000000000000000000, 0.9510565162951535312, 1.000000000000000000, 0.9510565162951535312, 1.000000000000000000, 0.9510565162951535312, 1.000000000000000000, 0.9510565162951535312, 1.000000000000000000, 0.9510565162951535312, 1.000000000000000000, 0.9510565162951535312, 1.000000000000000000, 0.9510565162951535312, 1.000000000000000000, 0.9510565162951535312, 1.000000000000000000, 0.9510565162951535312, 1.000000000000000000, 0.9510565162951535312, 1.000000000000000000, 0.9510565162951535312, 1.000000000000000000, 0.9510565162951535312, 1.000000000000000000, 0.9510565162951535312, 1.000000000000000000, 0.9510565162951535312, 1.000000000000000000, 0.9510565162951535312, 1.000000000000000000, 0.9510565162951535312, 1.000000000000000000, 0.9510565162951535312, 1.000000000000000000, 0.9510565162951535312, 1.000000000000000000, 0.9510565162951535312, 1.000000000000000000, 0.9510565162951535312, 1.000000000000000000, 0.9510565162951535312, 1.000000000000000000, 0.9510565162951535312, 1.000000000000000000, 0.9510565162951535312, 1.000000000000000000, 0.9510565162951535312, 1.000000000000000000, 0.9510565162951535312, 1.000000000000000000, 0.9510565162951535312, 1.000000000000000000, 0.9510565162951535312, 1.000000000000000000, 0.9510565162951535312, 1.000000000000000000, 0.9510565162951535312, 1.000000000000000000, 0.9510565162951535312, 1.000000000000000000, 0.9510565162951535312, 1.000000000000000000, 0.9510565162951535312, 1.000000000000000000, 0.9510565162951535312, 1.000000000000000000, 0.9510565162951535312, 1.000000000000000000, 0.9510565162951535312, 1.000000000000000000, 0.9510565162951535312, 1.000000000000000000, 0.9510565162951535312, 1.000000000000000000, 0.9510565162951535312, 1.000000000000000000, 0.9510565162951535312, 1.000000000000000000, 0.9510565162951535312, 1.000000000000000000, 0.9510565162951535312, 1.000000000000000000, 0.9510565162951535312, 1.000000000000000000, 0.9510565162951535312, 1.000000000000000000, 0.9510565162951535312, 1.000000000000000000, 0.9510565162951535312, 1.000000000000000000, 0.9510565162951535312, 1.000000000000000000, 0.9510565162951535312, 1.000000000000000000, 0.9510565162951535312, 1.000000000000000000) ) ) 
 REPRESENTATION_ITEM ( '' )  SURFACE ( )  );
#27790 = CARTESIAN_POINT ( 'NONE',  ( 105.6631189606246295, 105.8855032339526758, -48.20000000000001705 ) ) ;
#27791 = CARTESIAN_POINT ( 'NONE',  ( 5.444914386472302859, 38.42031250108393436, 13.14518615778179189 ) ) ;
#27792 = ADVANCED_FACE ( 'NONE', ( #26924 ), #22211, .F. ) ;
#27793 = CARTESIAN_POINT ( 'NONE',  ( 181.4251840539369596, 38.56914062500000284, -5.622872871577873077 ) ) ;
#27794 = CONTEXT_DEPENDENT_SHAPE_REPRESENTATION ( #6050, #9448 ) ;
#27795 = CYLINDRICAL_SURFACE ( 'NONE', #15963, 5.000000000000004441 ) ;
#27796 = CARTESIAN_POINT ( 'NONE',  ( 103.1528011352953342, -3.152801135295355106, 5.062500001365592972 ) ) ;
#27797 = CARTESIAN_POINT ( 'NONE',  ( 65.00000000000000000, 37.97382812608393721, -13.14518615778179544 ) ) ;
#27798 = EDGE_CURVE ( 'NONE', #21990, #22337, #25701, .T. ) ;
#27799 = CARTESIAN_POINT ( 'NONE',  ( 98.15313185440923860, 4.458734125000016313, 5.250000001365592972 ) ) ;
#27800 = CARTESIAN_POINT ( 'NONE',  ( 104.9999999999999716, 1.449011120738813565E-14, 10.62500000273118594 ) ) ;
#27801 = CARTESIAN_POINT ( 'NONE',  ( 101.8468681455907330, 92.74999999863439371, -4.458734124999994997 ) ) ;
#27802 = FACE_OUTER_BOUND ( 'NONE', #21221, .T. ) ;
#27803 = CARTESIAN_POINT ( 'NONE',  ( 2.493653234604083739E-15, 40.40468749999999432, 13.57481594606304576 ) ) ;
#27804 = CARTESIAN_POINT ( 'NONE',  ( 97.83688103937537051, 103.3426043859339103, -45.60000000000000853 ) ) ;
#27805 = EDGE_CURVE ( 'NONE', #24651, #487, #11351, .T. ) ;
#27806 = VERTEX_POINT ( 'NONE', #18064 ) ;
#27807 = CARTESIAN_POINT ( 'NONE',  ( 101.8468681455906903, 82.37500000136562051, -4.458734125000016313 ) ) ;
#27808 = CARTESIAN_POINT ( 'NONE',  ( 96.84719886470463734, 90.93749999863440792, 3.152801135295351997 ) ) ;
#27809 = VERTEX_POINT ( 'NONE', #26780 ) ;
#27810 = EDGE_CURVE ( 'NONE', #2928, #2045, #18962, .T. ) ;
#27811 = CARTESIAN_POINT ( 'NONE',  ( 1.662435489736055892E-15, 40.99999999999999289, 13.57481594606304576 ) ) ;
#27812 = CARTESIAN_POINT ( 'NONE',  ( 70.44491438647230552, 34.15390625108393863, -13.14518615778179900 ) ) ;
#27813 = ORIENTED_EDGE ( 'NONE', *, *, #10987, .F. ) ;
#27814 = CARTESIAN_POINT ( 'NONE',  ( 123.9209199794811980, 54.65154858643462177, -15.00000000000000178 ) ) ;
#27815 = AXIS2_PLACEMENT_3D ( 'NONE', #20208, #15344, #2409 ) ;
#27816 = CARTESIAN_POINT ( 'NONE',  ( 104.4587341249999639, 1.442382525525748735E-14, 5.187500001365592972 ) ) ;
#27817 = ORIENTED_EDGE ( 'NONE', *, *, #6927, .F. ) ;
#27818 = CARTESIAN_POINT ( 'NONE',  ( 2.414731522848535132E-15, 34.60039062608393579, 13.14518615778179544 ) ) ;
#27819 = CARTESIAN_POINT ( 'NONE',  ( 9.295050272127046043, 33.11210937608393579, -9.295050272127046043 ) ) ;
#27820 = CARTESIAN_POINT ( 'NONE',  ( 195.0000000000000000, 38.12265625216787157, 13.57481594606304576 ) ) ;
#27821 = CARTESIAN_POINT ( 'NONE',  ( -13.14518615778179722, 39.71015625108393010, -5.444914386472297529 ) ) ;
#27822 = DIRECTION ( 'NONE',  ( -0.000000000000000000, 1.000000000000000000, -0.000000000000000000 ) ) ;
#27823 = CARTESIAN_POINT ( 'NONE',  ( 198.9798144458085858, 50.00000000123236532, 13.01613927312799390 ) ) ;
#27824 = CARTESIAN_POINT ( 'NONE',  ( 124.5550856135277087, 39.80937500108393579, -13.14518615778179722 ) ) ;
#27825 = CARTESIAN_POINT ( 'NONE',  ( 2.414731522848535132E-15, 39.36289062608393152, 13.14518615778179544 ) ) ;
#27826 = CONICAL_SURFACE ( 'NONE', #6870, 12.50000000000001599, 0.7853981633974491672 ) ;
#27827 = ORIENTED_EDGE ( 'NONE', *, *, #19570, .F. ) ;
#27828 = CARTESIAN_POINT ( 'NONE',  ( 70.62287287157786864, 37.57695312499998863, -13.57481594606304753 ) ) ;
#27829 = CARTESIAN_POINT ( 'NONE',  ( 9.598844408820459861, 38.22187500216787015, 9.598844408820456309 ) ) ;
#27830 = CARTESIAN_POINT ( 'NONE',  ( 201.3519322287720854, 36.00000000000000711, 11.61660627739470186 ) ) ;
#27831 = CARTESIAN_POINT ( 'NONE',  ( 103.1528011352953342, -3.152801135295355106, 4.812500001365592084 ) ) ;
#27832 = CARTESIAN_POINT ( 'NONE',  ( -13.14518615778179900, 31.97109375108393436, -5.444914386472297529 ) ) ;
#27833 = CARTESIAN_POINT ( 'NONE',  ( 98.15313185440923860, 4.458734125000016313, 1.500000001365592972 ) ) ;
#27834 = CARTESIAN_POINT ( 'NONE',  ( 95.54126587499996504, 83.62500000136560629, -1.846868145590750077 ) ) ;
#27835 = CARTESIAN_POINT ( 'NONE',  ( 13.14518615778179900, 32.26875000108393721, -5.444914386472297529 ) ) ;
#27836 = CARTESIAN_POINT ( 'NONE',  ( -13.14518615778179189, 39.21406250108392300, 5.444914386472304635 ) ) ;
#27837 = ADVANCED_FACE ( 'NONE', ( #23200 ), #5675, .T. ) ;
#27838 = CARTESIAN_POINT ( 'NONE',  ( 106.5389055433250860, 114.7507929638356785, -46.67499999726882720 ) ) ;
#27839 = EDGE_LOOP ( 'NONE', ( #23525, #17527, #5482, #5375 ) ) ;
#27840 = CARTESIAN_POINT ( 'NONE',  ( -13.57481594606304576, 40.65273437608393436, 0.000000000000000000 ) ) ;
#27841 = LINE ( 'NONE', #23698, #21667 ) ;
#27842 = CARTESIAN_POINT ( 'NONE',  ( 96.46446609406721961, 81.25000000273119838, 3.535533905932727539 ) ) ;
#27843 = CARTESIAN_POINT ( 'NONE',  ( 102.4976396683250783, 117.6869444889999841, -54.47499999726881725 ) ) ;
#27844 = CARTESIAN_POINT ( 'NONE',  ( 97.92893218813451028, -4.999999999999989342, 6.312500002731185056 ) ) ;
#27845 = ORIENTED_EDGE ( 'NONE', *, *, #15166, .T. ) ;
#27846 = CARTESIAN_POINT ( 'NONE',  ( 78.14518615778179367, 37.97382812608393721, -1.609821015232357215E-15 ) ) ;
#27847 = DIRECTION ( 'NONE',  ( -0.000000000000000000, 1.000000000000000000, -0.000000000000000000 ) ) ;
#27848 = CARTESIAN_POINT ( 'NONE',  ( 13.57481594606304931, 34.99726562500000426, 5.622872871577868636 ) ) ;
#27849 = EDGE_LOOP ( 'NONE', ( #20054, #9213, #17004 ) ) ;
#27850 = CARTESIAN_POINT ( 'NONE',  ( 94.33688103937537051, 105.8855032339526758, -49.80000000000000426 ) ) ;
#27851 = FACE_OUTER_BOUND ( 'NONE', #17213, .T. ) ;
#27852 = CARTESIAN_POINT ( 'NONE',  ( 102.0669872999999797, 123.5500000010924708, -9.794112055954760458E-15 ) ) ;
#27853 = CARTESIAN_POINT ( 'NONE',  ( 135.6228728715778971, 34.99726562716787726, 13.57481594606304576 ) ) ;
#27854 = CARTESIAN_POINT ( 'NONE',  ( 70.44491438647230552, 40.20625000108394431, 13.14518615778179189 ) ) ;
#27855 = CARTESIAN_POINT ( 'NONE',  ( 208.1451861577817795, 35.54296875108394715, 5.444914386472293977 ) ) ;
#27856 = ORIENTED_EDGE ( 'NONE', *, *, #17865, .F. ) ;
#27857 = VERTEX_POINT ( 'NONE', #27481 ) ;
#27858 = ORIENTED_EDGE ( 'NONE', *, *, #3745, .F. ) ;
#27859 = CARTESIAN_POINT ( 'NONE',  ( -13.14518615778179544, 33.40976562608393863, 0.000000000000000000 ) ) ;
#27860 =( LENGTH_UNIT ( ) NAMED_UNIT ( * ) SI_UNIT ( .MILLI., .METRE. ) );
#27861 = DIRECTION ( 'NONE',  ( 0.000000000000000000, 3.469446951953611231E-16, -1.000000000000000000 ) ) ;
#27862 = CARTESIAN_POINT ( 'NONE',  ( 99.99999999999998579, 92.12499999726880162, -4.999999999999997335 ) ) ;
#27863 = CARTESIAN_POINT ( 'NONE',  ( 104.4587341249999781, 83.87500000136560629, 1.846868145590721655 ) ) ;
#27864 = CARTESIAN_POINT ( 'NONE',  ( -3.061616997868384226E-15, 23.00000000000000000, -25.00000000000001066 ) ) ;
#27865 = CARTESIAN_POINT ( 'NONE',  ( 143.5748159460630688, 39.95820312716787726, -5.622872871577873966 ) ) ;
#27866 = FACE_OUTER_BOUND ( 'NONE', #25414, .T. ) ;
#27867 = DIRECTION ( 'NONE',  ( -0.000000000000000000, 1.000000000000000000, 0.000000000000000000 ) ) ;
#27868 = CARTESIAN_POINT ( 'NONE',  ( 102.0710678118654897, 93.68749999726880162, 4.999999999999953815 ) ) ;
#27869 = EDGE_LOOP ( 'NONE', ( #19798, #19309, #11622, #26080 ) ) ;
#27870 = CARTESIAN_POINT ( 'NONE',  ( -13.14518615778179544, 32.02070312608393010, 0.000000000000000000 ) ) ;
#27871 = CARTESIAN_POINT ( 'NONE',  ( 3.878385410779738418, 31.34156310770110565, -13.57481594606304931 ) ) ;
#27872 =( BOUNDED_CURVE ( )  B_SPLINE_CURVE ( 2, ( #25432, #27171, #14301, #12154, #27434, #7624, #7899, #16593, #25287, #5915, #5772, #14443, #4186, #6456, #12715, #23711, #16869 ),
 .UNSPECIFIED., .F., .F. ) 
 B_SPLINE_CURVE_WITH_KNOTS ( ( 3, 2, 2, 2, 2, 2, 2, 2, 3 ),
 ( 0.8500000005328695041, 0.8599999999999999867, 0.8800000000000000044, 0.9000000000000000222, 0.9200000000000000400, 0.9399999999999999467, 0.9599999999999999645, 0.9799999999999999822, 1.000000000000000000 ),
 .UNSPECIFIED. ) 
 CURVE ( )  GEOMETRIC_REPRESENTATION_ITEM ( )  RATIONAL_B_SPLINE_CURVE ( ( 0.9755282581475768211, 0.9755282594516012651, 1.000000000000000000, 0.9510565162951535312, 1.000000000000000000, 0.9510565162951535312, 1.000000000000000000, 0.9510565162951535312, 1.000000000000000000, 0.9510565162951535312, 1.000000000000000000, 0.9510565162951535312, 1.000000000000000000, 0.9510565162951535312, 1.000000000000000000, 0.9510565162951535312, 1.000000000000000000 ) ) 
 REPRESENTATION_ITEM ( '' )  );
#27873 = CARTESIAN_POINT ( 'NONE',  ( 94.99999999999995737, 1.387778780781445676E-14, 1.125000002731184390 ) ) ;
#27874 = CARTESIAN_POINT ( 'NONE',  ( 120.7049497278729575, 36.88242187608393152, 9.295050272127047819 ) ) ;
#27875 = CARTESIAN_POINT ( 'NONE',  ( 51.85481384221820633, 37.37851562608393863, 0.000000000000000000 ) ) ;
#27876 = CARTESIAN_POINT ( 'NONE',  ( 185.7049497278729575, 31.92148437608393508, 9.295050272127047819 ) ) ;
#27877 = ORIENTED_EDGE ( 'NONE', *, *, #5353, .T. ) ;
#27878 = CARTESIAN_POINT ( 'NONE',  ( 52.94344797029973648, 36.00000000000000000, 5.307619621752120764 ) ) ;
#27879 = CARTESIAN_POINT ( 'NONE',  ( 5.444914386472297529, 35.54296875108393294, -13.14518615778179900 ) ) ;
#27880 = CARTESIAN_POINT ( 'NONE',  ( 125.4951129136839825, 51.44650206076906329, -15.00000000000066258 ) ) ;
#27881 = CARTESIAN_POINT ( 'NONE',  ( 0.000000000000000000, 11.00000000000000355, 17.49444650053485972 ) ) ;
#27882 = CARTESIAN_POINT ( 'NONE',  ( 96.46446609406721961, 81.87500000000000000, -3.535533905932755072 ) ) ;
#27883 = CARTESIAN_POINT ( 'NONE',  ( 5.444914386472297529, 38.71796875108393721, -13.14518615778179900 ) ) ;
#27884 = LINE ( 'NONE', #17031, #11536 ) ;
#27885 = CARTESIAN_POINT ( 'NONE',  ( 102.4999999999999716, 124.6500000000000199, -1.035533905932742638 ) ) ;
#27886 = CARTESIAN_POINT ( 'NONE',  ( 97.93301269999999192, 123.2000000010924765, 0.8561741729129329626 ) ) ;
#27887 = CARTESIAN_POINT ( 'NONE',  ( 101.4615807364564546, 123.4500000010924765, 1.461580736456455476 ) ) ;
#27888 =( NAMED_UNIT ( * ) SI_UNIT ( $, .STERADIAN. ) SOLID_ANGLE_UNIT ( ) );
#27889 = ORIENTED_EDGE ( 'NONE', *, *, #12602, .F. ) ;
#27890 = CARTESIAN_POINT ( 'NONE',  ( 103.1528011352953342, 3.152801135295383084, 13.06250000136559208 ) ) ;
#27891 = CARTESIAN_POINT ( 'NONE',  ( 93.00000000000000000, 110.0000000000000000, -48.50000000546238255 ) ) ;
#27892 = ORIENTED_EDGE ( 'NONE', *, *, #1010, .T. ) ;
#27893 = CARTESIAN_POINT ( 'NONE',  ( 101.7677669529663547, 124.0000000021849615, -1.767766952966370209 ) ) ;
#27894 = CARTESIAN_POINT ( 'NONE',  ( 104.4587341249999639, 1.442382525525748735E-14, 10.93750000136559208 ) ) ;
#27895 = CARTESIAN_POINT ( 'NONE',  ( -13.14518615778179544, 32.61601562608393579, 0.000000000000000000 ) ) ;
#27896 = AXIS2_PLACEMENT_3D ( 'NONE', #16166, #22883, #14581 ) ;
#27897 = CARTESIAN_POINT ( 'NONE',  ( 2.493653234604083739E-15, 31.77265625216787370, 13.57481594606304576 ) ) ;
#27898 = CARTESIAN_POINT ( 'NONE',  ( 94.99999999999995737, 2.071067811865491493, 3.062500002731185944 ) ) ;
#27899 = CARTESIAN_POINT ( 'NONE',  ( 98.15313185440925281, 80.25000000136559208, -4.458734125000016313 ) ) ;
#27900 = CARTESIAN_POINT ( 'NONE',  ( 65.00000000000000000, 38.56914062608393579, 13.14518615778179544 ) ) ;
#27901 = CARTESIAN_POINT ( 'NONE',  ( 108.0825317500000011, 112.6261737610028320, -50.27500000273119696 ) ) ;
#27902 = CARTESIAN_POINT ( 'NONE',  ( 96.46446609406721961, 3.535533905932755072, 11.87500000000000000 ) ) ;
#27903 = CARTESIAN_POINT ( 'NONE',  ( 102.0669872999999939, 122.8000000010924708, -0.8561741729129507261 ) ) ;
#27904 = DIRECTION ( 'NONE',  ( -0.000000000000000000, 1.000000000000000000, -0.000000000000000000 ) ) ;
#27905 = CARTESIAN_POINT ( 'NONE',  ( 102.1631189606246153, 116.6573956140660897, -51.09999999453764019 ) ) ;
#27906 = CARTESIAN_POINT ( 'NONE',  ( 124.3771271284221314, 40.85117187499999147, -13.57481594606304753 ) ) ;
#27907 = ORIENTED_EDGE ( 'NONE', *, *, #8942, .F. ) ;
#27908 = CYLINDRICAL_SURFACE ( 'NONE', #22237, 13.57481594606304398 ) ;
#27909 = FACE_OUTER_BOUND ( 'NONE', #16370, .T. ) ;
#27910 = CARTESIAN_POINT ( 'NONE',  ( 104.4587341249999781, 81.00000000136560629, -1.846868145590750299 ) ) ;
#27911 = CARTESIAN_POINT ( 'NONE',  ( 143.1451861577818079, 39.41250000108393436, -5.444914386472297529 ) ) ;
#27912 = CARTESIAN_POINT ( 'NONE',  ( 59.37712712842213136, 38.07304687716787583, 13.57481594606304753 ) ) ;
#27913 = EDGE_CURVE ( 'NONE', #22062, #15169, #24981, .T. ) ;
#27914 = CARTESIAN_POINT ( 'NONE',  ( 108.0825317499999869, 112.6261737610028320, -54.52499999726880731 ) ) ;
#27915 = CARTESIAN_POINT ( 'NONE',  ( 5.622872871577871301, 34.50117187716788436, -13.57481594606304753 ) ) ;
#27916 = ORIENTED_EDGE ( 'NONE', *, *, #26236, .T. ) ;
#27917 = VECTOR ( 'NONE', #11611, 1000.000000000000000 ) ;
#27918 = CARTESIAN_POINT ( 'NONE',  ( 102.0710678118654329, -4.999999999999989342, 4.312500000000000000 ) ) ;
#27919 =( BOUNDED_CURVE ( )  B_SPLINE_CURVE ( 2, ( #13379, #22108, #2587, #22532, #15817, #22388, #9552, #20816, #3288 ),
 .UNSPECIFIED., .F., .T. ) 
 B_SPLINE_CURVE_WITH_KNOTS ( ( 3, 2, 2, 2, 3 ),
 ( 0.1875000000000001388, 0.1979166666666667407, 0.2083333333333333703, 0.2187499999999999722, 0.2291666666666665741 ),
 .UNSPECIFIED. ) 
 CURVE ( )  GEOMETRIC_REPRESENTATION_ITEM ( )  RATIONAL_B_SPLINE_CURVE ( ( 0.9999999999999990008, 0.9238795325112877377, 1.000000000000000000, 0.9238795325112867385, 1.000000000000000000, 0.9238795325112867385, 1.000000000000000000, 0.9238795325112872936, 0.9999999999999994449 ) ) 
 REPRESENTATION_ITEM ( '' )  );
#27920 = CARTESIAN_POINT ( 'NONE',  ( 200.4449143864723055, 37.92421875108392726, -13.14518615778179900 ) ) ;
#27921 = CARTESIAN_POINT ( 'NONE',  ( 2.493653234604083739E-15, 38.81718749999999574, 13.57481594606304576 ) ) ;
#27922 = CARTESIAN_POINT ( 'NONE',  ( 130.0000000000000000, 38.37070312608393152, 13.14518615778179544 ) ) ;
#27923 = CARTESIAN_POINT ( 'NONE',  ( 13.57481594606304931, 35.79101562499999289, 5.622872871577868636 ) ) ;
#27924 = CARTESIAN_POINT ( 'NONE',  ( 219.9999999999999716, 75.00000000000000000, 14.99999999999994316 ) ) ;
#27925 = CARTESIAN_POINT ( 'NONE',  ( -8.312177448680279460E-16, 38.42031249999999432, -13.57481594606304576 ) ) ;
#27926 = FACE_OUTER_BOUND ( 'NONE', #1461, .T. ) ;
#27927 = CARTESIAN_POINT ( 'NONE',  ( 101.7677669529663547, 123.0999999999999943, -1.767766952966370209 ) ) ;
#27928 = CARTESIAN_POINT ( 'NONE',  ( 185.4011555911795597, 37.13046874999999147, 9.598844408820459861 ) ) ;
#27929 = PRODUCT_CONTEXT ( 'NONE', #21529, 'mechanical' ) ;
#27930 = CARTESIAN_POINT ( 'NONE',  ( 84.99999999999998579, 118.0000000000000000, -15.00000000000000533 ) ) ;
#27931 = CARTESIAN_POINT ( 'NONE',  ( 104.4587341249999639, 1.442382525525748735E-14, 4.187500001365592084 ) ) ;
#27932 = CARTESIAN_POINT ( 'NONE',  ( 51.85481384221819923, 38.91640625108393436, -5.444914386472297529 ) ) ;
#27933 = CARTESIAN_POINT ( 'NONE',  ( 99.99999999999995737, 4.458734125000016313, 7.187500001365592084 ) ) ;
#27934 = CARTESIAN_POINT ( 'NONE',  ( 100.0000000000000000, 110.0000000000000000, -55.00000000000000711 ) ) ;
#27935 = CARTESIAN_POINT ( 'NONE',  ( 95.54126587500000767, 92.81249999863440792, -7.484931351350258973E-15 ) ) ;
#27936 = CARTESIAN_POINT ( 'NONE',  ( 120.4011555911795455, 39.51171874999999289, 9.598844408820459861 ) ) ;
#27937 = CARTESIAN_POINT ( 'NONE',  ( -13.57481594606304753, 39.36289062499999858, -5.622872871577873077 ) ) ;
#27938 = CARTESIAN_POINT ( 'NONE',  ( 120.7049497278729575, 40.05742187608393579, 9.295050272127047819 ) ) ;
#27939 = ORIENTED_EDGE ( 'NONE', *, *, #16296, .T. ) ;
#27940 = CARTESIAN_POINT ( 'NONE',  ( 99.99999999999995737, 82.43750000136559208, -4.458734125000016313 ) ) ;
#27941 = EDGE_CURVE ( 'NONE', #15622, #16261, #25053, .T. ) ;
#27942 = LINE ( 'NONE', #16687, #22047 ) ;
#27943 = ORIENTED_EDGE ( 'NONE', *, *, #16579, .F. ) ;
#27944 = CARTESIAN_POINT ( 'NONE',  ( 99.99999999999998579, 128.0000000000000000, -5.204170427930421283E-15 ) ) ;
#27945 = CARTESIAN_POINT ( 'NONE',  ( 74.29505027212704249, 33.90585937608393863, 9.295050272127046043 ) ) ;
#27946 = ORIENTED_EDGE ( 'NONE', *, *, #27613, .F. ) ;
#27947 = ADVANCED_FACE ( 'NONE', ( #7803 ), #23332, .F. ) ;
#27948 = CARTESIAN_POINT ( 'NONE',  ( -13.57481594606304753, 36.98164062499999005, -5.622872871577872189 ) ) ;
#27949 = CARTESIAN_POINT ( 'NONE',  ( 96.84719886470459471, 3.152801135295383084, 3.562500001365592972 ) ) ;
#27950 = EDGE_CURVE ( 'NONE', #22274, #24795, #16633, .T. ) ;
#27951 = ORIENTED_EDGE ( 'NONE', *, *, #6682, .F. ) ;
#27952 = CARTESIAN_POINT ( 'NONE',  ( 94.99999999999995737, 82.06250000273119838, -2.071067811865491493 ) ) ;
#27953 = CARTESIAN_POINT ( 'NONE',  ( 9.295050272127046043, 39.66054687608393436, -9.295050272127046043 ) ) ;
#27954 = CARTESIAN_POINT ( 'NONE',  ( 195.0000000000000000, 38.91640625216786731, 13.57481594606304576 ) ) ;
#27955 = CARTESIAN_POINT ( 'NONE',  ( -8.049105076161786076E-16, 37.18007812608393436, -13.14518615778179544 ) ) ;
#27956 = CYLINDRICAL_SURFACE ( 'NONE', #21292, 5.000000000000004441 ) ;
#27957 = CARTESIAN_POINT ( 'NONE',  ( 199.8584992904752937, 49.99999999891486624, 12.70434618648238256 ) ) ;
#27958 = CARTESIAN_POINT ( 'NONE',  ( -12.68159279706118170, 36.04503594658365984, 5.908507747192915716 ) ) ;
#27959 = CARTESIAN_POINT ( 'NONE',  ( 13.14518615778179900, 38.81718750108393579, -5.444914386472297529 ) ) ;
#27960 = ORIENTED_EDGE ( 'NONE', *, *, #19455, .F. ) ;
#27961 = CARTESIAN_POINT ( 'NONE',  ( 116.8548138422182063, 35.74140625108393721, -5.444914386472297529 ) ) ;
#27962 = CARTESIAN_POINT ( 'NONE',  ( 51.42518405393695957, 37.82499999999999574, 0.000000000000000000 ) ) ;
#27963 = CARTESIAN_POINT ( 'NONE',  ( 65.00000000000000000, 39.31328125216787583, -13.57481594606304576 ) ) ;
#27964 = EDGE_CURVE ( 'NONE', #637, #8989, #25326, .T. ) ;
#27965 = CARTESIAN_POINT ( 'NONE',  ( 104.4587341249999781, -1.846868145590721655, 1.875000001365591862 ) ) ;
#27966 = CARTESIAN_POINT ( 'NONE',  ( 96.46446609406721961, 84.00000000273119838, -3.535533905932755072 ) ) ;
#27967 = CARTESIAN_POINT ( 'NONE',  ( 95.54126587499996504, 1.387778780781445676E-14, 2.437500001365592084 ) ) ;
#27968 = CARTESIAN_POINT ( 'NONE',  ( 97.50236033167492167, 117.6869444889999841, -49.52500000273119696 ) ) ;
#27969 = CARTESIAN_POINT ( 'NONE',  ( 98.15313185440923860, -4.458734124999987891, 4.875000001365592084 ) ) ;
#27970 = CARTESIAN_POINT ( 'NONE',  ( 0.000000000000000000, 10.00000000000000000, 0.000000000000000000 ) ) ;
#27971 = CARTESIAN_POINT ( 'NONE',  ( -5.444914386472299306, 31.97109375108393436, 13.14518615778179722 ) ) ;
#27972 = CARTESIAN_POINT ( 'NONE',  ( 13.14518615778179544, 39.56132812608393579, -1.609821015232357215E-15 ) ) ;
#27973 = CARTESIAN_POINT ( 'NONE',  ( 97.50236033167490746, 102.3130555110000159, -49.47499999726882436 ) ) ;
#27974 = ORIENTED_EDGE ( 'NONE', *, *, #9118, .F. ) ;
#27975 = DIRECTION ( 'NONE',  ( -0.000000000000000000, -1.000000000000000000, -0.000000000000000000 ) ) ;
#27976 = CARTESIAN_POINT ( 'NONE',  ( 92.99999999999998579, 107.7255621263696526, -54.39999999453763024 ) ) ;
#27977 = DIRECTION ( 'NONE',  ( 5.782411586589357392E-17, -0.000000000000000000, 1.000000000000000000 ) ) ;
#27978 = CARTESIAN_POINT ( 'NONE',  ( 108.0825317500000011, 110.0000000000000000, -52.87499999726882294 ) ) ;
#27979 = CARTESIAN_POINT ( 'NONE',  ( -5.622872871577873966, 36.98164062716787015, -13.57481594606304753 ) ) ;
#27980 = EDGE_CURVE ( 'NONE', #6018, #10602, #12338, .T. ) ;
#27981 = CARTESIAN_POINT ( 'NONE',  ( 181.8548138422182205, 38.96601562608393721, 0.000000000000000000 ) ) ;
#27982 = VERTEX_POINT ( 'NONE', #19042 ) ;
#27983 = CARTESIAN_POINT ( 'NONE',  ( 130.0000000000000000, 36.13828125216787157, -13.57481594606304576 ) ) ;
#27984 = CARTESIAN_POINT ( 'NONE',  ( 104.3262379212492448, 104.0454443415356991, -54.30000000000001137 ) ) ;
#27985 = CARTESIAN_POINT ( 'NONE',  ( 95.27063293749995410, 1.387778780781445676E-14, 0.2812500020483886254 ) ) ;
#27986 = ORIENTED_EDGE ( 'NONE', *, *, #2022, .F. ) ;
#27987 = CARTESIAN_POINT ( 'NONE',  ( 93.00000000000000000, 110.0000000000000000, -50.00000000000000711 ) ) ;
#27988 = VECTOR ( 'NONE', #20908, 1000.000000000000000 ) ;
#27989 = CYLINDRICAL_SURFACE ( 'NONE', #617, 15.57481594606304576 ) ;
#27990 = CARTESIAN_POINT ( 'NONE',  ( 99.99999999999998579, 123.7500000010924737, -2.066987299999998751 ) ) ;
#27991 = EDGE_CURVE ( 'NONE', #22131, #18157, #21893, .T. ) ;
#27992 = CARTESIAN_POINT ( 'NONE',  ( 139.5988444088204687, 35.04687500216787299, 9.598844408820456309 ) ) ;
#27993 = CARTESIAN_POINT ( 'NONE',  ( 74.29505027212704249, 40.45429687608393721, -9.295050272127046043 ) ) ;
#27994 = CARTESIAN_POINT ( 'NONE',  ( 99.99999999999995737, 84.25000000000000000, 4.999999999999990230 ) ) ;
#27995 = CARTESIAN_POINT ( 'NONE',  ( 204.2950502721270425, 34.10429687608393579, -9.295050272127046043 ) ) ;
#27996 = ORIENTED_EDGE ( 'NONE', *, *, #16960, .F. ) ;
#27997 = ORIENTED_EDGE ( 'NONE', *, *, #25674, .T. ) ;
#27998 = CARTESIAN_POINT ( 'NONE',  ( -5.444914386472297529, 38.22187500108393010, -13.14518615778179900 ) ) ;
#27999 = CARTESIAN_POINT ( 'NONE',  ( 94.99999999999995737, 84.00000000000000000, -1.387778780781445676E-14 ) ) ;
#28000 = CARTESIAN_POINT ( 'NONE',  ( 13.57481594606304931, 38.17226562499999432, 5.622872871577868636 ) ) ;
#28001 = CARTESIAN_POINT ( 'NONE',  ( 101.8468681455907046, 82.75000000136560629, 4.458734124999987891 ) ) ;
#28002 = CARTESIAN_POINT ( 'NONE',  ( 70.62287287157796811, 40.05742187716787583, -13.57481594606294095 ) ) ;
#28003 = CARTESIAN_POINT ( 'NONE',  ( -13.14518615778179189, 40.00781250108393294, 5.444914386472304635 ) ) ;
#28004 = LINE ( 'NONE', #21031, #12614 ) ;
#28005 = AXIS2_PLACEMENT_3D ( 'NONE', #9237, #8810, #2829 ) ;
#28006 = CARTESIAN_POINT ( 'NONE',  ( 107.0000000000000142, 110.0000000000000000, -51.50000000546237544 ) ) ;
#28007 = CARTESIAN_POINT ( 'NONE',  ( 107.0000000000000142, 110.0000000000000000, -49.00000000000000711 ) ) ;
#28008 = CARTESIAN_POINT ( 'NONE',  ( 108.0825317500000011, 110.0000000000000000, -46.62499999726882294 ) ) ;
#28009 = VERTEX_POINT ( 'NONE', #10062 ) ;
#28010 = CARTESIAN_POINT ( 'NONE',  ( 13.57481594606304931, 36.58476562499999574, 5.622872871577869525 ) ) ;
#28011 = CARTESIAN_POINT ( 'NONE',  ( -9.295050272127046043, 36.48554687608393721, -9.295050272127046043 ) ) ;
#28012 = VECTOR ( 'NONE', #11390, 1000.000000000000000 ) ;
#28013 = CARTESIAN_POINT ( 'NONE',  ( 104.9999999999999574, -2.071067811865462627, 3.562500002731184612 ) ) ;
#28014 = CARTESIAN_POINT ( 'NONE',  ( 116.8548138422182063, 36.73359375108393010, -5.444914386472297529 ) ) ;
#28015 = CARTESIAN_POINT ( 'NONE',  ( 78.14518615778179367, 36.13828125108393863, 5.444914386472293977 ) ) ;
#28016 = CARTESIAN_POINT ( 'NONE',  ( 181.8548138422182205, 39.95820312608393010, 0.000000000000000000 ) ) ;
#28017 = LINE ( 'NONE', #24160, #21167 ) ;
#28018 = CARTESIAN_POINT ( 'NONE',  ( 13.14518615778179900, 36.23750000108393010, -5.444914386472297529 ) ) ;
#28019 = CARTESIAN_POINT ( 'NONE',  ( 139.1801758136479918, 55.00000000000000000, -15.00000000000000000 ) ) ;
#28020 = FACE_OUTER_BOUND ( 'NONE', #1322, .T. ) ;
#28021 = DIRECTION ( 'NONE',  ( 0.000000000000000000, -0.7071067811865482389, -0.7071067811865469066 ) ) ;
#28022 = AXIS2_PLACEMENT_3D ( 'NONE', #1784, #27723, #25853 ) ;
#28023 = CARTESIAN_POINT ( 'NONE',  ( 13.14518615778179900, 39.41250000108393436, -5.444914386472297529 ) ) ;
#28024 = CARTESIAN_POINT ( 'NONE',  ( -8.312177448680279460E-16, 37.72578125216787726, -13.57481594606304576 ) ) ;
#28025 = CARTESIAN_POINT ( 'NONE',  ( 101.0355339059327378, 123.2500000021849758, -2.499999999999997780 ) ) ;
#28026 = CARTESIAN_POINT ( 'NONE',  ( 63.05267407791385637, 51.47162402671693116, 15.00000000000195399 ) ) ;
#28027 = VERTEX_POINT ( 'NONE', #18774 ) ;
#28028 = CARTESIAN_POINT ( 'NONE',  ( -5.622872871577804688, 37.18007812499999432, 13.57481594606311504 ) ) ;
#28029 = CARTESIAN_POINT ( 'NONE',  ( 101.8468681455906903, 4.458734125000016313, 9.125000001365592084 ) ) ;
#28030 = CARTESIAN_POINT ( 'NONE',  ( 78.45411265623080510, 36.00000000000001421, 0.6772748633563907550 ) ) ;
#28031 = VERTEX_POINT ( 'NONE', #5812 ) ;
#28032 = CARTESIAN_POINT ( 'NONE',  ( 9.180175813647995398, 55.00000000000000000, 9.999999999999994671 ) ) ;
#28033 = CARTESIAN_POINT ( 'NONE',  ( 104.4587341249999639, 1.442382525525748735E-14, 11.93750000136559208 ) ) ;
#28034 = CARTESIAN_POINT ( 'NONE',  ( 2.414731522848535132E-15, 38.37070312608393152, 13.14518615778179544 ) ) ;
#28035 = DIRECTION ( 'NONE',  ( -0.000000000000000000, -1.000000000000000000, -0.000000000000000000 ) ) ;
#28036 = CARTESIAN_POINT ( 'NONE',  ( 96.84719886470459471, 80.56250000136559208, -3.152801135295383084 ) ) ;
#28037 = CARTESIAN_POINT ( 'NONE',  ( 55.70494972787295751, 37.47773437608393010, -9.295050272127046043 ) ) ;
#28038 = CARTESIAN_POINT ( 'NONE',  ( 106.5389055433251002, 105.2492070361643215, -44.57500000273119412 ) ) ;
#28039 = CARTESIAN_POINT ( 'NONE',  ( -13.14518615778179189, 39.80937500108393579, 5.444914386472304635 ) ) ;
#28040 =( BOUNDED_CURVE ( )  B_SPLINE_CURVE ( 2, ( #3841, #10374, #25225, #14649, #20683, #23096, #23368, #27787, #8111 ),
 .UNSPECIFIED., .F., .F. ) 
 B_SPLINE_CURVE_WITH_KNOTS ( ( 3, 2, 2, 2, 3 ),
 ( 0.3541666666666666852, 0.3645833333333332593, 0.3749999999999998890, 0.3854166666666665741, 0.3958333333333331483 ),
 .UNSPECIFIED. ) 
 CURVE ( )  GEOMETRIC_REPRESENTATION_ITEM ( )  RATIONAL_B_SPLINE_CURVE ( ( 1.000000000000000000, 0.9238795325112867385, 1.000000000000000000, 0.9238795325112867385, 1.000000000000000000, 0.9238795325112867385, 1.000000000000000000, 0.9238795325112879597, 0.9999999999999987788 ) ) 
 REPRESENTATION_ITEM ( '' )  );
#28041 = VERTEX_POINT ( 'NONE', #18905 ) ;
#28042 = CARTESIAN_POINT ( 'NONE',  ( 104.9999999999999716, 1.449011120738813565E-14, 8.499999999999998224 ) ) ;
#28043 = CARTESIAN_POINT ( 'NONE',  ( 6.944423797152706079, 31.55306878032414986, -11.16113333171310451 ) ) ;
#28044 = CARTESIAN_POINT ( 'NONE',  ( 105.6631189606246153, 114.1144967660473242, -51.29999999453763593 ) ) ;
#28045 = CARTESIAN_POINT ( 'NONE',  ( 143.5748159460630404, 40.65273437499998721, -5.622872871577873077 ) ) ;
#28046 = ORIENTED_EDGE ( 'NONE', *, *, #13761, .F. ) ;
#28047 = CARTESIAN_POINT ( 'NONE',  ( 107.0000000000000000, 110.0000000000000000, -55.49999999453763877 ) ) ;
#28048 = CARTESIAN_POINT ( 'NONE',  ( 13.14518615778179544, 40.35507812608393863, -1.609821015232357215E-15 ) ) ;
#28049 = CARTESIAN_POINT ( 'NONE',  ( 96.84719886470459471, 80.56250000136559208, 3.152801135295355994 ) ) ;
#28050 = CARTESIAN_POINT ( 'NONE',  ( 139.2950502721270425, 36.28710937608393294, -9.295050272127046043 ) ) ;
#28051 = CARTESIAN_POINT ( 'NONE',  ( 51.42518405393695957, 36.33671875216787583, 0.000000000000000000 ) ) ;
#28052 = CARTESIAN_POINT ( 'NONE',  ( 12.32011696698886816, 36.00000000000002842, -5.704949255836476496 ) ) ;
#28053 = CARTESIAN_POINT ( 'NONE',  ( 13.57481594606304931, 36.68398437716788152, 5.622872871577869525 ) ) ;
#28054 = AXIS2_PLACEMENT_3D ( 'NONE', #19444, #15290, #24007 ) ;
#28055 = CARTESIAN_POINT ( 'NONE',  ( 104.9999999999999574, -2.071067811865462627, 6.437499999999999112 ) ) ;
#28056 = CARTESIAN_POINT ( 'NONE',  ( 97.92893218813451028, 5.000000000000018652, 1.812500000000000000 ) ) ;
#28057 = CARTESIAN_POINT ( 'NONE',  ( 181.8548138422181921, 38.22187500108393010, 5.444914386472304635 ) ) ;
#28058 = LINE ( 'NONE', #261, #19287 ) ;
#28059 = ORIENTED_EDGE ( 'NONE', *, *, #24347, .F. ) ;
#28060 = DIRECTION ( 'NONE',  ( 1.156482317317871478E-16, 0.000000000000000000, 1.000000000000000000 ) ) ;
#28061 = CARTESIAN_POINT ( 'NONE',  ( 102.0710678118654329, 5.000000000000018652, 4.812500002731185056 ) ) ;
#28062 = DIRECTION ( 'NONE',  ( 0.000000000000000000, -1.000000000000000000, 0.000000000000000000 ) ) ;
#28063 = CARTESIAN_POINT ( 'NONE',  ( 65.00000000000000000, -7.395377635281828788, -7.517135062566165128E-15 ) ) ;
#28064 = CIRCLE ( 'NONE', #24874, 13.57481594606304398 ) ;
#28065 = CARTESIAN_POINT ( 'NONE',  ( -13.14518615778179544, 36.78320312608393294, 0.000000000000000000 ) ) ;
#28066 = CARTESIAN_POINT ( 'NONE',  ( 5.444914386472297529, 37.92421875108392726, -13.14518615778179900 ) ) ;
#28067 = CARTESIAN_POINT ( 'NONE',  ( 189.3771271284221314, 38.46992187499999716, -13.57481594606304753 ) ) ;
#28068 = CARTESIAN_POINT ( 'NONE',  ( 91.91746824999998466, 112.6261737610028320, -47.47500000273119269 ) ) ;
#28069 = CARTESIAN_POINT ( 'NONE',  ( 101.8468681455906903, -4.458734124999987891, 2.000000001365591640 ) ) ;
#28070 = CARTESIAN_POINT ( 'NONE',  ( 70.44491438647230552, 38.42031250108393436, 13.14518615778179189 ) ) ;
#28071 = ADVANCED_FACE ( 'NONE', ( #25469 ), #8073, .F. ) ;
#28072 = CARTESIAN_POINT ( 'NONE',  ( 95.54126587499996504, -1.846868145590724986, 1.500000001365591196 ) ) ;
#28073 = CARTESIAN_POINT ( 'NONE',  ( 93.00000000000001421, 107.7255621263696668, -44.40000000546238113 ) ) ;
#28074 = CARTESIAN_POINT ( 'NONE',  ( 95.54126587500000767, 91.81249999863440792, -7.484931351350258973E-15 ) ) ;
#28075 = AXIS2_PLACEMENT_3D ( 'NONE', #9225, #22346, #9085 ) ;
#28076 = CARTESIAN_POINT ( 'NONE',  ( -4.374022130817611931, 35.99999999999999289, 12.40367315690591887 ) ) ;
#28077 = CARTESIAN_POINT ( 'NONE',  ( -9.598844408820454532, 37.92421874999999432, 9.598844408820459861 ) ) ;
#28078 = CARTESIAN_POINT ( 'NONE',  ( 124.5550856135277087, 40.60312500108393863, -13.14518615778179900 ) ) ;
#28079 = ORIENTED_EDGE ( 'NONE', *, *, #2181, .F. ) ;
#28080 = CARTESIAN_POINT ( 'NONE',  ( 97.92893218813451028, 82.81250000000001421, -5.000000000000018652 ) ) ;
#28081 = CARTESIAN_POINT ( 'NONE',  ( 95.54126587500000767, 91.81249999863440792, -7.484931351350258973E-15 ) ) ;
#28082 = VERTEX_POINT ( 'NONE', #11921 ) ;
#28083 =( BOUNDED_CURVE ( )  B_SPLINE_CURVE ( 2, ( #18677, #18538, #10231, #25089, #20955, #18941, #16249 ),
 .UNSPECIFIED., .F., .T. ) 
 B_SPLINE_CURVE_WITH_KNOTS ( ( 3, 2, 2, 3 ),
 ( 0.7500000000000006661, 0.7750000000000004663, 0.8000000000000002665, 0.8250000005912452306 ),
 .UNSPECIFIED. ) 
 CURVE ( )  GEOMETRIC_REPRESENTATION_ITEM ( )  RATIONAL_B_SPLINE_CURVE ( ( 0.9999999999999980016, 0.9238795325112887369, 1.000000000000000000, 0.9238795325112867385, 1.000000000000000000, 0.9238795325112867385, 1.000000000000000000 ) ) 
 REPRESENTATION_ITEM ( '' )  );
#28084 = CARTESIAN_POINT ( 'NONE',  ( 94.33688103937534208, 114.1144967660473242, -45.20000000000000995 ) ) ;
#28085 = CARTESIAN_POINT ( 'NONE',  ( 55.70494972787295751, 35.09648437608393579, -9.295050272127046043 ) ) ;
#28086 = ORIENTED_EDGE ( 'NONE', *, *, #15861, .F. ) ;
#28087 = AXIS2_PLACEMENT_3D ( 'NONE', #27003, #13571, #26716 ) ;
#28088 = CARTESIAN_POINT ( 'NONE',  ( -5.622872871577736298, 36.88242187499999858, -13.57481594606318254 ) ) ;
#28089 = CARTESIAN_POINT ( 'NONE',  ( 103.1528011352953342, -3.152801135295355106, 1.062500001365592528 ) ) ;
#28090 = ORIENTED_EDGE ( 'NONE', *, *, #3570, .F. ) ;
#28091 = CYLINDRICAL_SURFACE ( 'NONE', #25715, 5.000000000000000888 ) ;
#28092 = CARTESIAN_POINT ( 'NONE',  ( -13.14518615778179544, 39.95820312608393010, 0.000000000000000000 ) ) ;
#28093 = CARTESIAN_POINT ( 'NONE',  ( 181.4251840539369596, 37.13046875216787868, 0.000000000000000000 ) ) ;
#28094 = CARTESIAN_POINT ( 'NONE',  ( -9.295050272127044266, 37.47773437608393010, 9.295050272127047819 ) ) ;
#28095 = CARTESIAN_POINT ( 'NONE',  ( 93.00000000000000000, 110.0000000000000000, -48.50000000546238255 ) ) ;
#28096 = CARTESIAN_POINT ( 'NONE',  ( 197.5295839951739651, 49.99999999938382444, 13.34625891065862291 ) ) ;
#28097 = CARTESIAN_POINT ( 'NONE',  ( 116.8548138422182205, 39.16445312608393436, 0.000000000000000000 ) ) ;
#28098 = ORIENTED_EDGE ( 'NONE', *, *, #6036, .F. ) ;
#28099 = CARTESIAN_POINT ( 'NONE',  ( -9.295050272127046043, 38.27148437608393294, -9.295050272127046043 ) ) ;
#28100 = CARTESIAN_POINT ( 'NONE',  ( 135.4449143864723055, 36.03906250108394005, 13.14518615778179189 ) ) ;
#28101 = CARTESIAN_POINT ( 'NONE',  ( 65.00000000000000000, 36.43593749999999432, 13.57481594606304576 ) ) ;
#28102 = CARTESIAN_POINT ( 'NONE',  ( 74.18017581364799184, 50.00000000000000000, 9.999999999999985789 ) ) ;
#28103 = CARTESIAN_POINT ( 'NONE',  ( 98.15313185440925281, -4.458734124999987891, 1.625000001365591640 ) ) ;
#28104 = DIRECTION ( 'NONE',  ( 5.782411586589358625E-17, -0.000000000000000000, 1.000000000000000000 ) ) ;
#28105 = CARTESIAN_POINT ( 'NONE',  ( 101.8468681455906903, 4.458734125000016313, 3.125000001365592528 ) ) ;
#28106 = CARTESIAN_POINT ( 'NONE',  ( 95.00472066334982912, 116.8754121666685393, -53.42500000273118843 ) ) ;
#28107 = CARTESIAN_POINT ( 'NONE',  ( 13.57481594606304576, 39.11484375216787157, -1.662435489736055892E-15 ) ) ;
#28108 = AXIS2_PLACEMENT_3D ( 'NONE', #4428, #13370, #11238 ) ;
#28109 = CARTESIAN_POINT ( 'NONE',  ( 99.99999999999998579, 130.0000000000000000, 10.50000000000001066 ) ) ;
#28110 = CARTESIAN_POINT ( 'NONE',  ( 6.944423797152705191, 31.55306878032414986, -11.16113333171310451 ) ) ;
#28111 = CARTESIAN_POINT ( 'NONE',  ( -8.049105076161786076E-16, 40.55351562608393579, -13.14518615778179544 ) ) ;
#28112 = ORIENTED_EDGE ( 'NONE', *, *, #23634, .T. ) ;
#28113 = EDGE_CURVE ( 'NONE', #12986, #5360, #23710, .T. ) ;
#28114 = CARTESIAN_POINT ( 'NONE',  ( 102.0669872999999797, 123.5500000010924708, -9.794112055954760458E-15 ) ) ;
#28115 = FACE_OUTER_BOUND ( 'NONE', #26020, .T. ) ;
#28116 = FACE_OUTER_BOUND ( 'NONE', #10266, .T. ) ;
#28117 = CARTESIAN_POINT ( 'NONE',  ( 200.4449143864723055, 38.71796875108393721, -13.14518615778179900 ) ) ;
#28118 = ORIENTED_EDGE ( 'NONE', *, *, #6873, .T. ) ;
#28119 = CARTESIAN_POINT ( 'NONE',  ( 65.00000000000000000, 36.18789062608393436, 13.14518615778179544 ) ) ;
#28120 = DIRECTION ( 'NONE',  ( 0.000000000000000000, 0.000000000000000000, -1.000000000000000000 ) ) ;
#28121 = CARTESIAN_POINT ( 'NONE',  ( 96.84719886470459471, 3.152801135295383084, 14.56250000136559208 ) ) ;
#28122 = B_SPLINE_CURVE_WITH_KNOTS ( 'NONE', 3,
 ( #17259, #25959, #15101, #4023, #19123, #4301, #6564, #3744, #27830, #8151, #21126, #1612, #10270, #18979, #27688, #16844, #6022, #6156, #14685, #23405, #739, #2866, #6846, #13680, #22114, #24384, #17540, #10970, #26532, #24244, #595 ),
 .UNSPECIFIED., .F., .F.,
 ( 4, 2, 2, 2, 2, 2, 2, 2, 2, 2, 1, 2, 2, 2, 2, 4 ),
 ( 1.256496749369840159E-15, 0.001647793485001787040, 0.003295586970002317272, 0.004943380455002847722, 0.005767277197503111429, 0.006591173940003375135, 0.008238967425003898212, 0.009886760910004423891, 0.01318234788000547872, 0.01483014136500602695, 0.01647793485000657518, 0.01812572833500712341, 0.01977352182000766817, 0.02306910879000876810, 0.02471690227500932674, 0.02636469576000988191 ),
 .UNSPECIFIED. ) ;
#28123 = ORIENTED_EDGE ( 'NONE', *, *, #8313, .F. ) ;
#28124 = CARTESIAN_POINT ( 'NONE',  ( 97.83688103937537051, 103.3426043859339103, -53.60000000000000853 ) ) ;
#28125 = CARTESIAN_POINT ( 'NONE',  ( 13.14518615778179544, 39.36289062608393152, -1.609821015232357215E-15 ) ) ;
#28126 = CARTESIAN_POINT ( 'NONE',  ( 100.8561741729129295, 124.2000000010924907, 2.066987299999979211 ) ) ;
#28127 = CARTESIAN_POINT ( 'NONE',  ( 130.0000000000000000, 32.96328125216787441, -13.57481594606304576 ) ) ;
#28128 = CARTESIAN_POINT ( 'NONE',  ( 204.5988444088204403, 40.70234374999999716, -9.598844408820458085 ) ) ;
#28129 = CARTESIAN_POINT ( 'NONE',  ( 189.3771271284222166, 40.85117187499999147, -13.57481594606315412 ) ) ;
#28130 = DIRECTION ( 'NONE',  ( 5.782411586589358625E-17, -0.000000000000000000, 1.000000000000000000 ) ) ;
#28131 = CARTESIAN_POINT ( 'NONE',  ( 200.4449143864723055, 33.36015625108393579, -13.14518615778179900 ) ) ;
#28132 = ORIENTED_EDGE ( 'NONE', *, *, #9309, .F. ) ;
#28133 = ORIENTED_EDGE ( 'NONE', *, *, #12967, .F. ) ;
#28134 = CARTESIAN_POINT ( 'NONE',  ( -5.444914386472297529, 39.01562500108394005, -13.14518615778179900 ) ) ;
#28135 = CARTESIAN_POINT ( 'NONE',  ( 0.000000000000000000, 0.000000000000000000, 0.000000000000000000 ) ) ;
#28136 = CARTESIAN_POINT ( 'NONE',  ( 104.4587341249999639, 1.442382525525748735E-14, 10.18750000136559208 ) ) ;
#28137 = EDGE_CURVE ( 'NONE', #7853, #23118, #13021, .T. ) ;
#28138 = CARTESIAN_POINT ( 'NONE',  ( 99.99999999999998579, 124.7999999999999972, -2.499999999999997780 ) ) ;
#28139 = CARTESIAN_POINT ( 'NONE',  ( 181.8548138422182205, 39.75976562608393294, 0.000000000000000000 ) ) ;
#28140 = CARTESIAN_POINT ( 'NONE',  ( -13.14518615778179544, 39.95820312608393010, 0.000000000000000000 ) ) ;
#28141 = CARTESIAN_POINT ( 'NONE',  ( 84.99999999999998579, 123.0000000000000000, 14.99999999999999112 ) ) ;
#28142 = CARTESIAN_POINT ( 'NONE',  ( 97.92893218813451028, -4.999999999999989342, 12.18750000000000000 ) ) ;
#28143 = DIRECTION ( 'NONE',  ( -0.000000000000000000, -1.000000000000000000, -0.000000000000000000 ) ) ;
#28144 = CARTESIAN_POINT ( 'NONE',  ( 108.0825317500000011, 110.0000000000000000, -52.62499999726882294 ) ) ;
#28145 = EDGE_CURVE ( 'NONE', #26695, #24077, #21758, .T. ) ;
#28146 = VECTOR ( 'NONE', #15354, 1000.000000000000000 ) ;
#28147 = VERTEX_POINT ( 'NONE', #12609 ) ;
#28148 = CARTESIAN_POINT ( 'NONE',  ( 5.622872871577871301, 37.57695312499998863, -13.57481594606304753 ) ) ;
#28149 = CARTESIAN_POINT ( 'NONE',  ( 13.14518615778179900, 37.03125000108393294, -5.444914386472297529 ) ) ;
#28150 = CARTESIAN_POINT ( 'NONE',  ( 96.46446609406721961, 3.535533905932755072, 1.000000002731185944 ) ) ;
#28151 = CARTESIAN_POINT ( 'NONE',  ( 116.8548138422182063, 37.52734375108393294, -5.444914386472297529 ) ) ;
#28152 = CARTESIAN_POINT ( 'NONE',  ( 51.85481384221819923, 32.56640625108394005, -5.444914386472297529 ) ) ;
#28153 = EDGE_CURVE ( 'NONE', #11809, #13376, #26162, .T. ) ;
#28154 = CARTESIAN_POINT ( 'NONE',  ( 200.4449143864723055, 38.12265625108393152, -13.14518615778179900 ) ) ;
#28155 = CARTESIAN_POINT ( 'NONE',  ( 105.6631189606246295, 105.8855032339526758, -45.70000000546237828 ) ) ;
#28156 = CARTESIAN_POINT ( 'NONE',  ( 5.444914386472302859, 33.65781250108393152, 13.14518615778179189 ) ) ;
#28157 = CARTESIAN_POINT ( 'NONE',  ( 121.7985538123451477, 50.69246985423282581, -14.99999999999510791 ) ) ;
#28158 = DIRECTION ( 'NONE',  ( -0.000000000000000000, -1.000000000000000000, -0.000000000000000000 ) ) ;
#28159 = CARTESIAN_POINT ( 'NONE',  ( -8.049105076161786076E-16, 33.40976562608393863, -13.14518615778179544 ) ) ;
#28160 = CARTESIAN_POINT ( 'NONE',  ( 102.4976396683250925, 117.6869444889999841, -51.72500000273119980 ) ) ;
#28161 = CARTESIAN_POINT ( 'NONE',  ( 13.14518615778179900, 34.65000000108393152, -5.444914386472297529 ) ) ;
#28162 = ORIENTED_EDGE ( 'NONE', *, *, #22456, .T. ) ;
#28163 = CARTESIAN_POINT ( 'NONE',  ( -13.57481594606304576, 34.64999999999999147, 0.000000000000000000 ) ) ;
#28164 = CARTESIAN_POINT ( 'NONE',  ( 102.0710678118654897, 79.81250000273122680, -4.999999999999968914 ) ) ;
#28165 = VECTOR ( 'NONE', #16559, 1000.000000000000000 ) ;
#28166 = CARTESIAN_POINT ( 'NONE',  ( 2.493653234604083739E-15, 36.53515625216787299, 13.57481594606304576 ) ) ;
#28167 = CIRCLE ( 'NONE', #11773, 16.91709623134523000 ) ;
#28168 = CARTESIAN_POINT ( 'NONE',  ( 104.4587341249999781, 1.846868145590750299, 9.000000001365593860 ) ) ;
#28169 = CARTESIAN_POINT ( 'NONE',  ( 99.99999999999995737, 85.00000000000000000, -3.000000000000018208 ) ) ;
#28170 = CARTESIAN_POINT ( 'NONE',  ( 101.8468681455906903, 4.458734125000016313, 13.12500000136559208 ) ) ;
#28171 = CARTESIAN_POINT ( 'NONE',  ( 126.1360747348882825, 54.10645156199843342, 14.99999999999996803 ) ) ;
#28172 = CARTESIAN_POINT ( 'NONE',  ( 2.414731522848535132E-15, 39.16445312608392726, 13.14518615778179544 ) ) ;
#28173 = CARTESIAN_POINT ( 'NONE',  ( -8.312177448680279460E-16, 32.86406249999999574, -13.57481594606304576 ) ) ;
#28174 = CARTESIAN_POINT ( 'NONE',  ( 101.8468681455906903, 80.37500000136562051, -4.458734125000016313 ) ) ;
#28175 = CARTESIAN_POINT ( 'NONE',  ( 59.55508561352770158, 34.55078125108393294, 13.14518615778179722 ) ) ;
#28176 = CARTESIAN_POINT ( 'NONE',  ( 106.5389055433251002, 114.7507929638356785, -49.92500000273119554 ) ) ;
#28177 = DIRECTION ( 'NONE',  ( 5.782411586589357392E-17, -0.000000000000000000, 1.000000000000000000 ) ) ;
#28178 = DIRECTION ( 'NONE',  ( 0.8660254037844418162, 0.000000000000000000, 0.4999999999999947264 ) ) ;
#28179 = CARTESIAN_POINT ( 'NONE',  ( 2.493653234604083739E-15, 40.40468749999999432, 13.57481594606304576 ) ) ;
#28180 = CARTESIAN_POINT ( 'NONE',  ( 105.6631189606246295, 105.8855032339526758, -55.69999999453764161 ) ) ;
#28181 = CARTESIAN_POINT ( 'NONE',  ( 120.7049497278729575, 31.92148437608393508, -9.295050272127046043 ) ) ;
#28182 = EDGE_CURVE ( 'NONE', #13527, #19588, #18047, .T. ) ;
#28183 = ORIENTED_EDGE ( 'NONE', *, *, #21706, .T. ) ;
#28184 = CARTESIAN_POINT ( 'NONE',  ( 102.1631189606246295, 103.3426043859339103, -55.89999999453763735 ) ) ;
#28185 = CARTESIAN_POINT ( 'NONE',  ( 2.414731522848535132E-15, 37.77539062608393294, 13.14518615778179544 ) ) ;
#28186 = CARTESIAN_POINT ( 'NONE',  ( 9.598844408820456309, 36.83281250216787583, -9.598844408820458085 ) ) ;
#28187 = CARTESIAN_POINT ( 'NONE',  ( 116.8548138422182063, 35.04687500108393294, 5.444914386472304635 ) ) ;
#28188 = CARTESIAN_POINT ( 'NONE',  ( 55.40115559117954547, 32.46718750216787441, 9.598844408820459861 ) ) ;
#28189 = CYLINDRICAL_SURFACE ( 'NONE', #13862, 2.500000000000008882 ) ;
#28190 = VECTOR ( 'NONE', #25187, 1000.000000000000000 ) ;
#28191 = CARTESIAN_POINT ( 'NONE',  ( -13.57481594606304753, 35.49335937716787015, -5.622872871577873077 ) ) ;
#28192 = AXIS2_PLACEMENT_3D ( 'NONE', #23581, #1787, #10733 ) ;
#28193 = CARTESIAN_POINT ( 'NONE',  ( 94.99999999999995737, 2.071067811865491048, 3.937500000000000000 ) ) ;
#28194 = VERTEX_POINT ( 'NONE', #15027 ) ;
#28195 = CARTESIAN_POINT ( 'NONE',  ( 181.8548138422181921, 37.42812500108393436, 5.444914386472304635 ) ) ;
#28196 = DIRECTION ( 'NONE',  ( 1.000000000000000000, 0.000000000000000000, 0.000000000000000000 ) ) ;
#28197 = CARTESIAN_POINT ( 'NONE',  ( 143.1451861577818363, 36.13828125108393152, 5.444914386472293977 ) ) ;
#28198 = EDGE_LOOP ( 'NONE', ( #19056, #11237, #27348, #26216 ) ) ;
#28199 = CARTESIAN_POINT ( 'NONE',  ( 189.3771271284221598, 38.07304687716787583, 13.57481594606308128 ) ) ;
#28200 = DIRECTION ( 'NONE',  ( 0.000000000000000000, 0.000000000000000000, 1.000000000000000000 ) ) ;
#28201 = CARTESIAN_POINT ( 'NONE',  ( 0.000000000000000000, 50.00000000000000000, 0.000000000000000000 ) ) ;
#28202 = CARTESIAN_POINT ( 'NONE',  ( 13.57481594606304931, 38.17226562499999432, 5.622872871577869525 ) ) ;
#28203 = CARTESIAN_POINT ( 'NONE',  ( 116.4251840539369596, 40.30546875216787583, 0.000000000000000000 ) ) ;
#28204 = NEXT_ASSEMBLY_USAGE_OCCURRENCE ( 'NAUO1', ' ', ' ', #21636, #9428, $ ) ;
#28205 = NEXT_ASSEMBLY_USAGE_OCCURRENCE ( 'NAUO2', ' ', ' ', #21636, #27055, $ ) ;
#28206 = NEXT_ASSEMBLY_USAGE_OCCURRENCE ( 'NAUO3', ' ', ' ', #21636, #24593, $ ) ;
#28207 = NEXT_ASSEMBLY_USAGE_OCCURRENCE ( 'NAUO4', ' ', ' ', #21636, #13233, $ ) ;
#28208 = NEXT_ASSEMBLY_USAGE_OCCURRENCE ( 'NAUO5', ' ', ' ', #21636, #10642, $ ) ;
#28209 = NEXT_ASSEMBLY_USAGE_OCCURRENCE ( 'NAUO6', ' ', ' ', #21636, #22512, $ ) ;
#28210 = NEXT_ASSEMBLY_USAGE_OCCURRENCE ( 'NAUO7', ' ', ' ', #21636, #27055, $ ) ;
#28211 = NEXT_ASSEMBLY_USAGE_OCCURRENCE ( 'NAUO8', ' ', ' ', #21636, #27055, $ ) ;
#28212 = NEXT_ASSEMBLY_USAGE_OCCURRENCE ( 'NAUO9', ' ', ' ', #21636, #27055, $ ) ;
#28213 = NEXT_ASSEMBLY_USAGE_OCCURRENCE ( 'NAUO10', ' ', ' ', #21636, #9428, $ ) ;
#28214 = NEXT_ASSEMBLY_USAGE_OCCURRENCE ( 'NAUO11', ' ', ' ', #21636, #9428, $ ) ;
#28215 = NEXT_ASSEMBLY_USAGE_OCCURRENCE ( 'NAUO12', ' ', ' ', #21636, #9428, $ ) ;
#28216 = NEXT_ASSEMBLY_USAGE_OCCURRENCE ( 'NAUO13', ' ', ' ', #21636, #2652, $ ) ;
ENDSEC;
END-ISO-10303-21;
